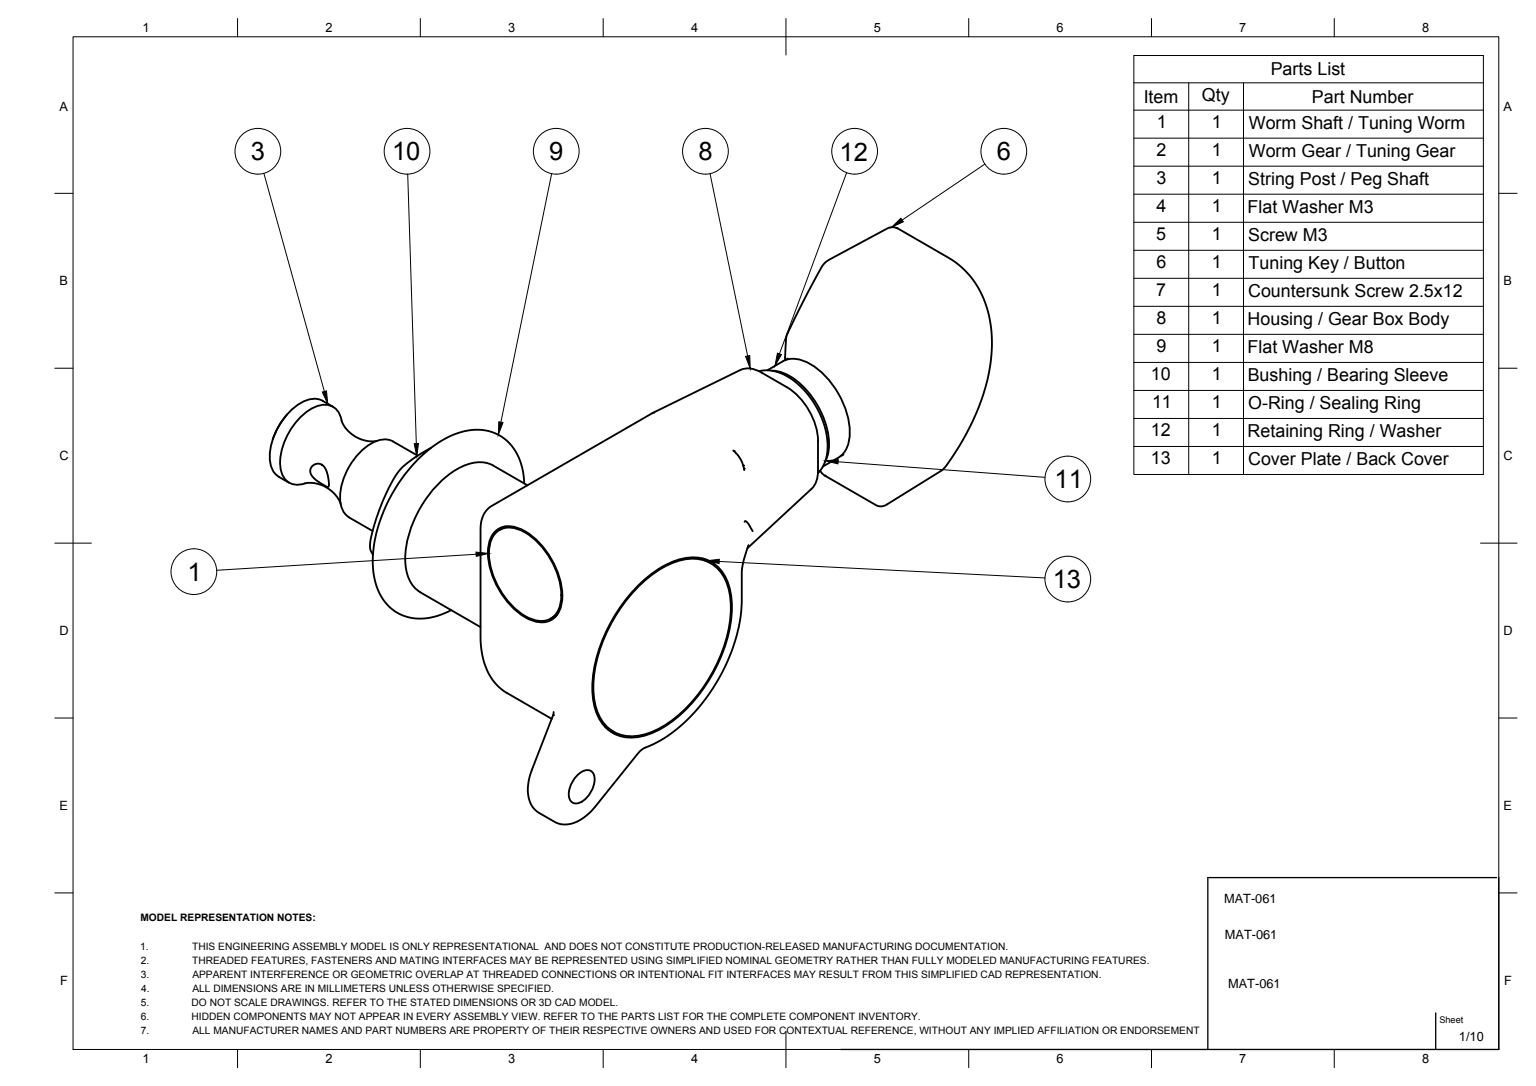
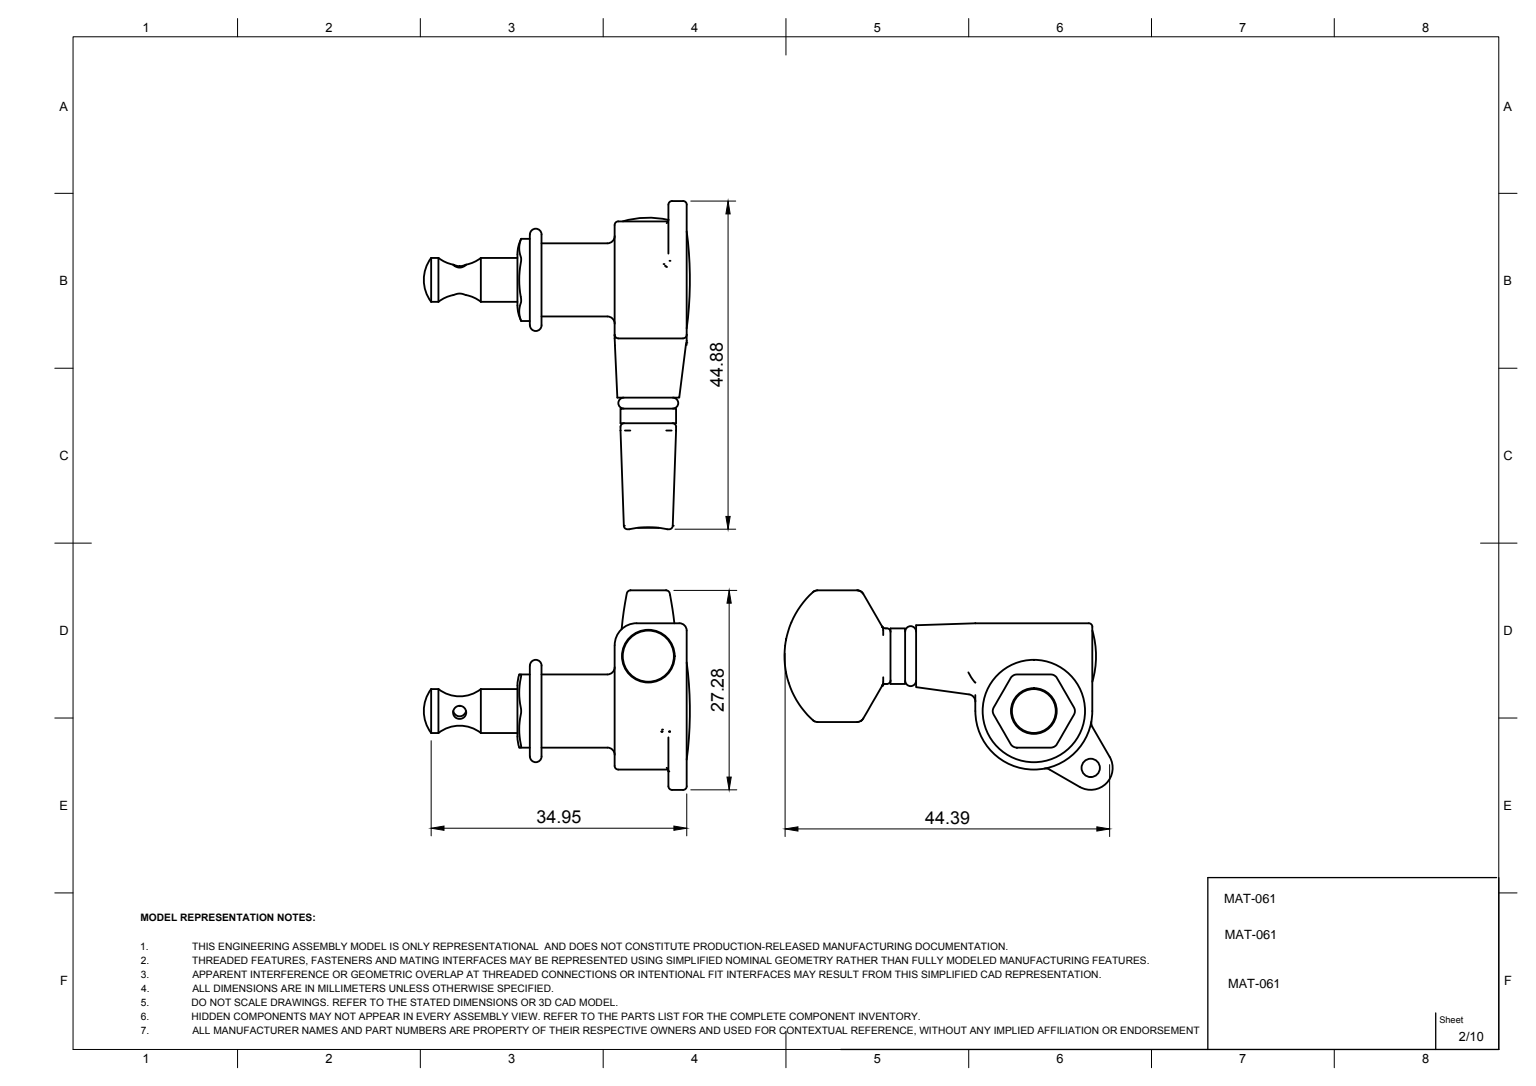
ISO-10303-21;
HEADER;
/* Generated by software containing ST-Developer
 * from STEP Tools, Inc. (www.steptools.com) 
 */

FILE_DESCRIPTION(
/* description */ ('', 'CAx-IF Rec.Pracs.---Representation and Presentation of Product Manufa
cturing Information (PMI)---4.0---2014-10-13'),
/* implementation_level */ '2;1');

FILE_NAME(
/* name */ 'MAT-061',
/* time_stamp */ '2026-10-28T14:45:12+01:00',
/* author */ (''),
/* organization */ (''),
/* preprocessor_version */ 'ST-DEVELOPER v20.2',
/* originating_system */ 'Autodesk Translation Framework v15.17.0.0',
/* authorisation */ '');

FILE_SCHEMA (('AP242_MANAGED_MODEL_BASED_3D_ENGINEERING_MIM_LF { 1 0 10303 442 2 1 4 }'));
ENDSEC;

DATA;
#10=MECHANICAL_DESIGN_GEOMETRIC_PRESENTATION_REPRESENTATION('',(#258,#259,
#260,#261,#262,#263,#264,#265,#266,#267,#268,#269,#270),#52164);
#11=ITEM_DEFINED_TRANSFORMATION($,$,#9276,#10197);
#12=ITEM_DEFINED_TRANSFORMATION($,$,#9302,#10198);
#13=ITEM_DEFINED_TRANSFORMATION($,$,#9667,#10199);
#14=ITEM_DEFINED_TRANSFORMATION($,$,#9694,#10200);
#15=ITEM_DEFINED_TRANSFORMATION($,$,#9704,#10201);
#16=ITEM_DEFINED_TRANSFORMATION($,$,#9776,#10202);
#17=ITEM_DEFINED_TRANSFORMATION($,$,#9921,#10203);
#18=ITEM_DEFINED_TRANSFORMATION($,$,#9987,#10204);
#19=ITEM_DEFINED_TRANSFORMATION($,$,#10132,#10205);
#20=ITEM_DEFINED_TRANSFORMATION($,$,#10142,#10206);
#21=ITEM_DEFINED_TRANSFORMATION($,$,#10171,#10207);
#22=ITEM_DEFINED_TRANSFORMATION($,$,#10175,#10208);
#23=ITEM_DEFINED_TRANSFORMATION($,$,#10184,#10209);
#24=(
REPRESENTATION_RELATIONSHIP($,$,#52211,#52210)
REPRESENTATION_RELATIONSHIP_WITH_TRANSFORMATION(#11)
SHAPE_REPRESENTATION_RELATIONSHIP()
);
#25=(
REPRESENTATION_RELATIONSHIP($,$,#52212,#52210)
REPRESENTATION_RELATIONSHIP_WITH_TRANSFORMATION(#12)
SHAPE_REPRESENTATION_RELATIONSHIP()
);
#26=(
REPRESENTATION_RELATIONSHIP($,$,#52213,#52210)
REPRESENTATION_RELATIONSHIP_WITH_TRANSFORMATION(#13)
SHAPE_REPRESENTATION_RELATIONSHIP()
);
#27=(
REPRESENTATION_RELATIONSHIP($,$,#52214,#52210)
REPRESENTATION_RELATIONSHIP_WITH_TRANSFORMATION(#14)
SHAPE_REPRESENTATION_RELATIONSHIP()
);
#28=(
REPRESENTATION_RELATIONSHIP($,$,#52215,#52210)
REPRESENTATION_RELATIONSHIP_WITH_TRANSFORMATION(#15)
SHAPE_REPRESENTATION_RELATIONSHIP()
);
#29=(
REPRESENTATION_RELATIONSHIP($,$,#52216,#52210)
REPRESENTATION_RELATIONSHIP_WITH_TRANSFORMATION(#16)
SHAPE_REPRESENTATION_RELATIONSHIP()
);
#30=(
REPRESENTATION_RELATIONSHIP($,$,#52217,#52210)
REPRESENTATION_RELATIONSHIP_WITH_TRANSFORMATION(#17)
SHAPE_REPRESENTATION_RELATIONSHIP()
);
#31=(
REPRESENTATION_RELATIONSHIP($,$,#52218,#52210)
REPRESENTATION_RELATIONSHIP_WITH_TRANSFORMATION(#18)
SHAPE_REPRESENTATION_RELATIONSHIP()
);
#32=(
REPRESENTATION_RELATIONSHIP($,$,#52219,#52210)
REPRESENTATION_RELATIONSHIP_WITH_TRANSFORMATION(#19)
SHAPE_REPRESENTATION_RELATIONSHIP()
);
#33=(
REPRESENTATION_RELATIONSHIP($,$,#52220,#52210)
REPRESENTATION_RELATIONSHIP_WITH_TRANSFORMATION(#20)
SHAPE_REPRESENTATION_RELATIONSHIP()
);
#34=(
REPRESENTATION_RELATIONSHIP($,$,#52221,#52210)
REPRESENTATION_RELATIONSHIP_WITH_TRANSFORMATION(#21)
SHAPE_REPRESENTATION_RELATIONSHIP()
);
#35=(
REPRESENTATION_RELATIONSHIP($,$,#52222,#52210)
REPRESENTATION_RELATIONSHIP_WITH_TRANSFORMATION(#22)
SHAPE_REPRESENTATION_RELATIONSHIP()
);
#36=(
REPRESENTATION_RELATIONSHIP($,$,#52223,#52210)
REPRESENTATION_RELATIONSHIP_WITH_TRANSFORMATION(#23)
SHAPE_REPRESENTATION_RELATIONSHIP()
);
#37=CONTEXT_DEPENDENT_SHAPE_REPRESENTATION(#24,#52197);
#38=CONTEXT_DEPENDENT_SHAPE_REPRESENTATION(#25,#52198);
#39=CONTEXT_DEPENDENT_SHAPE_REPRESENTATION(#26,#52199);
#40=CONTEXT_DEPENDENT_SHAPE_REPRESENTATION(#27,#52200);
#41=CONTEXT_DEPENDENT_SHAPE_REPRESENTATION(#28,#52201);
#42=CONTEXT_DEPENDENT_SHAPE_REPRESENTATION(#29,#52202);
#43=CONTEXT_DEPENDENT_SHAPE_REPRESENTATION(#30,#52203);
#44=CONTEXT_DEPENDENT_SHAPE_REPRESENTATION(#31,#52204);
#45=CONTEXT_DEPENDENT_SHAPE_REPRESENTATION(#32,#52205);
#46=CONTEXT_DEPENDENT_SHAPE_REPRESENTATION(#33,#52206);
#47=CONTEXT_DEPENDENT_SHAPE_REPRESENTATION(#34,#52207);
#48=CONTEXT_DEPENDENT_SHAPE_REPRESENTATION(#35,#52208);
#49=CONTEXT_DEPENDENT_SHAPE_REPRESENTATION(#36,#52209);
#50=NEXT_ASSEMBLY_USAGE_OCCURRENCE('Worm Shaft / Tuning Worm:1',
'Worm Shaft / Tuning Worm:1','Worm Shaft / Tuning Worm:1',#52225,#52226,
'Worm Shaft / Tuning Worm:1');
#51=NEXT_ASSEMBLY_USAGE_OCCURRENCE('Worm Gear / Tuning Gear:1',
'Worm Gear / Tuning Gear:1','Worm Gear / Tuning Gear:1',#52225,#52227,
'Worm Gear / Tuning Gear:1');
#52=NEXT_ASSEMBLY_USAGE_OCCURRENCE('String Post / Peg Shaft:1',
'String Post / Peg Shaft:1','String Post / Peg Shaft:1',#52225,#52228,
'String Post / Peg Shaft:1');
#53=NEXT_ASSEMBLY_USAGE_OCCURRENCE('Flat Washer M3:1',
'Flat Washer M3:1','Flat Washer M3:1',#52225,#52229,'Flat Washer M3:1');
#54=NEXT_ASSEMBLY_USAGE_OCCURRENCE('Screw M3:1','Screw M3:1',
'Screw M3:1',#52225,#52230,'Screw M3:1');
#55=NEXT_ASSEMBLY_USAGE_OCCURRENCE('Tuning Key / Button:1',
'Tuning Key / Button:1','Tuning Key / Button:1',#52225,#52231,
'Tuning Key / Button:1');
#56=NEXT_ASSEMBLY_USAGE_OCCURRENCE('Countersunk Screw 2.5x12:1',
'Countersunk Screw 2.5x12:1','Countersunk Screw 2.5x12:1',#52225,#52232,
'Countersunk Screw 2.5x12:1');
#57=NEXT_ASSEMBLY_USAGE_OCCURRENCE('Housing / Gear Box Body:1',
'Housing / Gear Box Body:1','Housing / Gear Box Body:1',#52225,#52233,
'Housing / Gear Box Body:1');
#58=NEXT_ASSEMBLY_USAGE_OCCURRENCE('Flat Washer M8:1',
'Flat Washer M8:1','Flat Washer M8:1',#52225,#52234,'Flat Washer M8:1');
#59=NEXT_ASSEMBLY_USAGE_OCCURRENCE('Bushing / Bearing Sleeve:1',
'Bushing / Bearing Sleeve:1','Bushing / Bearing Sleeve:1',#52225,#52235,
'Bushing / Bearing Sleeve:1');
#60=NEXT_ASSEMBLY_USAGE_OCCURRENCE('O-Ring / Sealing Ring:1',
'O-Ring / Sealing Ring:1','O-Ring / Sealing Ring:1',#52225,#52236,
'O-Ring / Sealing Ring:1');
#61=NEXT_ASSEMBLY_USAGE_OCCURRENCE('Retaining Ring / Washer:1',
'Retaining Ring / Washer:1','Retaining Ring / Washer:1',#52225,#52237,
'Retaining Ring / Washer:1');
#62=NEXT_ASSEMBLY_USAGE_OCCURRENCE('Cover Plate / Back Cover:1',
'Cover Plate / Back Cover:1','Cover Plate / Back Cover:1',#52225,#52238,
'Cover Plate / Back Cover:1');
#63=(
BOUNDED_CURVE()
B_SPLINE_CURVE(2,(#29010,#29011,#29012),.UNSPECIFIED.,.F.,.F.)
B_SPLINE_CURVE_WITH_KNOTS((3,3),(-1.41025055977478,-0.304692654014095),
 .UNSPECIFIED.)
CURVE()
GEOMETRIC_REPRESENTATION_ITEM()
RATIONAL_B_SPLINE_CURVE((0.957089080441345,0.830796931423118,1.))
REPRESENTATION_ITEM('')
);
#64=(
BOUNDED_CURVE()
B_SPLINE_CURVE(2,(#46348,#46349,#46350),.UNSPECIFIED.,.F.,.F.)
B_SPLINE_CURVE_WITH_KNOTS((3,3),(1.23956041519017,1.57079632679222),
 .UNSPECIFIED.)
CURVE()
GEOMETRIC_REPRESENTATION_ITEM()
RATIONAL_B_SPLINE_CURVE((0.987875274923375,0.980288238878012,1.))
REPRESENTATION_ITEM('')
);
#65=ELLIPSE('',#9725,0.771415586451778,0.0652711480392958);
#66=ELLIPSE('',#9726,0.771415586451778,0.0652711480392958);
#67=ELLIPSE('',#9729,0.771415586459596,0.0652711480406291);
#68=ELLIPSE('',#9733,0.251906298612587,0.25);
#69=ELLIPSE('',#9735,0.251906298612587,0.25);
#70=ELLIPSE('',#9736,0.251906298612587,0.25);
#71=ELLIPSE('',#9737,0.251906298612587,0.25);
#72=ELLIPSE('',#9738,0.251906298612587,0.25);
#73=ELLIPSE('',#9739,0.251906298612587,0.25);
#74=ELLIPSE('',#9740,0.251906298612587,0.25);
#75=ELLIPSE('',#9741,0.251906298612587,0.25);
#76=ELLIPSE('',#9742,0.251906298612587,0.25);
#77=ELLIPSE('',#9743,0.251906298612587,0.25);
#78=ELLIPSE('',#9744,0.251906298612587,0.25);
#79=ELLIPSE('',#9745,0.251906298612587,0.25);
#80=ELLIPSE('',#9748,0.251906298612587,0.25);
#81=ELLIPSE('',#9750,0.251906298612587,0.25);
#82=ELLIPSE('',#9752,0.251906298612587,0.25);
#83=ELLIPSE('',#9754,0.251906298612587,0.25);
#84=ELLIPSE('',#9778,3.41583409365519,0.299010553745989);
#85=ELLIPSE('',#9779,1.15925578938865,0.129764384341253);
#86=ELLIPSE('',#9810,58.0067380360385,50.6192841142981);
#87=ELLIPSE('',#9813,1.18656669130194,0.53832789407732);
#88=ELLIPSE('',#9814,2.36619692333918,0.2327676175482);
#89=ELLIPSE('',#9837,58.0426595105096,50.6800723424155);
#90=ELLIPSE('',#9844,57.8529892126302,50.3590102148563);
#91=ELLIPSE('',#9882,57.6813518726037,50.0696217347841);
#92=ELLIPSE('',#9924,0.251906298612587,0.25);
#93=ELLIPSE('',#9925,0.251906298612587,0.25);
#94=ELLIPSE('',#9926,0.251906298612587,0.25);
#95=ELLIPSE('',#9927,0.251906298612587,0.25);
#96=ELLIPSE('',#9928,0.251906298612587,0.25);
#97=ELLIPSE('',#9929,0.251906298612587,0.25);
#98=ELLIPSE('',#9930,0.251906298612587,0.25);
#99=ELLIPSE('',#9931,0.251906298612587,0.25);
#100=ELLIPSE('',#9932,0.251906298612587,0.25);
#101=ELLIPSE('',#9933,0.251906298612587,0.25);
#102=ELLIPSE('',#9934,0.251906298612587,0.25);
#103=ELLIPSE('',#9935,0.251906298612587,0.25);
#104=ELLIPSE('',#9951,0.251906298612587,0.25);
#105=ELLIPSE('',#9954,0.251906298612587,0.25);
#106=ELLIPSE('',#9955,0.251906298612587,0.25);
#107=ELLIPSE('',#9956,0.251906298612587,0.25);
#108=ELLIPSE('',#9957,0.251906298612587,0.25);
#109=ELLIPSE('',#9958,0.251906298612587,0.25);
#110=ELLIPSE('',#9959,0.251906298612587,0.25);
#111=ELLIPSE('',#9960,0.251906298612587,0.25);
#112=ELLIPSE('',#9961,0.251906298612587,0.25);
#113=ELLIPSE('',#9962,0.251906298612587,0.25);
#114=ELLIPSE('',#9963,0.251906298612587,0.25);
#115=ELLIPSE('',#9964,0.251906298612587,0.25);
#116=ELLIPSE('',#10069,3.09185060411887,2.99998911300292);
#117=ELLIPSE('',#10070,0.558356536433831,0.540529130211527);
#118=ELLIPSE('',#10075,3.02534560825415,3.);
#119=ELLIPSE('',#10096,3.05201365986006,3.);
#120=ELLIPSE('',#10097,3.03164154875039,3.);
#121=ELLIPSE('',#10098,3.00479269659654,3.);
#122=ELLIPSE('',#10104,3.05599112671771,2.99998273953943);
#123=ELLIPSE('',#10106,0.477842904086099,0.430473129723059);
#124=ELLIPSE('',#10110,0.470434252195438,0.436250539297532);
#125=ELLIPSE('',#10111,0.502233427925589,0.501933027798313);
#126=ELLIPSE('',#10115,0.0333294784166319,0.012380355937192);
#127=(
BOUNDED_SURFACE()
B_SPLINE_SURFACE(2,2,((#28929,#28930,#28931,#28932,#28933,#28934,#28935,
#28936,#28937),(#28938,#28939,#28940,#28941,#28942,#28943,#28944,#28945,
#28946),(#28947,#28948,#28949,#28950,#28951,#28952,#28953,#28954,#28955)),
 .UNSPECIFIED.,.F.,.T.,.F.)
B_SPLINE_SURFACE_WITH_KNOTS((3,3),(3,2,2,2,3),(0.304692654014095,1.57079632680149),
(-3.14159265358979,-1.5707963267949,0.,1.5707963267949,3.14159265358979),
 .UNSPECIFIED.)
GEOMETRIC_REPRESENTATION_ITEM()
RATIONAL_B_SPLINE_SURFACE(((1.,0.707106781186548,1.,0.707106781186548,1.,
0.707106781186548,1.,0.707106781186548,1.),(0.806225774827519,0.570087712547917,
0.806225774827519,0.570087712547917,0.806225774827519,0.570087712547917,
0.806225774827519,0.570087712547917,0.806225774827519),(1.,0.707106781186548,
1.,0.707106781186548,1.,0.707106781186548,1.,0.707106781186548,1.)))
REPRESENTATION_ITEM('')
SURFACE()
);
#128=(
BOUNDED_SURFACE()
B_SPLINE_SURFACE(3,3,((#29423,#29424,#29425,#29426,#29427,#29428,#29429,
#29430,#29431,#29432,#29433),(#29434,#29435,#29436,#29437,#29438,#29439,
#29440,#29441,#29442,#29443,#29444),(#29445,#29446,#29447,#29448,#29449,
#29450,#29451,#29452,#29453,#29454,#29455),(#29456,#29457,#29458,#29459,
#29460,#29461,#29462,#29463,#29464,#29465,#29466)),.UNSPECIFIED.,.F.,.F.,
 .F.)
B_SPLINE_SURFACE_WITH_KNOTS((4,4),(4,1,1,1,1,1,1,1,4),(0.,1.),(-0.02986974742742,
0.,0.1596527875626,0.3152888236561,0.4716393647845,0.6325142775716,0.8056128321368,
1.,1.030037265102),.UNSPECIFIED.)
GEOMETRIC_REPRESENTATION_ITEM()
RATIONAL_B_SPLINE_SURFACE(((1.021500558569,1.021500558569,1.021500558569,
1.021500558569,1.021500558569,1.021500558569,1.021500558569,1.021500558569,
1.021500558569,1.021500558569,1.021500558569),(0.9928331471435,0.9928331471435,
0.9928331471435,0.9928331471435,0.9928331471435,0.9928331471435,0.9928331471435,
0.9928331471435,0.9928331471435,0.9928331471435,0.9928331471435),(0.9928331471435,
0.9928331471435,0.9928331471435,0.9928331471435,0.9928331471435,0.9928331471435,
0.9928331471435,0.9928331471435,0.9928331471435,0.9928331471435,0.9928331471435),
(1.021500558569,1.021500558569,1.021500558569,1.021500558569,1.021500558569,
1.021500558569,1.021500558569,1.021500558569,1.021500558569,1.021500558569,
1.021500558569)))
REPRESENTATION_ITEM('')
SURFACE()
);
#129=(
BOUNDED_SURFACE()
B_SPLINE_SURFACE(3,3,((#29522,#29523,#29524,#29525,#29526,#29527,#29528,
#29529,#29530),(#29531,#29532,#29533,#29534,#29535,#29536,#29537,#29538,
#29539),(#29540,#29541,#29542,#29543,#29544,#29545,#29546,#29547,#29548),
(#29549,#29550,#29551,#29552,#29553,#29554,#29555,#29556,#29557)),
 .UNSPECIFIED.,.F.,.F.,.F.)
B_SPLINE_SURFACE_WITH_KNOTS((4,4),(4,1,1,1,1,1,4),(0.,1.),(-0.01572041923322,
0.,0.2489956052111,0.4846339404094,0.7277879443756,1.,1.015767529497),
 .UNSPECIFIED.)
GEOMETRIC_REPRESENTATION_ITEM()
RATIONAL_B_SPLINE_SURFACE(((1.20167030075,1.20167030075,1.20167030075,1.20167030075,
1.20167030075,1.20167030075,1.20167030075,1.20167030075,1.20167030075),
(0.9327765664168,0.9327765664168,0.9327765664168,0.9327765664168,0.9327765664168,
0.9327765664168,0.9327765664168,0.9327765664168,0.9327765664168),(0.9327765664168,
0.9327765664168,0.9327765664168,0.9327765664168,0.9327765664168,0.9327765664168,
0.9327765664168,0.9327765664168,0.9327765664168),(1.20167030075,1.20167030075,
1.20167030075,1.20167030075,1.20167030075,1.20167030075,1.20167030075,1.20167030075,
1.20167030075)))
REPRESENTATION_ITEM('')
SURFACE()
);
#130=(
BOUNDED_SURFACE()
B_SPLINE_SURFACE(3,3,((#29629,#29630,#29631,#29632,#29633,#29634,#29635,
#29636,#29637),(#29638,#29639,#29640,#29641,#29642,#29643,#29644,#29645,
#29646),(#29647,#29648,#29649,#29650,#29651,#29652,#29653,#29654,#29655),
(#29656,#29657,#29658,#29659,#29660,#29661,#29662,#29663,#29664)),
 .UNSPECIFIED.,.F.,.F.,.F.)
B_SPLINE_SURFACE_WITH_KNOTS((4,4),(4,1,1,1,1,1,4),(0.,1.),(-0.05556040640744,
0.,0.2510807745895,0.5005021153997,0.7496749190056,1.,1.055704479788),
 .UNSPECIFIED.)
GEOMETRIC_REPRESENTATION_ITEM()
RATIONAL_B_SPLINE_SURFACE(((1.211236736652,1.211236736652,1.211236736652,
1.211236736652,1.211236736652,1.211236736652,1.211236736652,1.211236736652,
1.211236736652),(0.9295877544494,0.9295877544494,0.9295877544494,0.9295877544494,
0.9295877544494,0.9295877544494,0.9295877544494,0.9295877544494,0.9295877544494),
(0.9295877544494,0.9295877544494,0.9295877544494,0.9295877544494,0.9295877544494,
0.9295877544494,0.9295877544494,0.9295877544494,0.9295877544494),(1.211236736652,
1.211236736652,1.211236736652,1.211236736652,1.211236736652,1.211236736652,
1.211236736652,1.211236736652,1.211236736652)))
REPRESENTATION_ITEM('')
SURFACE()
);
#131=(
BOUNDED_SURFACE()
B_SPLINE_SURFACE(3,3,((#29668,#29669,#29670,#29671,#29672,#29673,#29674,
#29675),(#29676,#29677,#29678,#29679,#29680,#29681,#29682,#29683),(#29684,
#29685,#29686,#29687,#29688,#29689,#29690,#29691),(#29692,#29693,#29694,
#29695,#29696,#29697,#29698,#29699)),.UNSPECIFIED.,.F.,.F.,.F.)
B_SPLINE_SURFACE_WITH_KNOTS((4,4),(4,1,1,1,1,4),(0.,1.),(0.8911674115136,
0.9072696780606,0.9355241084298,0.9657104248281,1.,1.001077582608),
 .UNSPECIFIED.)
GEOMETRIC_REPRESENTATION_ITEM()
RATIONAL_B_SPLINE_SURFACE(((1.199526961773,1.199526961773,1.199526961773,
1.199526961773,1.199526961773,1.199526961773,1.199526961773,1.199526961773),
(0.9334910127424,0.9334910127424,0.9334910127424,0.9334910127424,0.9334910127424,
0.9334910127424,0.9334910127424,0.9334910127424),(0.9334910127424,0.9334910127424,
0.9334910127424,0.9334910127424,0.9334910127424,0.9334910127424,0.9334910127424,
0.9334910127424),(1.199526961773,1.199526961773,1.199526961773,1.199526961773,
1.199526961773,1.199526961773,1.199526961773,1.199526961773)))
REPRESENTATION_ITEM('')
SURFACE()
);
#132=(
BOUNDED_SURFACE()
B_SPLINE_SURFACE(3,3,((#29815,#29816,#29817,#29818,#29819,#29820,#29821,
#29822,#29823,#29824,#29825),(#29826,#29827,#29828,#29829,#29830,#29831,
#29832,#29833,#29834,#29835,#29836),(#29837,#29838,#29839,#29840,#29841,
#29842,#29843,#29844,#29845,#29846,#29847),(#29848,#29849,#29850,#29851,
#29852,#29853,#29854,#29855,#29856,#29857,#29858)),.UNSPECIFIED.,.F.,.F.,
 .F.)
B_SPLINE_SURFACE_WITH_KNOTS((4,4),(4,1,1,1,1,1,1,1,4),(0.,1.),(-0.05042394646536,
0.,0.169599833297,0.3375196990485,0.507342039377,0.6686225111424,0.8285344877041,
1.,1.040577583792),.UNSPECIFIED.)
GEOMETRIC_REPRESENTATION_ITEM()
RATIONAL_B_SPLINE_SURFACE(((1.008087174025,1.008087174025,1.008087174025,
1.008087174025,1.008087174025,1.008087174025,1.008087174025,1.008087174025,
1.008087174025,1.008087174025,1.008087174025),(0.9973042753251,0.9973042753251,
0.9973042753251,0.9973042753251,0.9973042753251,0.9973042753251,0.9973042753251,
0.9973042753251,0.9973042753251,0.9973042753251,0.9973042753251),(0.9973042753251,
0.9973042753251,0.9973042753251,0.9973042753251,0.9973042753251,0.9973042753251,
0.9973042753251,0.9973042753251,0.9973042753251,0.9973042753251,0.9973042753251),
(1.008087174025,1.008087174025,1.008087174025,1.008087174025,1.008087174025,
1.008087174025,1.008087174025,1.008087174025,1.008087174025,1.008087174025,
1.008087174025)))
REPRESENTATION_ITEM('')
SURFACE()
);
#133=(
BOUNDED_SURFACE()
B_SPLINE_SURFACE(3,3,((#29905,#29906,#29907,#29908,#29909,#29910,#29911),
(#29912,#29913,#29914,#29915,#29916,#29917,#29918),(#29919,#29920,#29921,
#29922,#29923,#29924,#29925),(#29926,#29927,#29928,#29929,#29930,#29931,
#29932)),.UNSPECIFIED.,.F.,.F.,.F.)
B_SPLINE_SURFACE_WITH_KNOTS((4,4),(4,1,1,1,4),(0.,1.),(0.112613801722,0.3198611143952,
0.6533271535514,1.,1.02662543373),.UNSPECIFIED.)
GEOMETRIC_REPRESENTATION_ITEM()
RATIONAL_B_SPLINE_SURFACE(((1.133923634678,1.133923634678,1.133923634678,
1.133923634678,1.133923634678,1.133923634678,1.133923634678),(0.9553587884407,
0.9553587884407,0.9553587884407,0.9553587884407,0.9553587884407,0.9553587884407,
0.9553587884407),(0.9553587884407,0.9553587884407,0.9553587884407,0.9553587884407,
0.9553587884407,0.9553587884407,0.9553587884407),(1.133923634678,1.133923634678,
1.133923634678,1.133923634678,1.133923634678,1.133923634678,1.133923634678)))
REPRESENTATION_ITEM('')
SURFACE()
);
#134=(
BOUNDED_SURFACE()
B_SPLINE_SURFACE(3,3,((#30489,#30490,#30491,#30492,#30493,#30494,#30495,
#30496,#30497,#30498,#30499,#30500,#30501,#30502,#30503,#30504,#30505,#30506,
#30507),(#30508,#30509,#30510,#30511,#30512,#30513,#30514,#30515,#30516,
#30517,#30518,#30519,#30520,#30521,#30522,#30523,#30524,#30525,#30526),
(#30527,#30528,#30529,#30530,#30531,#30532,#30533,#30534,#30535,#30536,
#30537,#30538,#30539,#30540,#30541,#30542,#30543,#30544,#30545),(#30546,
#30547,#30548,#30549,#30550,#30551,#30552,#30553,#30554,#30555,#30556,#30557,
#30558,#30559,#30560,#30561,#30562,#30563,#30564)),.UNSPECIFIED.,.F.,.F.,
 .F.)
B_SPLINE_SURFACE_WITH_KNOTS((4,4),(4,1,1,1,1,1,1,1,1,1,1,1,1,1,1,1,4),(0.,
1.),(-0.01076426746052,0.,0.04152389901163,0.08394379225383,0.1302342687653,
0.1804523447143,0.2349355052965,0.2939338029968,0.3580057487009,0.4275129366519,
0.5025423241298,0.5839356639567,0.6731830882241,0.771794295847,0.880557504522,
1.,1.009808133051),.UNSPECIFIED.)
GEOMETRIC_REPRESENTATION_ITEM()
RATIONAL_B_SPLINE_SURFACE(((1.088372924818,1.088372924818,1.088372924818,
1.088372924818,1.088372924818,1.088372924818,1.088372924818,1.088372924818,
1.088372924818,1.088372924818,1.088372924818,1.088372924818,1.088372924818,
1.088372924818,1.088372924818,1.088372924818,1.088372924818,1.088372924818,
1.088372924818),(0.9705423583942,0.9705423583942,0.9705423583942,0.9705423583942,
0.9705423583942,0.9705423583942,0.9705423583942,0.9705423583942,0.9705423583942,
0.9705423583942,0.9705423583942,0.9705423583942,0.9705423583942,0.9705423583942,
0.9705423583942,0.9705423583942,0.9705423583942,0.9705423583942,0.9705423583942),
(0.9705423583942,0.9705423583942,0.9705423583942,0.9705423583942,0.9705423583942,
0.9705423583942,0.9705423583942,0.9705423583942,0.9705423583942,0.9705423583942,
0.9705423583942,0.9705423583942,0.9705423583942,0.9705423583942,0.9705423583942,
0.9705423583942,0.9705423583942,0.9705423583942,0.9705423583942),(1.088372924818,
1.088372924818,1.088372924818,1.088372924818,1.088372924818,1.088372924818,
1.088372924818,1.088372924818,1.088372924818,1.088372924818,1.088372924818,
1.088372924818,1.088372924818,1.088372924818,1.088372924818,1.088372924818,
1.088372924818,1.088372924818,1.088372924818)))
REPRESENTATION_ITEM('')
SURFACE()
);
#135=(
BOUNDED_SURFACE()
B_SPLINE_SURFACE(3,3,((#30667,#30668,#30669,#30670,#30671,#30672,#30673,
#30674,#30675,#30676),(#30677,#30678,#30679,#30680,#30681,#30682,#30683,
#30684,#30685,#30686),(#30687,#30688,#30689,#30690,#30691,#30692,#30693,
#30694,#30695,#30696),(#30697,#30698,#30699,#30700,#30701,#30702,#30703,
#30704,#30705,#30706)),.UNSPECIFIED.,.F.,.F.,.F.)
B_SPLINE_SURFACE_WITH_KNOTS((4,4),(4,1,1,1,1,1,1,4),(0.,1.),(0.03540281776569,
0.1234679415061,0.2632035734035,0.4203296727883,0.5957836491344,0.7892685013705,
1.,1.00911688994),.UNSPECIFIED.)
GEOMETRIC_REPRESENTATION_ITEM()
RATIONAL_B_SPLINE_SURFACE(((1.211236248281,1.211236248281,1.211236248281,
1.211236248281,1.211236248281,1.211236248281,1.211236248281,1.211236248281,
1.211236248281,1.211236248281),(0.9295879172397,0.9295879172397,0.9295879172397,
0.9295879172397,0.9295879172397,0.9295879172397,0.9295879172397,0.9295879172397,
0.9295879172397,0.9295879172397),(0.9295879172397,0.9295879172397,0.9295879172397,
0.9295879172397,0.9295879172397,0.9295879172397,0.9295879172397,0.9295879172397,
0.9295879172397,0.9295879172397),(1.211236248281,1.211236248281,1.211236248281,
1.211236248281,1.211236248281,1.211236248281,1.211236248281,1.211236248281,
1.211236248281,1.211236248281)))
REPRESENTATION_ITEM('')
SURFACE()
);
#136=(
BOUNDED_SURFACE()
B_SPLINE_SURFACE(3,3,((#30720,#30721,#30722,#30723,#30724,#30725,#30726,
#30727,#30728,#30729,#30730,#30731),(#30732,#30733,#30734,#30735,#30736,
#30737,#30738,#30739,#30740,#30741,#30742,#30743),(#30744,#30745,#30746,
#30747,#30748,#30749,#30750,#30751,#30752,#30753,#30754,#30755),(#30756,
#30757,#30758,#30759,#30760,#30761,#30762,#30763,#30764,#30765,#30766,#30767)),
 .UNSPECIFIED.,.F.,.F.,.F.)
B_SPLINE_SURFACE_WITH_KNOTS((4,4),(4,1,1,1,1,1,1,1,1,4),(0.,1.),(-0.1526180119247,
0.,0.1440925301464,0.2801219903111,0.411439159359,0.5434056701394,0.683264528579,
0.8346596058499,1.,1.152833582057),.UNSPECIFIED.)
GEOMETRIC_REPRESENTATION_ITEM()
RATIONAL_B_SPLINE_SURFACE(((1.000094023891,1.000094023891,1.000094023891,
1.000094023891,1.000094023891,1.000094023891,1.000094023891,1.000094023891,
1.000094023891,1.000094023891,1.000094023891,1.000094023891),(0.9999686587029,
0.9999686587029,0.9999686587029,0.9999686587029,0.9999686587029,0.9999686587029,
0.9999686587029,0.9999686587029,0.9999686587029,0.9999686587029,0.9999686587029,
0.9999686587029),(0.9999686587029,0.9999686587029,0.9999686587029,0.9999686587029,
0.9999686587029,0.9999686587029,0.9999686587029,0.9999686587029,0.9999686587029,
0.9999686587029,0.9999686587029,0.9999686587029),(1.000094023891,1.000094023891,
1.000094023891,1.000094023891,1.000094023891,1.000094023891,1.000094023891,
1.000094023891,1.000094023891,1.000094023891,1.000094023891,1.000094023891)))
REPRESENTATION_ITEM('')
SURFACE()
);
#137=(
BOUNDED_SURFACE()
B_SPLINE_SURFACE(3,3,((#30792,#30793,#30794,#30795,#30796,#30797,#30798,
#30799,#30800,#30801),(#30802,#30803,#30804,#30805,#30806,#30807,#30808,
#30809,#30810,#30811),(#30812,#30813,#30814,#30815,#30816,#30817,#30818,
#30819,#30820,#30821),(#30822,#30823,#30824,#30825,#30826,#30827,#30828,
#30829,#30830,#30831)),.UNSPECIFIED.,.F.,.F.,.F.)
B_SPLINE_SURFACE_WITH_KNOTS((4,4),(4,1,1,1,1,1,1,4),(0.,1.),(-0.009053405764055,
0.,0.2128253131464,0.406710340465,0.5817418357976,0.7383188923361,0.8773475428248,
0.9585687317144),.UNSPECIFIED.)
GEOMETRIC_REPRESENTATION_ITEM()
RATIONAL_B_SPLINE_SURFACE(((1.211237524847,1.211237524847,1.211237524847,
1.211237524847,1.211237524847,1.211237524847,1.211237524847,1.211237524847,
1.211237524847,1.211237524847),(0.9295874917176,0.9295874917176,0.9295874917176,
0.9295874917176,0.9295874917176,0.9295874917176,0.9295874917176,0.9295874917176,
0.9295874917176,0.9295874917176),(0.9295874917176,0.9295874917176,0.9295874917176,
0.9295874917176,0.9295874917176,0.9295874917176,0.9295874917176,0.9295874917176,
0.9295874917176,0.9295874917176),(1.211237524847,1.211237524847,1.211237524847,
1.211237524847,1.211237524847,1.211237524847,1.211237524847,1.211237524847,
1.211237524847,1.211237524847)))
REPRESENTATION_ITEM('')
SURFACE()
);
#138=(
BOUNDED_SURFACE()
B_SPLINE_SURFACE(3,3,((#30920,#30921,#30922,#30923,#30924,#30925,#30926,
#30927,#30928,#30929,#30930,#30931,#30932,#30933,#30934,#30935,#30936,#30937),
(#30938,#30939,#30940,#30941,#30942,#30943,#30944,#30945,#30946,#30947,
#30948,#30949,#30950,#30951,#30952,#30953,#30954,#30955),(#30956,#30957,
#30958,#30959,#30960,#30961,#30962,#30963,#30964,#30965,#30966,#30967,#30968,
#30969,#30970,#30971,#30972,#30973),(#30974,#30975,#30976,#30977,#30978,
#30979,#30980,#30981,#30982,#30983,#30984,#30985,#30986,#30987,#30988,#30989,
#30990,#30991)),.UNSPECIFIED.,.F.,.F.,.F.)
B_SPLINE_SURFACE_WITH_KNOTS((4,4),(4,1,1,1,1,1,1,1,1,1,1,1,1,1,1,4),(0.,
1.),(-0.009797090891185,0.,0.1252864769206,0.2381332273305,0.3395214867104,
0.4311702756132,0.514794596407,0.5913458810939,0.661337900673,0.7254151205028,
0.7843391271164,0.8380935847788,0.8886737238569,0.9411160876018,1.,1.010696795736),
 .UNSPECIFIED.)
GEOMETRIC_REPRESENTATION_ITEM()
RATIONAL_B_SPLINE_SURFACE(((1.088374512803,1.088374512803,1.088374512803,
1.088374512803,1.088374512803,1.088374512803,1.088374512803,1.088374512803,
1.088374512803,1.088374512803,1.088374512803,1.088374512803,1.088374512803,
1.088374512803,1.088374512803,1.088374512803,1.088374512803,1.088374512803),
(0.9705418290656,0.9705418290656,0.9705418290656,0.9705418290656,0.9705418290656,
0.9705418290656,0.9705418290656,0.9705418290655,0.9705418290656,0.9705418290656,
0.9705418290656,0.9705418290656,0.9705418290655,0.9705418290656,0.9705418290656,
0.9705418290655,0.9705418290656,0.9705418290656),(0.9705418290656,0.9705418290656,
0.9705418290656,0.9705418290656,0.9705418290656,0.9705418290656,0.9705418290656,
0.9705418290655,0.9705418290656,0.9705418290656,0.9705418290656,0.9705418290656,
0.9705418290655,0.9705418290656,0.9705418290656,0.9705418290655,0.9705418290656,
0.9705418290656),(1.088374512803,1.088374512803,1.088374512803,1.088374512803,
1.088374512803,1.088374512803,1.088374512803,1.088374512803,1.088374512803,
1.088374512803,1.088374512803,1.088374512803,1.088374512803,1.088374512803,
1.088374512803,1.088374512803,1.088374512803,1.088374512803)))
REPRESENTATION_ITEM('')
SURFACE()
);
#139=(
BOUNDED_SURFACE()
B_SPLINE_SURFACE(3,3,((#30993,#30994,#30995,#30996,#30997,#30998,#30999,
#31000,#31001),(#31002,#31003,#31004,#31005,#31006,#31007,#31008,#31009,
#31010),(#31011,#31012,#31013,#31014,#31015,#31016,#31017,#31018,#31019),
(#31020,#31021,#31022,#31023,#31024,#31025,#31026,#31027,#31028)),
 .UNSPECIFIED.,.F.,.F.,.F.)
B_SPLINE_SURFACE_WITH_KNOTS((4,4),(4,1,1,1,1,1,4),(0.,1.),(-0.01572041923323,
0.,0.2489956052094,0.4846339404077,0.7277879443747,1.,1.015767529497),
 .UNSPECIFIED.)
GEOMETRIC_REPRESENTATION_ITEM()
RATIONAL_B_SPLINE_SURFACE(((1.20167030075,1.20167030075,1.20167030075,1.20167030075,
1.20167030075,1.20167030075,1.20167030075,1.20167030075,1.20167030075),
(0.9327765664168,0.9327765664168,0.9327765664168,0.9327765664168,0.9327765664168,
0.9327765664168,0.9327765664168,0.9327765664168,0.9327765664168),(0.9327765664168,
0.9327765664168,0.9327765664168,0.9327765664168,0.9327765664168,0.9327765664168,
0.9327765664168,0.9327765664168,0.9327765664168),(1.20167030075,1.20167030075,
1.20167030075,1.20167030075,1.20167030075,1.20167030075,1.20167030075,1.20167030075,
1.20167030075)))
REPRESENTATION_ITEM('')
SURFACE()
);
#140=(
BOUNDED_SURFACE()
B_SPLINE_SURFACE(3,3,((#31065,#31066,#31067,#31068,#31069,#31070,#31071,
#31072,#31073),(#31074,#31075,#31076,#31077,#31078,#31079,#31080,#31081,
#31082),(#31083,#31084,#31085,#31086,#31087,#31088,#31089,#31090,#31091),
(#31092,#31093,#31094,#31095,#31096,#31097,#31098,#31099,#31100)),
 .UNSPECIFIED.,.F.,.F.,.F.)
B_SPLINE_SURFACE_WITH_KNOTS((4,4),(4,1,1,1,1,1,4),(0.,1.),(-0.05556027674448,
0.,0.2486256441043,0.4972385660022,0.747219976182,1.,1.055704281495),
 .UNSPECIFIED.)
GEOMETRIC_REPRESENTATION_ITEM()
RATIONAL_B_SPLINE_SURFACE(((1.211236736616,1.211236736616,1.211236736616,
1.211236736616,1.211236736616,1.211236736616,1.211236736616,1.211236736616,
1.211236736616),(0.9295877544614,0.9295877544614,0.9295877544614,0.9295877544614,
0.9295877544614,0.9295877544614,0.9295877544614,0.9295877544614,0.9295877544614),
(0.9295877544614,0.9295877544614,0.9295877544614,0.9295877544614,0.9295877544614,
0.9295877544614,0.9295877544614,0.9295877544614,0.9295877544614),(1.211236736616,
1.211236736616,1.211236736616,1.211236736616,1.211236736616,1.211236736616,
1.211236736616,1.211236736616,1.211236736616)))
REPRESENTATION_ITEM('')
SURFACE()
);
#141=(
BOUNDED_SURFACE()
B_SPLINE_SURFACE(3,3,((#31104,#31105,#31106,#31107,#31108,#31109,#31110,
#31111),(#31112,#31113,#31114,#31115,#31116,#31117,#31118,#31119),(#31120,
#31121,#31122,#31123,#31124,#31125,#31126,#31127),(#31128,#31129,#31130,
#31131,#31132,#31133,#31134,#31135)),.UNSPECIFIED.,.F.,.F.,.F.)
B_SPLINE_SURFACE_WITH_KNOTS((4,4),(4,1,1,1,1,4),(0.,1.),(0.8864361758264,
0.9023348460698,0.9320880776135,0.9638776326039,1.,1.001124438805),
 .UNSPECIFIED.)
GEOMETRIC_REPRESENTATION_ITEM()
RATIONAL_B_SPLINE_SURFACE(((1.199526961777,1.199526961777,1.199526961777,
1.199526961777,1.199526961777,1.199526961777,1.199526961777,1.199526961777),
(0.933491012741,0.933491012741,0.933491012741,0.933491012741,0.933491012741,
0.933491012741,0.933491012741,0.933491012741),(0.933491012741,0.933491012741,
0.933491012741,0.933491012741,0.933491012741,0.933491012741,0.933491012741,
0.933491012741),(1.199526961777,1.199526961777,1.199526961777,1.199526961777,
1.199526961777,1.199526961777,1.199526961777,1.199526961777)))
REPRESENTATION_ITEM('')
SURFACE()
);
#142=(
BOUNDED_SURFACE()
B_SPLINE_SURFACE(3,3,((#31139,#31140,#31141,#31142,#31143,#31144,#31145,
#31146,#31147,#31148),(#31149,#31150,#31151,#31152,#31153,#31154,#31155,
#31156,#31157,#31158),(#31159,#31160,#31161,#31162,#31163,#31164,#31165,
#31166,#31167,#31168),(#31169,#31170,#31171,#31172,#31173,#31174,#31175,
#31176,#31177,#31178)),.UNSPECIFIED.,.F.,.F.,.F.)
B_SPLINE_SURFACE_WITH_KNOTS((4,4),(4,1,1,1,1,1,1,4),(0.,1.),(-0.02782802324678,
0.,0.206830483526,0.4072723973775,0.5982739087583,0.7917037265225,1.,1.028080129965),
 .UNSPECIFIED.)
GEOMETRIC_REPRESENTATION_ITEM()
RATIONAL_B_SPLINE_SURFACE(((1.187634479555,1.187634479555,1.187634479555,
1.187634479555,1.187634479555,1.187634479555,1.187634479555,1.187634479555,
1.187634479555,1.187634479555),(0.9374551734818,0.9374551734818,0.9374551734818,
0.9374551734818,0.9374551734818,0.9374551734818,0.9374551734818,0.9374551734818,
0.9374551734818,0.9374551734818),(0.9374551734818,0.9374551734818,0.9374551734818,
0.9374551734818,0.9374551734818,0.9374551734818,0.9374551734818,0.9374551734818,
0.9374551734818,0.9374551734818),(1.187634479555,1.187634479555,1.187634479555,
1.187634479555,1.187634479555,1.187634479555,1.187634479555,1.187634479555,
1.187634479555,1.187634479555)))
REPRESENTATION_ITEM('')
SURFACE()
);
#143=(
BOUNDED_SURFACE()
B_SPLINE_SURFACE(3,3,((#31284,#31285,#31286,#31287,#31288,#31289,#31290,
#31291,#31292,#31293),(#31294,#31295,#31296,#31297,#31298,#31299,#31300,
#31301,#31302,#31303),(#31304,#31305,#31306,#31307,#31308,#31309,#31310,
#31311,#31312,#31313),(#31314,#31315,#31316,#31317,#31318,#31319,#31320,
#31321,#31322,#31323)),.UNSPECIFIED.,.F.,.F.,.F.)
B_SPLINE_SURFACE_WITH_KNOTS((4,4),(4,1,1,1,1,1,1,4),(0.,1.),(-0.02810100933582,
0.,0.2037887769512,0.4025777380169,0.5941765368876,0.7898232262628,1.,1.027817051165),
 .UNSPECIFIED.)
GEOMETRIC_REPRESENTATION_ITEM()
RATIONAL_B_SPLINE_SURFACE(((1.18763448144,1.18763448144,1.18763448144,1.18763448144,
1.18763448144,1.18763448144,1.18763448144,1.18763448144,1.18763448144,1.18763448144),
(0.9374551728533,0.9374551728533,0.9374551728533,0.9374551728533,0.9374551728533,
0.9374551728533,0.9374551728533,0.9374551728533,0.9374551728533,0.9374551728533),
(0.9374551728533,0.9374551728533,0.9374551728533,0.9374551728533,0.9374551728533,
0.9374551728533,0.9374551728533,0.9374551728533,0.9374551728533,0.9374551728533),
(1.18763448144,1.18763448144,1.18763448144,1.18763448144,1.18763448144,
1.18763448144,1.18763448144,1.18763448144,1.18763448144,1.18763448144)))
REPRESENTATION_ITEM('')
SURFACE()
);
#144=(
BOUNDED_SURFACE()
B_SPLINE_SURFACE(3,3,((#31368,#31369,#31370,#31371,#31372,#31373,#31374,
#31375),(#31376,#31377,#31378,#31379,#31380,#31381,#31382,#31383),(#31384,
#31385,#31386,#31387,#31388,#31389,#31390,#31391),(#31392,#31393,#31394,
#31395,#31396,#31397,#31398,#31399)),.UNSPECIFIED.,.F.,.F.,.F.)
B_SPLINE_SURFACE_WITH_KNOTS((4,4),(4,1,1,1,1,4),(0.,1.),(-0.001124474187882,
0.,0.0292220127923,0.0587438887651,0.09152259808643,0.1135644482631),
 .UNSPECIFIED.)
GEOMETRIC_REPRESENTATION_ITEM()
RATIONAL_B_SPLINE_SURFACE(((1.199526978638,1.199526978638,1.199526978638,
1.199526978638,1.199526978638,1.199526978638,1.199526978638,1.199526978638),
(0.9334910071206,0.9334910071206,0.9334910071206,0.9334910071206,0.9334910071206,
0.9334910071206,0.9334910071206,0.9334910071206),(0.9334910071206,0.9334910071206,
0.9334910071206,0.9334910071206,0.9334910071206,0.9334910071206,0.9334910071206,
0.9334910071206),(1.199526978638,1.199526978638,1.199526978638,1.199526978638,
1.199526978638,1.199526978638,1.199526978638,1.199526978638)))
REPRESENTATION_ITEM('')
SURFACE()
);
#145=(
BOUNDED_SURFACE()
B_SPLINE_SURFACE(3,3,((#31403,#31404,#31405,#31406,#31407,#31408,#31409,
#31410,#31411,#31412,#31413,#31414),(#31415,#31416,#31417,#31418,#31419,
#31420,#31421,#31422,#31423,#31424,#31425,#31426),(#31427,#31428,#31429,
#31430,#31431,#31432,#31433,#31434,#31435,#31436,#31437,#31438),(#31439,
#31440,#31441,#31442,#31443,#31444,#31445,#31446,#31447,#31448,#31449,#31450)),
 .UNSPECIFIED.,.F.,.F.,.F.)
B_SPLINE_SURFACE_WITH_KNOTS((4,4),(4,1,1,1,1,1,1,1,1,4),(0.,1.),(0.01735834385764,
0.1111047299147,0.222221140213,0.3333544708185,0.4444847206802,0.5555988587856,
0.6667216990803,0.777841116212,0.8889364520316,0.9880643576882),
 .UNSPECIFIED.)
GEOMETRIC_REPRESENTATION_ITEM()
RATIONAL_B_SPLINE_SURFACE(((1.211236726429,1.211236726429,1.211236726429,
1.211236726429,1.211236726429,1.211236726429,1.211236726429,1.211236726429,
1.211236726429,1.211236726429,1.211236726429,1.211236726429),(0.929587757857,
0.929587757857,0.929587757857,0.929587757857,0.929587757857,0.929587757857,
0.929587757857,0.929587757857,0.929587757857,0.929587757857,0.929587757857,
0.929587757857),(0.929587757857,0.929587757857,0.929587757857,0.929587757857,
0.929587757857,0.929587757857,0.929587757857,0.929587757857,0.929587757857,
0.929587757857,0.929587757857,0.929587757857),(1.211236726429,1.211236726429,
1.211236726429,1.211236726429,1.211236726429,1.211236726429,1.211236726429,
1.211236726429,1.211236726429,1.211236726429,1.211236726429,1.211236726429)))
REPRESENTATION_ITEM('')
SURFACE()
);
#146=(
BOUNDED_SURFACE()
B_SPLINE_SURFACE(3,3,((#31488,#31489,#31490,#31491,#31492,#31493,#31494,
#31495,#31496),(#31497,#31498,#31499,#31500,#31501,#31502,#31503,#31504,
#31505),(#31506,#31507,#31508,#31509,#31510,#31511,#31512,#31513,#31514),
(#31515,#31516,#31517,#31518,#31519,#31520,#31521,#31522,#31523)),
 .UNSPECIFIED.,.F.,.F.,.F.)
B_SPLINE_SURFACE_WITH_KNOTS((4,4),(4,1,1,1,1,1,4),(0.,1.),(-0.01575975614392,
0.,0.2456294260624,0.4801888085378,0.72700648837,1.,1.015733967826),
 .UNSPECIFIED.)
GEOMETRIC_REPRESENTATION_ITEM()
RATIONAL_B_SPLINE_SURFACE(((1.201670188537,1.201670188537,1.201670188537,
1.201670188537,1.201670188537,1.201670188537,1.201670188537,1.201670188537,
1.201670188537),(0.9327766038211,0.9327766038211,0.9327766038211,0.9327766038211,
0.9327766038211,0.9327766038211,0.9327766038211,0.9327766038211,0.9327766038211),
(0.9327766038211,0.9327766038211,0.9327766038211,0.9327766038211,0.9327766038211,
0.9327766038211,0.9327766038211,0.9327766038211,0.9327766038211),(1.201670188537,
1.201670188537,1.201670188537,1.201670188537,1.201670188537,1.201670188537,
1.201670188537,1.201670188537,1.201670188537)))
REPRESENTATION_ITEM('')
SURFACE()
);
#147=(
BOUNDED_SURFACE()
B_SPLINE_SURFACE(3,3,((#31570,#31571,#31572,#31573,#31574,#31575,#31576,
#31577,#31578,#31579),(#31580,#31581,#31582,#31583,#31584,#31585,#31586,
#31587,#31588,#31589),(#31590,#31591,#31592,#31593,#31594,#31595,#31596,
#31597,#31598,#31599),(#31600,#31601,#31602,#31603,#31604,#31605,#31606,
#31607,#31608,#31609)),.UNSPECIFIED.,.F.,.F.,.F.)
B_SPLINE_SURFACE_WITH_KNOTS((4,4),(4,1,1,1,1,1,1,4),(0.,1.),(-0.02987479217279,
0.,0.1922564273876,0.376033241946,0.5650637118402,0.769737337347,1.,1.030040321285),
 .UNSPECIFIED.)
GEOMETRIC_REPRESENTATION_ITEM()
RATIONAL_B_SPLINE_SURFACE(((1.02150055857,1.02150055857,1.02150055857,1.02150055857,
1.02150055857,1.02150055857,1.02150055857,1.02150055857,1.02150055857,1.02150055857),
(0.9928331471434,0.9928331471434,0.9928331471434,0.9928331471434,0.9928331471434,
0.9928331471434,0.9928331471434,0.9928331471434,0.9928331471434,0.9928331471434),
(0.9928331471434,0.9928331471434,0.9928331471434,0.9928331471434,0.9928331471434,
0.9928331471434,0.9928331471434,0.9928331471434,0.9928331471434,0.9928331471434),
(1.02150055857,1.02150055857,1.02150055857,1.02150055857,1.02150055857,
1.02150055857,1.02150055857,1.02150055857,1.02150055857,1.02150055857)))
REPRESENTATION_ITEM('')
SURFACE()
);
#148=(
BOUNDED_SURFACE()
B_SPLINE_SURFACE(3,3,((#31612,#31613,#31614,#31615,#31616,#31617,#31618,
#31619,#31620),(#31621,#31622,#31623,#31624,#31625,#31626,#31627,#31628,
#31629),(#31630,#31631,#31632,#31633,#31634,#31635,#31636,#31637,#31638),
(#31639,#31640,#31641,#31642,#31643,#31644,#31645,#31646,#31647)),
 .UNSPECIFIED.,.F.,.F.,.F.)
B_SPLINE_SURFACE_WITH_KNOTS((4,4),(4,1,1,1,1,1,4),(0.,1.),(-0.05038062996365,
0.,0.2351349496917,0.4696037900664,0.7241664476852,1.,1.040579001464),
 .UNSPECIFIED.)
GEOMETRIC_REPRESENTATION_ITEM()
RATIONAL_B_SPLINE_SURFACE(((1.008087784169,1.008087784169,1.008087784169,
1.008087784169,1.008087784169,1.008087784169,1.008087784169,1.008087784169,
1.008087784169),(0.9973040719437,0.9973040719437,0.9973040719437,0.9973040719437,
0.9973040719437,0.9973040719437,0.9973040719437,0.9973040719437,0.9973040719437),
(0.9973040719437,0.9973040719437,0.9973040719437,0.9973040719437,0.9973040719437,
0.9973040719437,0.9973040719437,0.9973040719437,0.9973040719437),(1.008087784169,
1.008087784169,1.008087784169,1.008087784169,1.008087784169,1.008087784169,
1.008087784169,1.008087784169,1.008087784169)))
REPRESENTATION_ITEM('')
SURFACE()
);
#149=(
BOUNDED_SURFACE()
B_SPLINE_SURFACE(3,3,((#31685,#31686,#31687,#31688,#31689,#31690,#31691),
(#31692,#31693,#31694,#31695,#31696,#31697,#31698),(#31699,#31700,#31701,
#31702,#31703,#31704,#31705),(#31706,#31707,#31708,#31709,#31710,#31711,
#31712)),.UNSPECIFIED.,.F.,.F.,.F.)
B_SPLINE_SURFACE_WITH_KNOTS((4,4),(4,1,1,1,4),(0.,1.),(-0.02191865670978,
0.,0.3711108307934,0.7030029884295,0.8666418147817),.UNSPECIFIED.)
GEOMETRIC_REPRESENTATION_ITEM()
RATIONAL_B_SPLINE_SURFACE(((1.201671391236,1.201671391236,1.201671391236,
1.201671391236,1.201671391236,1.201671391236,1.201671391236),(0.9327762029212,
0.9327762029212,0.9327762029212,0.9327762029212,0.9327762029212,0.9327762029212,
0.9327762029212),(0.9327762029212,0.9327762029212,0.9327762029212,0.9327762029212,
0.9327762029212,0.9327762029212,0.9327762029212),(1.201671391236,1.201671391236,
1.201671391236,1.201671391236,1.201671391236,1.201671391236,1.201671391236)))
REPRESENTATION_ITEM('')
SURFACE()
);
#150=(
BOUNDED_SURFACE()
B_SPLINE_SURFACE(3,3,((#31714,#31715,#31716,#31717,#31718,#31719,#31720,
#31721),(#31722,#31723,#31724,#31725,#31726,#31727,#31728,#31729),(#31730,
#31731,#31732,#31733,#31734,#31735,#31736,#31737),(#31738,#31739,#31740,
#31741,#31742,#31743,#31744,#31745)),.UNSPECIFIED.,.F.,.F.,.F.)
B_SPLINE_SURFACE_WITH_KNOTS((4,4),(4,1,1,1,1,4),(0.,1.),(-0.01121526784147,
0.,0.3190655160223,0.6396471045238,1.,1.011194064343),.UNSPECIFIED.)
GEOMETRIC_REPRESENTATION_ITEM()
RATIONAL_B_SPLINE_SURFACE(((1.095350229527,1.095350229527,1.095350229527,
1.095350229527,1.095350229527,1.095350229527,1.095350229527,1.095350229527),
(0.9682165901577,0.9682165901577,0.9682165901577,0.9682165901577,0.9682165901577,
0.9682165901577,0.9682165901577,0.9682165901577),(0.9682165901577,0.9682165901577,
0.9682165901577,0.9682165901577,0.9682165901577,0.9682165901577,0.9682165901577,
0.9682165901577),(1.095350229527,1.095350229527,1.095350229527,1.095350229527,
1.095350229527,1.095350229527,1.095350229527,1.095350229527)))
REPRESENTATION_ITEM('')
SURFACE()
);
#151=(
BOUNDED_SURFACE()
B_SPLINE_SURFACE(3,3,((#31747,#31748,#31749,#31750,#31751,#31752,#31753,
#31754),(#31755,#31756,#31757,#31758,#31759,#31760,#31761,#31762),(#31763,
#31764,#31765,#31766,#31767,#31768,#31769,#31770),(#31771,#31772,#31773,
#31774,#31775,#31776,#31777,#31778)),.UNSPECIFIED.,.F.,.F.,.F.)
B_SPLINE_SURFACE_WITH_KNOTS((4,4),(4,1,1,1,1,4),(0.,1.),(-0.01123151966199,
0.,0.3226423274774,0.6411748598112,1.,1.011214131254),.UNSPECIFIED.)
GEOMETRIC_REPRESENTATION_ITEM()
RATIONAL_B_SPLINE_SURFACE(((1.095350237894,1.095350237894,1.095350237894,
1.095350237894,1.095350237894,1.095350237894,1.095350237894,1.095350237894),
(0.9682165873688,0.9682165873688,0.9682165873688,0.9682165873688,0.9682165873688,
0.9682165873688,0.9682165873688,0.9682165873688),(0.9682165873688,0.9682165873688,
0.9682165873688,0.9682165873688,0.9682165873688,0.9682165873688,0.9682165873688,
0.9682165873688),(1.095350237894,1.095350237894,1.095350237894,1.095350237894,
1.095350237894,1.095350237894,1.095350237894,1.095350237894)))
REPRESENTATION_ITEM('')
SURFACE()
);
#152=(
BOUNDED_SURFACE()
B_SPLINE_SURFACE(3,3,((#31780,#31781,#31782,#31783,#31784,#31785,#31786),
(#31787,#31788,#31789,#31790,#31791,#31792,#31793),(#31794,#31795,#31796,
#31797,#31798,#31799,#31800),(#31801,#31802,#31803,#31804,#31805,#31806,
#31807)),.UNSPECIFIED.,.F.,.F.,.F.)
B_SPLINE_SURFACE_WITH_KNOTS((4,4),(4,1,1,1,4),(0.,1.),(0.1126138017486,
0.319861120519,0.6533271596459,1.,1.026625433703),.UNSPECIFIED.)
GEOMETRIC_REPRESENTATION_ITEM()
RATIONAL_B_SPLINE_SURFACE(((1.133923637937,1.133923637937,1.133923637937,
1.133923637937,1.133923637937,1.133923637937,1.133923637937),(0.9553587873545,
0.9553587873545,0.9553587873545,0.9553587873545,0.9553587873545,0.9553587873545,
0.9553587873545),(0.9553587873545,0.9553587873545,0.9553587873545,0.9553587873545,
0.9553587873545,0.9553587873545,0.9553587873545),(1.133923637937,1.133923637937,
1.133923637937,1.133923637937,1.133923637937,1.133923637937,1.133923637937)))
REPRESENTATION_ITEM('')
SURFACE()
);
#153=(
BOUNDED_SURFACE()
B_SPLINE_SURFACE(3,3,((#31844,#31845,#31846,#31847,#31848,#31849,#31850,
#31851,#31852,#31853,#31854),(#31855,#31856,#31857,#31858,#31859,#31860,
#31861,#31862,#31863,#31864,#31865),(#31866,#31867,#31868,#31869,#31870,
#31871,#31872,#31873,#31874,#31875,#31876),(#31877,#31878,#31879,#31880,
#31881,#31882,#31883,#31884,#31885,#31886,#31887)),.UNSPECIFIED.,.F.,.F.,
 .F.)
B_SPLINE_SURFACE_WITH_KNOTS((4,4),(4,1,1,1,1,1,1,1,4),(0.,1.),(-0.04051174551792,
0.,0.1601684695697,0.3176853418238,0.4756542837724,0.6362846105788,0.8070461231236,
1.,1.048408689707),.UNSPECIFIED.)
GEOMETRIC_REPRESENTATION_ITEM()
RATIONAL_B_SPLINE_SURFACE(((1.008087174024,1.008087174024,1.008087174024,
1.008087174024,1.008087174024,1.008087174024,1.008087174024,1.008087174024,
1.008087174024,1.008087174024,1.008087174024),(0.9973042753252,0.9973042753252,
0.9973042753252,0.9973042753252,0.9973042753252,0.9973042753252,0.9973042753252,
0.9973042753252,0.9973042753252,0.9973042753252,0.9973042753252),(0.9973042753252,
0.9973042753252,0.9973042753252,0.9973042753252,0.9973042753252,0.9973042753252,
0.9973042753252,0.9973042753252,0.9973042753252,0.9973042753252,0.9973042753252),
(1.008087174024,1.008087174024,1.008087174024,1.008087174024,1.008087174024,
1.008087174024,1.008087174024,1.008087174024,1.008087174024,1.008087174024,
1.008087174024)))
REPRESENTATION_ITEM('')
SURFACE()
);
#154=(
BOUNDED_SURFACE()
B_SPLINE_SURFACE(3,3,((#31889,#31890,#31891,#31892,#31893,#31894,#31895,
#31896,#31897),(#31898,#31899,#31900,#31901,#31902,#31903,#31904,#31905,
#31906),(#31907,#31908,#31909,#31910,#31911,#31912,#31913,#31914,#31915),
(#31916,#31917,#31918,#31919,#31920,#31921,#31922,#31923,#31924)),
 .UNSPECIFIED.,.F.,.F.,.F.)
B_SPLINE_SURFACE_WITH_KNOTS((4,4),(4,1,1,1,1,1,4),(0.,1.),(-0.02991897955271,
0.,0.2239749897618,0.4574668129281,0.7131740843088,1.,1.029884092175),
 .UNSPECIFIED.)
GEOMETRIC_REPRESENTATION_ITEM()
RATIONAL_B_SPLINE_SURFACE(((1.021500558577,1.021500558577,1.021500558577,
1.021500558577,1.021500558577,1.021500558577,1.021500558577,1.021500558577,
1.021500558577),(0.992833147141,0.992833147141,0.992833147141,0.992833147141,
0.992833147141,0.992833147141,0.992833147141,0.992833147141,0.992833147141),
(0.992833147141,0.992833147141,0.992833147141,0.992833147141,0.992833147141,
0.992833147141,0.992833147141,0.992833147141,0.992833147141),(1.021500558577,
1.021500558577,1.021500558577,1.021500558577,1.021500558577,1.021500558577,
1.021500558577,1.021500558577,1.021500558577)))
REPRESENTATION_ITEM('')
SURFACE()
);
#155=(
BOUNDED_SURFACE()
B_SPLINE_SURFACE(3,3,((#31992,#31993,#31994,#31995,#31996,#31997,#31998,
#31999,#32000,#32001,#32002),(#32003,#32004,#32005,#32006,#32007,#32008,
#32009,#32010,#32011,#32012,#32013),(#32014,#32015,#32016,#32017,#32018,
#32019,#32020,#32021,#32022,#32023,#32024),(#32025,#32026,#32027,#32028,
#32029,#32030,#32031,#32032,#32033,#32034,#32035)),.UNSPECIFIED.,.F.,.F.,
 .F.)
B_SPLINE_SURFACE_WITH_KNOTS((4,4),(4,1,1,1,1,1,1,1,4),(0.,1.),(-0.02991442636641,
0.,0.1652192384749,0.3271780455741,0.486578186817,0.6458635561448,0.8144083932013,
1.,1.029876740826),.UNSPECIFIED.)
GEOMETRIC_REPRESENTATION_ITEM()
RATIONAL_B_SPLINE_SURFACE(((1.021500558569,1.021500558569,1.021500558569,
1.021500558569,1.021500558569,1.021500558569,1.021500558569,1.021500558569,
1.021500558569,1.021500558569,1.021500558569),(0.9928331471435,0.9928331471435,
0.9928331471435,0.9928331471435,0.9928331471435,0.9928331471435,0.9928331471435,
0.9928331471435,0.9928331471435,0.9928331471435,0.9928331471435),(0.9928331471435,
0.9928331471435,0.9928331471435,0.9928331471435,0.9928331471435,0.9928331471435,
0.9928331471435,0.9928331471435,0.9928331471435,0.9928331471435,0.9928331471435),
(1.021500558569,1.021500558569,1.021500558569,1.021500558569,1.021500558569,
1.021500558569,1.021500558569,1.021500558569,1.021500558569,1.021500558569,
1.021500558569)))
REPRESENTATION_ITEM('')
SURFACE()
);
#156=(
BOUNDED_SURFACE()
B_SPLINE_SURFACE(3,3,((#32040,#32041,#32042,#32043,#32044,#32045,#32046,
#32047,#32048,#32049,#32050,#32051),(#32052,#32053,#32054,#32055,#32056,
#32057,#32058,#32059,#32060,#32061,#32062,#32063),(#32064,#32065,#32066,
#32067,#32068,#32069,#32070,#32071,#32072,#32073,#32074,#32075),(#32076,
#32077,#32078,#32079,#32080,#32081,#32082,#32083,#32084,#32085,#32086,#32087)),
 .UNSPECIFIED.,.F.,.F.,.F.)
B_SPLINE_SURFACE_WITH_KNOTS((4,4),(4,1,1,1,1,1,1,1,1,4),(0.,1.),(0.0119111100004,
0.111104700859,0.2222213328836,0.3333553389617,0.4444873410571,0.5556025705647,
0.6667268893849,0.7778458691404,0.888938349439,0.9826188152285),
 .UNSPECIFIED.)
GEOMETRIC_REPRESENTATION_ITEM()
RATIONAL_B_SPLINE_SURFACE(((1.211236726733,1.211236726733,1.211236726733,
1.211236726733,1.211236726733,1.211236726733,1.211236726733,1.211236726733,
1.211236726733,1.211236726733,1.211236726733,1.211236726733),(0.9295877577556,
0.9295877577556,0.9295877577556,0.9295877577556,0.9295877577556,0.9295877577556,
0.9295877577556,0.9295877577556,0.9295877577556,0.9295877577556,0.9295877577556,
0.9295877577556),(0.9295877577556,0.9295877577556,0.9295877577556,0.9295877577556,
0.9295877577556,0.9295877577556,0.9295877577556,0.9295877577556,0.9295877577556,
0.9295877577556,0.9295877577556,0.9295877577556),(1.211236726733,1.211236726733,
1.211236726733,1.211236726733,1.211236726733,1.211236726733,1.211236726733,
1.211236726733,1.211236726733,1.211236726733,1.211236726733,1.211236726733)))
REPRESENTATION_ITEM('')
SURFACE()
);
#157=(
BOUNDED_SURFACE()
B_SPLINE_SURFACE(3,3,((#32123,#32124,#32125,#32126,#32127,#32128,#32129,
#32130,#32131),(#32132,#32133,#32134,#32135,#32136,#32137,#32138,#32139,
#32140),(#32141,#32142,#32143,#32144,#32145,#32146,#32147,#32148,#32149),
(#32150,#32151,#32152,#32153,#32154,#32155,#32156,#32157,#32158)),
 .UNSPECIFIED.,.F.,.F.,.F.)
B_SPLINE_SURFACE_WITH_KNOTS((4,4),(4,1,1,1,1,1,4),(0.,1.),(-0.01575975614391,
0.,0.2456294260624,0.4801888085378,0.7270064883701,1.,1.015733967826),
 .UNSPECIFIED.)
GEOMETRIC_REPRESENTATION_ITEM()
RATIONAL_B_SPLINE_SURFACE(((1.201670188537,1.201670188537,1.201670188537,
1.201670188537,1.201670188537,1.201670188537,1.201670188537,1.201670188537,
1.201670188537),(0.9327766038211,0.9327766038211,0.9327766038211,0.9327766038211,
0.9327766038211,0.9327766038211,0.9327766038211,0.9327766038211,0.9327766038211),
(0.9327766038211,0.9327766038211,0.9327766038211,0.9327766038211,0.9327766038211,
0.9327766038211,0.9327766038211,0.9327766038211,0.9327766038211),(1.201670188537,
1.201670188537,1.201670188537,1.201670188537,1.201670188537,1.201670188537,
1.201670188537,1.201670188537,1.201670188537)))
REPRESENTATION_ITEM('')
SURFACE()
);
#158=(
BOUNDED_SURFACE()
B_SPLINE_SURFACE(3,3,((#32368,#32369,#32370,#32371,#32372,#32373,#32374,
#32375),(#32376,#32377,#32378,#32379,#32380,#32381,#32382,#32383),(#32384,
#32385,#32386,#32387,#32388,#32389,#32390,#32391),(#32392,#32393,#32394,
#32395,#32396,#32397,#32398,#32399)),.UNSPECIFIED.,.F.,.F.,.F.)
B_SPLINE_SURFACE_WITH_KNOTS((4,4),(4,1,1,1,1,4),(0.,1.),(-0.02000000006299,
0.,0.3331237554216,0.6664570887615,1.,1.020000003967),.UNSPECIFIED.)
GEOMETRIC_REPRESENTATION_ITEM()
RATIONAL_B_SPLINE_SURFACE(((1.158475807259,1.158475807259,1.158475807259,
1.158475807259,1.158475807259,1.158475807259,1.158475807259,1.158475807259),
(0.9471747309136,0.9471747309136,0.9471747309136,0.9471747309136,0.9471747309136,
0.9471747309136,0.9471747309136,0.9471747309136),(0.9471747309136,0.9471747309136,
0.9471747309136,0.9471747309136,0.9471747309136,0.9471747309136,0.9471747309136,
0.9471747309136),(1.158475807259,1.158475807259,1.158475807259,1.158475807259,
1.158475807259,1.158475807259,1.158475807259,1.158475807259)))
REPRESENTATION_ITEM('')
SURFACE()
);
#159=(
BOUNDED_SURFACE()
B_SPLINE_SURFACE(3,3,((#32407,#32408,#32409,#32410,#32411,#32412,#32413,
#32414),(#32415,#32416,#32417,#32418,#32419,#32420,#32421,#32422),(#32423,
#32424,#32425,#32426,#32427,#32428,#32429,#32430),(#32431,#32432,#32433,
#32434,#32435,#32436,#32437,#32438)),.UNSPECIFIED.,.F.,.F.,.F.)
B_SPLINE_SURFACE_WITH_KNOTS((4,4),(4,1,1,1,1,4),(0.,1.),(-0.02,0.,0.3335430444131,
0.666876377753,1.,1.019999999985),.UNSPECIFIED.)
GEOMETRIC_REPRESENTATION_ITEM()
RATIONAL_B_SPLINE_SURFACE(((1.158475807259,1.158475807259,1.158475807259,
1.158475807259,1.158475807259,1.158475807259,1.158475807259,1.158475807259),
(0.9471747309136,0.9471747309136,0.9471747309136,0.9471747309136,0.9471747309136,
0.9471747309136,0.9471747309136,0.9471747309136),(0.9471747309136,0.9471747309136,
0.9471747309136,0.9471747309136,0.9471747309136,0.9471747309136,0.9471747309136,
0.9471747309136),(1.158475807259,1.158475807259,1.158475807259,1.158475807259,
1.158475807259,1.158475807259,1.158475807259,1.158475807259)))
REPRESENTATION_ITEM('')
SURFACE()
);
#160=(
BOUNDED_SURFACE()
B_SPLINE_SURFACE(3,3,((#32665,#32666,#32667,#32668,#32669,#32670,#32671,
#32672,#32673,#32674),(#32675,#32676,#32677,#32678,#32679,#32680,#32681,
#32682,#32683,#32684),(#32685,#32686,#32687,#32688,#32689,#32690,#32691,
#32692,#32693,#32694),(#32695,#32696,#32697,#32698,#32699,#32700,#32701,
#32702,#32703,#32704)),.UNSPECIFIED.,.F.,.F.,.F.)
B_SPLINE_SURFACE_WITH_KNOTS((4,4),(4,1,1,1,1,1,1,4),(0.,1.),(-0.02782793672778,
0.,0.2061198945833,0.405852717027,0.5969792694224,0.7914070803093,1.,1.028079856947),
 .UNSPECIFIED.)
GEOMETRIC_REPRESENTATION_ITEM()
RATIONAL_B_SPLINE_SURFACE(((1.187634479517,1.187634479517,1.187634479517,
1.187634479517,1.187634479517,1.187634479517,1.187634479517,1.187634479517,
1.187634479517,1.187634479517),(0.9374551734942,0.9374551734942,0.9374551734942,
0.9374551734942,0.9374551734942,0.9374551734942,0.9374551734942,0.9374551734942,
0.9374551734942,0.9374551734942),(0.9374551734942,0.9374551734942,0.9374551734942,
0.9374551734942,0.9374551734942,0.9374551734942,0.9374551734942,0.9374551734942,
0.9374551734942,0.9374551734942),(1.187634479517,1.187634479517,1.187634479517,
1.187634479517,1.187634479517,1.187634479517,1.187634479517,1.187634479517,
1.187634479517,1.187634479517)))
REPRESENTATION_ITEM('')
SURFACE()
);
#161=(
BOUNDED_SURFACE()
B_SPLINE_SURFACE(3,3,((#32793,#32794,#32795,#32796,#32797,#32798,#32799,
#32800,#32801,#32802),(#32803,#32804,#32805,#32806,#32807,#32808,#32809,
#32810,#32811,#32812),(#32813,#32814,#32815,#32816,#32817,#32818,#32819,
#32820,#32821,#32822),(#32823,#32824,#32825,#32826,#32827,#32828,#32829,
#32830,#32831,#32832)),.UNSPECIFIED.,.F.,.F.,.F.)
B_SPLINE_SURFACE_WITH_KNOTS((4,4),(4,1,1,1,1,1,1,4),(0.,1.),(-0.02810083996936,
0.,0.2044929737017,0.4039878177866,0.5954658095825,0.7901158902839,1.,1.027817073056),
 .UNSPECIFIED.)
GEOMETRIC_REPRESENTATION_ITEM()
RATIONAL_B_SPLINE_SURFACE(((1.187634481559,1.187634481559,1.187634481559,
1.187634481559,1.187634481559,1.187634481559,1.187634481559,1.187634481559,
1.187634481559,1.187634481559),(0.9374551728136,0.9374551728136,0.9374551728136,
0.9374551728136,0.9374551728136,0.9374551728136,0.9374551728136,0.9374551728136,
0.9374551728136,0.9374551728136),(0.9374551728136,0.9374551728136,0.9374551728136,
0.9374551728136,0.9374551728136,0.9374551728136,0.9374551728136,0.9374551728136,
0.9374551728136,0.9374551728136),(1.187634481559,1.187634481559,1.187634481559,
1.187634481559,1.187634481559,1.187634481559,1.187634481559,1.187634481559,
1.187634481559,1.187634481559)))
REPRESENTATION_ITEM('')
SURFACE()
);
#162=(
BOUNDED_SURFACE()
B_SPLINE_SURFACE(3,3,((#32835,#32836,#32837,#32838,#32839,#32840,#32841,
#32842),(#32843,#32844,#32845,#32846,#32847,#32848,#32849,#32850),(#32851,
#32852,#32853,#32854,#32855,#32856,#32857,#32858),(#32859,#32860,#32861,
#32862,#32863,#32864,#32865,#32866)),.UNSPECIFIED.,.F.,.F.,.F.)
B_SPLINE_SURFACE_WITH_KNOTS((4,4),(4,1,1,1,1,4),(0.,1.),(-0.001077616544647,
0.,0.0278179355033,0.0559228241955,0.08712239292215,0.1088331409388),
 .UNSPECIFIED.)
GEOMETRIC_REPRESENTATION_ITEM()
RATIONAL_B_SPLINE_SURFACE(((1.199526979016,1.199526979016,1.199526979016,
1.199526979016,1.199526979016,1.199526979016,1.199526979016,1.199526979016),
(0.9334910069946,0.9334910069946,0.9334910069946,0.9334910069946,0.9334910069946,
0.9334910069946,0.9334910069946,0.9334910069946),(0.9334910069946,0.9334910069946,
0.9334910069946,0.9334910069946,0.9334910069946,0.9334910069946,0.9334910069946,
0.9334910069946),(1.199526979016,1.199526979016,1.199526979016,1.199526979016,
1.199526979016,1.199526979016,1.199526979016,1.199526979016)))
REPRESENTATION_ITEM('')
SURFACE()
);
#163=(
BOUNDED_SURFACE()
B_SPLINE_SURFACE(3,3,((#32867,#32868,#32869,#32870,#32871,#32872,#32873,
#32874),(#32875,#32876,#32877,#32878,#32879,#32880,#32881,#32882),(#32883,
#32884,#32885,#32886,#32887,#32888,#32889,#32890),(#32891,#32892,#32893,
#32894,#32895,#32896,#32897,#32898)),.UNSPECIFIED.,.F.,.F.,.F.)
B_SPLINE_SURFACE_WITH_KNOTS((4,4),(4,1,1,1,1,4),(0.,1.),(-0.02,0.,0.3335430447055,
0.6668763780453,1.,1.019999999985),.UNSPECIFIED.)
GEOMETRIC_REPRESENTATION_ITEM()
RATIONAL_B_SPLINE_SURFACE(((1.158475807259,1.158475807259,1.158475807259,
1.158475807259,1.158475807259,1.158475807259,1.158475807259,1.158475807259),
(0.9471747309136,0.9471747309136,0.9471747309136,0.9471747309136,0.9471747309136,
0.9471747309136,0.9471747309136,0.9471747309136),(0.9471747309136,0.9471747309136,
0.9471747309136,0.9471747309136,0.9471747309136,0.9471747309136,0.9471747309136,
0.9471747309136),(1.158475807259,1.158475807259,1.158475807259,1.158475807259,
1.158475807259,1.158475807259,1.158475807259,1.158475807259)))
REPRESENTATION_ITEM('')
SURFACE()
);
#164=(
BOUNDED_SURFACE()
B_SPLINE_SURFACE(3,3,((#32906,#32907,#32908,#32909,#32910,#32911,#32912,
#32913),(#32914,#32915,#32916,#32917,#32918,#32919,#32920,#32921),(#32922,
#32923,#32924,#32925,#32926,#32927,#32928,#32929),(#32930,#32931,#32932,
#32933,#32934,#32935,#32936,#32937)),.UNSPECIFIED.,.F.,.F.,.F.)
B_SPLINE_SURFACE_WITH_KNOTS((4,4),(4,1,1,1,1,4),(0.,1.),(-0.02000000007603,
0.,0.3331237556924,0.6664570890323,1.,1.020000004632),.UNSPECIFIED.)
GEOMETRIC_REPRESENTATION_ITEM()
RATIONAL_B_SPLINE_SURFACE(((1.158475807259,1.158475807259,1.158475807259,
1.158475807259,1.158475807259,1.158475807259,1.158475807259,1.158475807259),
(0.9471747309136,0.9471747309136,0.9471747309136,0.9471747309136,0.9471747309136,
0.9471747309136,0.9471747309136,0.9471747309136),(0.9471747309136,0.9471747309136,
0.9471747309136,0.9471747309136,0.9471747309136,0.9471747309136,0.9471747309136,
0.9471747309136),(1.158475807259,1.158475807259,1.158475807259,1.158475807259,
1.158475807259,1.158475807259,1.158475807259,1.158475807259)))
REPRESENTATION_ITEM('')
SURFACE()
);
#165=(
BOUNDED_SURFACE()
B_SPLINE_SURFACE(3,3,((#32939,#32940,#32941,#32942,#32943,#32944,#32945,
#32946,#32947),(#32948,#32949,#32950,#32951,#32952,#32953,#32954,#32955,
#32956),(#32957,#32958,#32959,#32960,#32961,#32962,#32963,#32964,#32965),
(#32966,#32967,#32968,#32969,#32970,#32971,#32972,#32973,#32974)),
 .UNSPECIFIED.,.F.,.F.,.F.)
B_SPLINE_SURFACE_WITH_KNOTS((4,4),(4,1,1,1,1,1,4),(0.,1.),(-0.03990139320459,
0.,0.2383747185699,0.4794833111693,0.7307955330181,1.,1.039731692604),
 .UNSPECIFIED.)
GEOMETRIC_REPRESENTATION_ITEM()
RATIONAL_B_SPLINE_SURFACE(((1.163827495202,1.163827495202,1.163827495202,
1.163827495202,1.163827495202,1.163827495202,1.163827495202,1.163827495202,
1.163827495202),(0.9453908349325,0.9453908349325,0.9453908349325,0.9453908349325,
0.9453908349325,0.9453908349325,0.9453908349325,0.9453908349325,0.9453908349325),
(0.9453908349325,0.9453908349325,0.9453908349325,0.9453908349325,0.9453908349325,
0.9453908349325,0.9453908349325,0.9453908349325,0.9453908349325),(1.163827495202,
1.163827495202,1.163827495202,1.163827495202,1.163827495202,1.163827495202,
1.163827495202,1.163827495202,1.163827495202)))
REPRESENTATION_ITEM('')
SURFACE()
);
#166=(
BOUNDED_SURFACE()
B_SPLINE_SURFACE(3,3,((#33033,#33034,#33035,#33036,#33037,#33038,#33039,
#33040,#33041),(#33042,#33043,#33044,#33045,#33046,#33047,#33048,#33049,
#33050),(#33051,#33052,#33053,#33054,#33055,#33056,#33057,#33058,#33059),
(#33060,#33061,#33062,#33063,#33064,#33065,#33066,#33067,#33068)),
 .UNSPECIFIED.,.F.,.F.,.F.)
B_SPLINE_SURFACE_WITH_KNOTS((4,4),(4,1,1,1,1,1,4),(0.,1.),(-0.03973821722907,
0.,0.2388826440098,0.4802432095543,0.7314080978693,1.,1.039877733719),
 .UNSPECIFIED.)
GEOMETRIC_REPRESENTATION_ITEM()
RATIONAL_B_SPLINE_SURFACE(((1.163827493612,1.163827493612,1.163827493612,
1.163827493612,1.163827493612,1.163827493612,1.163827493612,1.163827493612,
1.163827493612),(0.9453908354627,0.9453908354627,0.9453908354627,0.9453908354627,
0.9453908354627,0.9453908354627,0.9453908354627,0.9453908354627,0.9453908354627),
(0.9453908354627,0.9453908354627,0.9453908354627,0.9453908354627,0.9453908354627,
0.9453908354627,0.9453908354627,0.9453908354627,0.9453908354627),(1.163827493612,
1.163827493612,1.163827493612,1.163827493612,1.163827493612,1.163827493612,
1.163827493612,1.163827493612,1.163827493612)))
REPRESENTATION_ITEM('')
SURFACE()
);
#167=(
BOUNDED_SURFACE()
B_SPLINE_SURFACE(3,3,((#33070,#33071,#33072,#33073,#33074,#33075,#33076,
#33077,#33078,#33079,#33080,#33081,#33082,#33083,#33084,#33085,#33086,#33087,
#33088,#33089,#33090,#33091,#33092,#33093,#33094,#33095,#33096,#33097,#33098,
#33099,#33100,#33101),(#33102,#33103,#33104,#33105,#33106,#33107,#33108,
#33109,#33110,#33111,#33112,#33113,#33114,#33115,#33116,#33117,#33118,#33119,
#33120,#33121,#33122,#33123,#33124,#33125,#33126,#33127,#33128,#33129,#33130,
#33131,#33132,#33133),(#33134,#33135,#33136,#33137,#33138,#33139,#33140,
#33141,#33142,#33143,#33144,#33145,#33146,#33147,#33148,#33149,#33150,#33151,
#33152,#33153,#33154,#33155,#33156,#33157,#33158,#33159,#33160,#33161,#33162,
#33163,#33164,#33165),(#33166,#33167,#33168,#33169,#33170,#33171,#33172,
#33173,#33174,#33175,#33176,#33177,#33178,#33179,#33180,#33181,#33182,#33183,
#33184,#33185,#33186,#33187,#33188,#33189,#33190,#33191,#33192,#33193,#33194,
#33195,#33196,#33197)),.UNSPECIFIED.,.F.,.F.,.F.)
B_SPLINE_SURFACE_WITH_KNOTS((4,4),(4,1,1,1,1,1,1,1,1,1,1,1,1,1,1,1,1,1,
1,1,1,1,1,1,1,1,1,1,1,4),(0.,1.),(-0.009989617270159,0.,0.0587369296208,
0.111068550249,0.1581000808001,0.2003396839717,0.2384448290796,0.2747221985793,
0.3117544904028,0.3494937277553,0.3869465899255,0.4242215507061,0.4615931261968,
0.499066395259,0.5364199609172,0.5733902772176,0.6100694635878,0.6464467903499,
0.6809974474155,0.7120024196009,0.7411742705344,0.7707771184994,0.8006196344549,
0.8302940356761,0.8602243035839,0.8909644083677,0.9237463930732,0.9597502743101,
1.,1.009989117017),.UNSPECIFIED.)
GEOMETRIC_REPRESENTATION_ITEM()
RATIONAL_B_SPLINE_SURFACE(((1.192397230944,1.192397230944,1.192397230944,
1.192397230944,1.192397230944,1.192397230944,1.192397230944,1.192397230944,
1.192397230944,1.192397230944,1.192397230944,1.192397230944,1.192397230944,
1.192397230944,1.192397230944,1.192397230944,1.192397230944,1.192397230944,
1.192397230944,1.192397230944,1.192397230944,1.192397230944,1.192397230944,
1.192397230944,1.192397230944,1.192397230944,1.192397230944,1.192397230944,
1.192397230944,1.192397230944,1.192397230944,1.192397230944),(0.9358675896855,
0.9358675896855,0.9358675896855,0.9358675896855,0.9358675896855,0.9358675896855,
0.9358675896855,0.9358675896855,0.9358675896855,0.9358675896855,0.9358675896855,
0.9358675896855,0.9358675896855,0.9358675896855,0.9358675896855,0.9358675896855,
0.9358675896855,0.9358675896855,0.9358675896855,0.9358675896855,0.9358675896855,
0.9358675896855,0.9358675896855,0.9358675896855,0.9358675896855,0.9358675896855,
0.9358675896855,0.9358675896855,0.9358675896855,0.9358675896855,0.9358675896855,
0.9358675896855),(0.9358675896855,0.9358675896855,0.9358675896855,0.9358675896855,
0.9358675896855,0.9358675896855,0.9358675896855,0.9358675896855,0.9358675896855,
0.9358675896855,0.9358675896855,0.9358675896855,0.9358675896855,0.9358675896855,
0.9358675896855,0.9358675896855,0.9358675896855,0.9358675896855,0.9358675896855,
0.9358675896855,0.9358675896855,0.9358675896855,0.9358675896855,0.9358675896855,
0.9358675896855,0.9358675896855,0.9358675896855,0.9358675896855,0.9358675896855,
0.9358675896855,0.9358675896855,0.9358675896855),(1.192397230944,1.192397230944,
1.192397230944,1.192397230944,1.192397230944,1.192397230944,1.192397230944,
1.192397230944,1.192397230944,1.192397230944,1.192397230944,1.192397230944,
1.192397230944,1.192397230944,1.192397230944,1.192397230944,1.192397230944,
1.192397230944,1.192397230944,1.192397230944,1.192397230944,1.192397230944,
1.192397230944,1.192397230944,1.192397230944,1.192397230944,1.192397230944,
1.192397230944,1.192397230944,1.192397230944,1.192397230944,1.192397230944)))
REPRESENTATION_ITEM('')
SURFACE()
);
#168=(
BOUNDED_SURFACE()
B_SPLINE_SURFACE(3,3,((#33666,#33667,#33668,#33669,#33670,#33671,#33672,
#33673,#33674,#33675,#33676,#33677,#33678,#33679,#33680,#33681,#33682,#33683,
#33684,#33685,#33686,#33687,#33688,#33689,#33690,#33691,#33692,#33693,#33694,
#33695,#33696,#33697),(#33698,#33699,#33700,#33701,#33702,#33703,#33704,
#33705,#33706,#33707,#33708,#33709,#33710,#33711,#33712,#33713,#33714,#33715,
#33716,#33717,#33718,#33719,#33720,#33721,#33722,#33723,#33724,#33725,#33726,
#33727,#33728,#33729),(#33730,#33731,#33732,#33733,#33734,#33735,#33736,
#33737,#33738,#33739,#33740,#33741,#33742,#33743,#33744,#33745,#33746,#33747,
#33748,#33749,#33750,#33751,#33752,#33753,#33754,#33755,#33756,#33757,#33758,
#33759,#33760,#33761),(#33762,#33763,#33764,#33765,#33766,#33767,#33768,
#33769,#33770,#33771,#33772,#33773,#33774,#33775,#33776,#33777,#33778,#33779,
#33780,#33781,#33782,#33783,#33784,#33785,#33786,#33787,#33788,#33789,#33790,
#33791,#33792,#33793)),.UNSPECIFIED.,.F.,.F.,.F.)
B_SPLINE_SURFACE_WITH_KNOTS((4,4),(4,1,1,1,1,1,1,1,1,1,1,1,1,1,1,1,1,1,
1,1,1,1,1,1,1,1,1,1,1,4),(0.,1.),(-0.009989616921005,0.,0.05872646932563,
0.1110508073303,0.1580780876269,0.2003155443802,0.2384155963746,0.2746745689611,
0.3116781024864,0.3493943002845,0.3868271443784,0.4240772685742,0.4614186760705,
0.4988604389596,0.5361879081759,0.5731414127621,0.6098108086259,0.6461939396313,
0.6807803323384,0.7118281019108,0.7410274548133,0.7706525155955,0.8005231162647,
0.8302238307092,0.8601755167066,0.89093194483,0.9237248042115,0.9597384770757,
1.,1.009989116574),.UNSPECIFIED.)
GEOMETRIC_REPRESENTATION_ITEM()
RATIONAL_B_SPLINE_SURFACE(((1.192397251387,1.192397251387,1.192397251387,
1.192397251387,1.192397251387,1.192397251387,1.192397251387,1.192397251387,
1.192397251387,1.192397251387,1.192397251387,1.192397251387,1.192397251387,
1.192397251387,1.192397251387,1.192397251387,1.192397251387,1.192397251387,
1.192397251387,1.192397251387,1.192397251387,1.192397251387,1.192397251387,
1.192397251387,1.192397251387,1.192397251387,1.192397251387,1.192397251387,
1.192397251387,1.192397251387,1.192397251387,1.192397251387),(0.935867582871,
0.935867582871,0.935867582871,0.935867582871,0.935867582871,0.935867582871,
0.935867582871,0.935867582871,0.935867582871,0.935867582871,0.935867582871,
0.935867582871,0.935867582871,0.935867582871,0.935867582871,0.935867582871,
0.935867582871,0.935867582871,0.935867582871,0.935867582871,0.935867582871,
0.935867582871,0.935867582871,0.935867582871,0.935867582871,0.935867582871,
0.935867582871,0.935867582871,0.935867582871,0.935867582871,0.935867582871,
0.935867582871),(0.935867582871,0.935867582871,0.935867582871,0.935867582871,
0.935867582871,0.935867582871,0.935867582871,0.935867582871,0.935867582871,
0.935867582871,0.935867582871,0.935867582871,0.935867582871,0.935867582871,
0.935867582871,0.935867582871,0.935867582871,0.935867582871,0.935867582871,
0.935867582871,0.935867582871,0.935867582871,0.935867582871,0.935867582871,
0.935867582871,0.935867582871,0.935867582871,0.935867582871,0.935867582871,
0.935867582871,0.935867582871,0.935867582871),(1.192397251387,1.192397251387,
1.192397251387,1.192397251387,1.192397251387,1.192397251387,1.192397251387,
1.192397251387,1.192397251387,1.192397251387,1.192397251387,1.192397251387,
1.192397251387,1.192397251387,1.192397251387,1.192397251387,1.192397251387,
1.192397251387,1.192397251387,1.192397251387,1.192397251387,1.192397251387,
1.192397251387,1.192397251387,1.192397251387,1.192397251387,1.192397251387,
1.192397251387,1.192397251387,1.192397251387,1.192397251387,1.192397251387)))
REPRESENTATION_ITEM('')
SURFACE()
);
#169=(
BOUNDED_SURFACE()
B_SPLINE_SURFACE(3,3,((#33795,#33796,#33797,#33798,#33799,#33800,#33801,
#33802,#33803),(#33804,#33805,#33806,#33807,#33808,#33809,#33810,#33811,
#33812),(#33813,#33814,#33815,#33816,#33817,#33818,#33819,#33820,#33821),
(#33822,#33823,#33824,#33825,#33826,#33827,#33828,#33829,#33830)),
 .UNSPECIFIED.,.F.,.F.,.F.)
B_SPLINE_SURFACE_WITH_KNOTS((4,4),(4,1,1,1,1,1,4),(0.,1.),(-0.03973820027638,
0.,0.238622357915,0.4800568473432,0.731387517944,1.,1.03987771478),
 .UNSPECIFIED.)
GEOMETRIC_REPRESENTATION_ITEM()
RATIONAL_B_SPLINE_SURFACE(((1.163827493602,1.163827493602,1.163827493602,
1.163827493602,1.163827493602,1.163827493602,1.163827493602,1.163827493602,
1.163827493602),(0.9453908354662,0.9453908354662,0.9453908354662,0.9453908354662,
0.9453908354662,0.9453908354662,0.9453908354662,0.9453908354662,0.9453908354662),
(0.9453908354662,0.9453908354662,0.9453908354662,0.9453908354662,0.9453908354662,
0.9453908354662,0.9453908354662,0.9453908354662,0.9453908354662),(1.163827493602,
1.163827493602,1.163827493602,1.163827493602,1.163827493602,1.163827493602,
1.163827493602,1.163827493602,1.163827493602)))
REPRESENTATION_ITEM('')
SURFACE()
);
#170=(
BOUNDED_SURFACE()
B_SPLINE_SURFACE(3,3,((#33888,#33889,#33890,#33891,#33892,#33893,#33894,
#33895,#33896),(#33897,#33898,#33899,#33900,#33901,#33902,#33903,#33904,
#33905),(#33906,#33907,#33908,#33909,#33910,#33911,#33912,#33913,#33914),
(#33915,#33916,#33917,#33918,#33919,#33920,#33921,#33922,#33923)),
 .UNSPECIFIED.,.F.,.F.,.F.)
B_SPLINE_SURFACE_WITH_KNOTS((4,4),(4,1,1,1,1,1,4),(0.,1.),(-0.03990137353967,
0.,0.2386413019669,0.4796774710128,0.7308215928377,1.,1.039731675547),
 .UNSPECIFIED.)
GEOMETRIC_REPRESENTATION_ITEM()
RATIONAL_B_SPLINE_SURFACE(((1.163827495208,1.163827495208,1.163827495208,
1.163827495208,1.163827495208,1.163827495208,1.163827495208,1.163827495208,
1.163827495208),(0.9453908349308,0.9453908349308,0.9453908349308,0.9453908349308,
0.9453908349308,0.9453908349308,0.9453908349308,0.9453908349308,0.9453908349308),
(0.9453908349308,0.9453908349308,0.9453908349308,0.9453908349308,0.9453908349308,
0.9453908349308,0.9453908349308,0.9453908349308,0.9453908349308),(1.163827495208,
1.163827495208,1.163827495208,1.163827495208,1.163827495208,1.163827495208,
1.163827495208,1.163827495208,1.163827495208)))
REPRESENTATION_ITEM('')
SURFACE()
);
#171=(
BOUNDED_SURFACE()
B_SPLINE_SURFACE(3,3,((#33924,#33925,#33926,#33927,#33928,#33929,#33930,
#33931,#33932,#33933),(#33934,#33935,#33936,#33937,#33938,#33939,#33940,
#33941,#33942,#33943),(#33944,#33945,#33946,#33947,#33948,#33949,#33950,
#33951,#33952,#33953),(#33954,#33955,#33956,#33957,#33958,#33959,#33960,
#33961,#33962,#33963)),.UNSPECIFIED.,.F.,.F.,.F.)
B_SPLINE_SURFACE_WITH_KNOTS((4,4),(4,1,1,1,1,1,1,4),(0.,1.),(0.03540281776569,
0.1234679415063,0.2632035734038,0.4203296727887,0.5957836491349,0.789268501371,
1.,1.00911688994),.UNSPECIFIED.)
GEOMETRIC_REPRESENTATION_ITEM()
RATIONAL_B_SPLINE_SURFACE(((1.211236248281,1.211236248281,1.211236248281,
1.211236248281,1.211236248281,1.211236248281,1.211236248281,1.211236248281,
1.211236248281,1.211236248281),(0.9295879172397,0.9295879172397,0.9295879172397,
0.9295879172397,0.9295879172397,0.9295879172397,0.9295879172397,0.9295879172397,
0.9295879172397,0.9295879172397),(0.9295879172397,0.9295879172397,0.9295879172397,
0.9295879172397,0.9295879172397,0.9295879172397,0.9295879172397,0.9295879172397,
0.9295879172397,0.9295879172397),(1.211236248281,1.211236248281,1.211236248281,
1.211236248281,1.211236248281,1.211236248281,1.211236248281,1.211236248281,
1.211236248281,1.211236248281)))
REPRESENTATION_ITEM('')
SURFACE()
);
#172=(
BOUNDED_SURFACE()
B_SPLINE_SURFACE(3,3,((#34041,#34042,#34043,#34044,#34045,#34046,#34047,
#34048,#34049,#34050,#34051,#34052,#34053,#34054,#34055,#34056,#34057,#34058,
#34059),(#34060,#34061,#34062,#34063,#34064,#34065,#34066,#34067,#34068,
#34069,#34070,#34071,#34072,#34073,#34074,#34075,#34076,#34077,#34078),
(#34079,#34080,#34081,#34082,#34083,#34084,#34085,#34086,#34087,#34088,
#34089,#34090,#34091,#34092,#34093,#34094,#34095,#34096,#34097),(#34098,
#34099,#34100,#34101,#34102,#34103,#34104,#34105,#34106,#34107,#34108,#34109,
#34110,#34111,#34112,#34113,#34114,#34115,#34116)),.UNSPECIFIED.,.F.,.F.,
 .F.)
B_SPLINE_SURFACE_WITH_KNOTS((4,4),(4,1,1,1,1,1,1,1,1,1,1,1,1,1,1,1,4),(0.,
1.),(-0.01076426746053,0.,0.04152389901166,0.08394379225387,0.1302342687654,
0.1804523447143,0.2349355052966,0.2939338029969,0.3580057487009,0.4275129366519,
0.5025423241297,0.5839356639565,0.6731830882238,0.7717942958468,0.8805575045219,
1.,1.009808133051),.UNSPECIFIED.)
GEOMETRIC_REPRESENTATION_ITEM()
RATIONAL_B_SPLINE_SURFACE(((1.088372924818,1.088372924818,1.088372924818,
1.088372924818,1.088372924818,1.088372924818,1.088372924818,1.088372924818,
1.088372924818,1.088372924818,1.088372924818,1.088372924818,1.088372924818,
1.088372924818,1.088372924818,1.088372924818,1.088372924818,1.088372924818,
1.088372924818),(0.9705423583942,0.9705423583942,0.9705423583942,0.9705423583942,
0.9705423583942,0.9705423583942,0.9705423583942,0.9705423583942,0.9705423583942,
0.9705423583942,0.9705423583942,0.9705423583942,0.9705423583942,0.9705423583942,
0.9705423583942,0.9705423583942,0.9705423583942,0.9705423583942,0.9705423583942),
(0.9705423583942,0.9705423583942,0.9705423583942,0.9705423583942,0.9705423583942,
0.9705423583942,0.9705423583942,0.9705423583942,0.9705423583942,0.9705423583942,
0.9705423583942,0.9705423583942,0.9705423583942,0.9705423583942,0.9705423583942,
0.9705423583942,0.9705423583942,0.9705423583942,0.9705423583942),(1.088372924818,
1.088372924818,1.088372924818,1.088372924818,1.088372924818,1.088372924818,
1.088372924818,1.088372924818,1.088372924818,1.088372924818,1.088372924818,
1.088372924818,1.088372924818,1.088372924818,1.088372924818,1.088372924818,
1.088372924818,1.088372924818,1.088372924818)))
REPRESENTATION_ITEM('')
SURFACE()
);
#173=(
BOUNDED_SURFACE()
B_SPLINE_SURFACE(3,3,((#34117,#34118,#34119,#34120,#34121,#34122,#34123,
#34124,#34125,#34126,#34127,#34128),(#34129,#34130,#34131,#34132,#34133,
#34134,#34135,#34136,#34137,#34138,#34139,#34140),(#34141,#34142,#34143,
#34144,#34145,#34146,#34147,#34148,#34149,#34150,#34151,#34152),(#34153,
#34154,#34155,#34156,#34157,#34158,#34159,#34160,#34161,#34162,#34163,#34164)),
 .UNSPECIFIED.,.F.,.F.,.F.)
B_SPLINE_SURFACE_WITH_KNOTS((4,4),(4,1,1,1,1,1,1,1,1,4),(0.,1.),(-0.152618011925,
0.,0.1440925301842,0.2801219903658,0.4114391594101,0.5434056701778,0.6832645286048,
0.8346596058642,1.,1.152833582056),.UNSPECIFIED.)
GEOMETRIC_REPRESENTATION_ITEM()
RATIONAL_B_SPLINE_SURFACE(((1.000094023891,1.000094023891,1.000094023891,
1.000094023891,1.000094023891,1.000094023891,1.000094023891,1.000094023891,
1.000094023891,1.000094023891,1.000094023891,1.000094023891),(0.9999686587029,
0.9999686587029,0.9999686587029,0.9999686587029,0.9999686587029,0.9999686587029,
0.9999686587029,0.9999686587029,0.9999686587029,0.9999686587029,0.9999686587029,
0.9999686587029),(0.9999686587029,0.9999686587029,0.9999686587029,0.9999686587029,
0.9999686587029,0.9999686587029,0.9999686587029,0.9999686587029,0.9999686587029,
0.9999686587029,0.9999686587029,0.9999686587029),(1.000094023891,1.000094023891,
1.000094023891,1.000094023891,1.000094023891,1.000094023891,1.000094023891,
1.000094023891,1.000094023891,1.000094023891,1.000094023891,1.000094023891)))
REPRESENTATION_ITEM('')
SURFACE()
);
#174=(
BOUNDED_SURFACE()
B_SPLINE_SURFACE(3,3,((#34166,#34167,#34168,#34169,#34170,#34171,#34172,
#34173,#34174,#34175),(#34176,#34177,#34178,#34179,#34180,#34181,#34182,
#34183,#34184,#34185),(#34186,#34187,#34188,#34189,#34190,#34191,#34192,
#34193,#34194,#34195),(#34196,#34197,#34198,#34199,#34200,#34201,#34202,
#34203,#34204,#34205)),.UNSPECIFIED.,.F.,.F.,.F.)
B_SPLINE_SURFACE_WITH_KNOTS((4,4),(4,1,1,1,1,1,1,4),(0.,1.),(-0.009053405764054,
0.,0.2128253131466,0.4067103404652,0.5817418357977,0.7383188923361,0.8773475428248,
0.9585687317144),.UNSPECIFIED.)
GEOMETRIC_REPRESENTATION_ITEM()
RATIONAL_B_SPLINE_SURFACE(((1.211237524847,1.211237524847,1.211237524847,
1.211237524847,1.211237524847,1.211237524847,1.211237524847,1.211237524847,
1.211237524847,1.211237524847),(0.9295874917176,0.9295874917176,0.9295874917176,
0.9295874917176,0.9295874917176,0.9295874917176,0.9295874917176,0.9295874917176,
0.9295874917176,0.9295874917176),(0.9295874917176,0.9295874917176,0.9295874917176,
0.9295874917176,0.9295874917176,0.9295874917176,0.9295874917176,0.9295874917176,
0.9295874917176,0.9295874917176),(1.211237524847,1.211237524847,1.211237524847,
1.211237524847,1.211237524847,1.211237524847,1.211237524847,1.211237524847,
1.211237524847,1.211237524847)))
REPRESENTATION_ITEM('')
SURFACE()
);
#175=(
BOUNDED_SURFACE()
B_SPLINE_SURFACE(3,3,((#34282,#34283,#34284,#34285,#34286,#34287,#34288,
#34289,#34290,#34291,#34292,#34293,#34294,#34295,#34296,#34297,#34298,#34299),
(#34300,#34301,#34302,#34303,#34304,#34305,#34306,#34307,#34308,#34309,
#34310,#34311,#34312,#34313,#34314,#34315,#34316,#34317),(#34318,#34319,
#34320,#34321,#34322,#34323,#34324,#34325,#34326,#34327,#34328,#34329,#34330,
#34331,#34332,#34333,#34334,#34335),(#34336,#34337,#34338,#34339,#34340,
#34341,#34342,#34343,#34344,#34345,#34346,#34347,#34348,#34349,#34350,#34351,
#34352,#34353)),.UNSPECIFIED.,.F.,.F.,.F.)
B_SPLINE_SURFACE_WITH_KNOTS((4,4),(4,1,1,1,1,1,1,1,1,1,1,1,1,1,1,4),(0.,
1.),(-0.009797090891202,0.,0.1252864769222,0.2381332273333,0.3395214867139,
0.4311702756169,0.5147945964105,0.5913458810972,0.6613379006761,0.7254151205055,
0.7843391271186,0.8380935847805,0.8886737238581,0.9411160876025,1.,1.010696795736),
 .UNSPECIFIED.)
GEOMETRIC_REPRESENTATION_ITEM()
RATIONAL_B_SPLINE_SURFACE(((1.088374512803,1.088374512803,1.088374512803,
1.088374512803,1.088374512803,1.088374512803,1.088374512803,1.088374512803,
1.088374512803,1.088374512803,1.088374512803,1.088374512803,1.088374512803,
1.088374512803,1.088374512803,1.088374512803,1.088374512803,1.088374512803),
(0.9705418290655,0.9705418290655,0.9705418290655,0.9705418290655,0.9705418290655,
0.9705418290655,0.9705418290655,0.9705418290655,0.9705418290655,0.9705418290655,
0.9705418290655,0.9705418290655,0.9705418290655,0.9705418290655,0.9705418290655,
0.9705418290655,0.9705418290655,0.9705418290655),(0.9705418290655,0.9705418290655,
0.9705418290655,0.9705418290655,0.9705418290655,0.9705418290655,0.9705418290655,
0.9705418290655,0.9705418290655,0.9705418290655,0.9705418290655,0.9705418290655,
0.9705418290655,0.9705418290655,0.9705418290655,0.9705418290655,0.9705418290655,
0.9705418290655),(1.088374512803,1.088374512803,1.088374512803,1.088374512803,
1.088374512803,1.088374512803,1.088374512803,1.088374512803,1.088374512803,
1.088374512803,1.088374512803,1.088374512803,1.088374512803,1.088374512803,
1.088374512803,1.088374512803,1.088374512803,1.088374512803)))
REPRESENTATION_ITEM('')
SURFACE()
);
#176=(
BOUNDED_SURFACE()
B_SPLINE_SURFACE(3,3,((#34354,#34355,#34356,#34357,#34358,#34359,#34360,
#34361,#34362,#34363,#34364),(#34365,#34366,#34367,#34368,#34369,#34370,
#34371,#34372,#34373,#34374,#34375),(#34376,#34377,#34378,#34379,#34380,
#34381,#34382,#34383,#34384,#34385,#34386),(#34387,#34388,#34389,#34390,
#34391,#34392,#34393,#34394,#34395,#34396,#34397)),.UNSPECIFIED.,.F.,.F.,
 .F.)
B_SPLINE_SURFACE_WITH_KNOTS((4,4),(4,1,1,1,1,1,1,1,4),(0.,1.),(-0.04050719629992,
0.,0.2121825428154,0.403201234845,0.5756502932434,0.7316337186034,0.8727661988069,
1.,1.048418925808),.UNSPECIFIED.)
GEOMETRIC_REPRESENTATION_ITEM()
RATIONAL_B_SPLINE_SURFACE(((1.008087784168,1.008087784168,1.008087784168,
1.008087784168,1.008087784168,1.008087784168,1.008087784168,1.008087784168,
1.008087784168,1.008087784168,1.008087784168),(0.997304071944,0.997304071944,
0.997304071944,0.997304071944,0.997304071944,0.997304071944,0.997304071944,
0.997304071944,0.997304071944,0.997304071944,0.997304071944),(0.997304071944,
0.997304071944,0.997304071944,0.997304071944,0.997304071944,0.997304071944,
0.997304071944,0.997304071944,0.997304071944,0.997304071944,0.997304071944),
(1.008087784168,1.008087784168,1.008087784168,1.008087784168,1.008087784168,
1.008087784168,1.008087784168,1.008087784168,1.008087784168,1.008087784168,
1.008087784168)))
REPRESENTATION_ITEM('')
SURFACE()
);
#177=(
BOUNDED_SURFACE()
B_SPLINE_SURFACE(3,3,((#34432,#34433,#34434,#34435,#34436,#34437,#34438),
(#34439,#34440,#34441,#34442,#34443,#34444,#34445),(#34446,#34447,#34448,
#34449,#34450,#34451,#34452),(#34453,#34454,#34455,#34456,#34457,#34458,
#34459)),.UNSPECIFIED.,.F.,.F.,.F.)
B_SPLINE_SURFACE_WITH_KNOTS((4,4),(4,1,1,1,4),(0.,1.),(-0.02191865670977,
0.,0.3711108308406,0.7030029886383,0.86664181477),.UNSPECIFIED.)
GEOMETRIC_REPRESENTATION_ITEM()
RATIONAL_B_SPLINE_SURFACE(((1.201671391236,1.201671391236,1.201671391236,
1.201671391236,1.201671391236,1.201671391236,1.201671391236),(0.9327762029212,
0.9327762029212,0.9327762029212,0.9327762029212,0.9327762029212,0.9327762029212,
0.9327762029212),(0.9327762029212,0.9327762029212,0.9327762029212,0.9327762029212,
0.9327762029212,0.9327762029212,0.9327762029212),(1.201671391236,1.201671391236,
1.201671391236,1.201671391236,1.201671391236,1.201671391236,1.201671391236)))
REPRESENTATION_ITEM('')
SURFACE()
);
#178=(
BOUNDED_SURFACE()
B_SPLINE_SURFACE(3,3,((#34461,#34462,#34463,#34464,#34465,#34466,#34467,
#34468),(#34469,#34470,#34471,#34472,#34473,#34474,#34475,#34476),(#34477,
#34478,#34479,#34480,#34481,#34482,#34483,#34484),(#34485,#34486,#34487,
#34488,#34489,#34490,#34491,#34492)),.UNSPECIFIED.,.F.,.F.,.F.)
B_SPLINE_SURFACE_WITH_KNOTS((4,4),(4,1,1,1,1,4),(0.,1.),(-0.01121526815079,
0.,0.3190669955162,0.6396376709117,1.,1.01119406465),.UNSPECIFIED.)
GEOMETRIC_REPRESENTATION_ITEM()
RATIONAL_B_SPLINE_SURFACE(((1.095350229537,1.095350229537,1.095350229537,
1.095350229537,1.095350229537,1.095350229537,1.095350229537,1.095350229537),
(0.9682165901542,0.9682165901542,0.9682165901542,0.9682165901542,0.9682165901542,
0.9682165901542,0.9682165901542,0.9682165901542),(0.9682165901542,0.9682165901542,
0.9682165901542,0.9682165901542,0.9682165901542,0.9682165901542,0.9682165901542,
0.9682165901542),(1.095350229537,1.095350229537,1.095350229537,1.095350229537,
1.095350229537,1.095350229537,1.095350229537,1.095350229537)))
REPRESENTATION_ITEM('')
SURFACE()
);
#179=(
BOUNDED_SURFACE()
B_SPLINE_SURFACE(3,3,((#34494,#34495,#34496,#34497,#34498,#34499,#34500,
#34501),(#34502,#34503,#34504,#34505,#34506,#34507,#34508,#34509),(#34510,
#34511,#34512,#34513,#34514,#34515,#34516,#34517),(#34518,#34519,#34520,
#34521,#34522,#34523,#34524,#34525)),.UNSPECIFIED.,.F.,.F.,.F.)
B_SPLINE_SURFACE_WITH_KNOTS((4,4),(4,1,1,1,1,4),(0.,1.),(-0.01123151971552,
0.,0.3226324635879,0.6411683732307,1.,1.011214131133),.UNSPECIFIED.)
GEOMETRIC_REPRESENTATION_ITEM()
RATIONAL_B_SPLINE_SURFACE(((1.095350237893,1.095350237893,1.095350237893,
1.095350237893,1.095350237893,1.095350237893,1.095350237893,1.095350237893),
(0.9682165873689,0.9682165873689,0.9682165873689,0.9682165873689,0.9682165873689,
0.9682165873689,0.9682165873689,0.9682165873689),(0.9682165873689,0.9682165873689,
0.9682165873689,0.9682165873689,0.9682165873689,0.9682165873689,0.9682165873689,
0.9682165873689),(1.095350237893,1.095350237893,1.095350237893,1.095350237893,
1.095350237893,1.095350237893,1.095350237893,1.095350237893)))
REPRESENTATION_ITEM('')
SURFACE()
);
#180=(
BOUNDED_SURFACE()
B_SPLINE_SURFACE(3,3,((#43761,#43762,#43763,#43764,#43765,#43766,#43767,
#43768,#43769,#43770,#43771,#43772,#43773,#43774,#43775),(#43776,#43777,
#43778,#43779,#43780,#43781,#43782,#43783,#43784,#43785,#43786,#43787,#43788,
#43789,#43790),(#43791,#43792,#43793,#43794,#43795,#43796,#43797,#43798,
#43799,#43800,#43801,#43802,#43803,#43804,#43805),(#43806,#43807,#43808,
#43809,#43810,#43811,#43812,#43813,#43814,#43815,#43816,#43817,#43818,#43819,
#43820)),.UNSPECIFIED.,.F.,.F.,.F.)
B_SPLINE_SURFACE_WITH_KNOTS((4,4),(4,1,1,1,1,1,1,1,1,1,1,1,4),(0.,1.),(-0.02367250505126,
0.,0.1568376273924,0.2958784950045,0.4193835102427,0.5294996966959,0.6286414323947,
0.7182158704286,0.7992496439752,0.8730760680591,0.9399209839788,1.,1.025375300283),
 .UNSPECIFIED.)
GEOMETRIC_REPRESENTATION_ITEM()
RATIONAL_B_SPLINE_SURFACE(((1.19686984414,1.19686984414,1.19686984414,1.19686984414,
1.19686984414,1.19686984414,1.19686984414,1.19686984414,1.19686984414,1.19686984414,
1.19686984414,1.19686984414,1.19686984414,1.19686984414,1.19686984414),
(0.9343767186201,0.9343767186201,0.9343767186201,0.9343767186201,0.9343767186201,
0.9343767186201,0.9343767186201,0.9343767186201,0.9343767186201,0.9343767186201,
0.9343767186201,0.9343767186201,0.9343767186201,0.9343767186201,0.9343767186201),
(0.9343767186201,0.9343767186201,0.9343767186201,0.9343767186201,0.9343767186201,
0.9343767186201,0.9343767186201,0.9343767186201,0.9343767186201,0.9343767186201,
0.9343767186201,0.9343767186201,0.9343767186201,0.9343767186201,0.9343767186201),
(1.19686984414,1.19686984414,1.19686984414,1.19686984414,1.19686984414,
1.19686984414,1.19686984414,1.19686984414,1.19686984414,1.19686984414,1.19686984414,
1.19686984414,1.19686984414,1.19686984414,1.19686984414)))
REPRESENTATION_ITEM('')
SURFACE()
);
#181=(
BOUNDED_SURFACE()
B_SPLINE_SURFACE(3,3,((#43843,#43844,#43845,#43846,#43847,#43848,#43849,
#43850,#43851,#43852,#43853,#43854,#43855,#43856,#43857),(#43858,#43859,
#43860,#43861,#43862,#43863,#43864,#43865,#43866,#43867,#43868,#43869,#43870,
#43871,#43872),(#43873,#43874,#43875,#43876,#43877,#43878,#43879,#43880,
#43881,#43882,#43883,#43884,#43885,#43886,#43887),(#43888,#43889,#43890,
#43891,#43892,#43893,#43894,#43895,#43896,#43897,#43898,#43899,#43900,#43901,
#43902)),.UNSPECIFIED.,.F.,.F.,.F.)
B_SPLINE_SURFACE_WITH_KNOTS((4,4),(4,1,1,1,1,1,1,1,1,1,1,1,4),(0.,1.),(-0.02541201080131,
0.,0.06012137477617,0.127023679674,0.2009097013355,0.2820155865859,0.3717063075714,
0.470928205433,0.5809950476801,0.7044646083568,0.8434955500304,1.,1.023466062398),
 .UNSPECIFIED.)
GEOMETRIC_REPRESENTATION_ITEM()
RATIONAL_B_SPLINE_SURFACE(((1.196861975576,1.196861975576,1.196861975576,
1.196861975576,1.196861975576,1.196861975576,1.196861975576,1.196861975576,
1.196861975576,1.196861975576,1.196861975576,1.196861975576,1.196861975576,
1.196861975576,1.196861975576),(0.9343793414748,0.9343793414748,0.9343793414748,
0.9343793414748,0.9343793414748,0.9343793414748,0.9343793414748,0.9343793414748,
0.9343793414748,0.9343793414748,0.9343793414748,0.9343793414748,0.9343793414748,
0.9343793414748,0.9343793414748),(0.9343793414748,0.9343793414748,0.9343793414748,
0.9343793414748,0.9343793414748,0.9343793414748,0.9343793414748,0.9343793414748,
0.9343793414748,0.9343793414748,0.9343793414748,0.9343793414748,0.9343793414748,
0.9343793414748,0.9343793414748),(1.196861975576,1.196861975576,1.196861975576,
1.196861975576,1.196861975576,1.196861975576,1.196861975576,1.196861975576,
1.196861975576,1.196861975576,1.196861975576,1.196861975576,1.196861975576,
1.196861975576,1.196861975576)))
REPRESENTATION_ITEM('')
SURFACE()
);
#182=(
BOUNDED_SURFACE()
B_SPLINE_SURFACE(3,3,((#44165,#44166,#44167,#44168,#44169,#44170,#44171,
#44172,#44173,#44174,#44175,#44176,#44177,#44178,#44179,#44180,#44181,#44182,
#44183,#44184,#44185),(#44186,#44187,#44188,#44189,#44190,#44191,#44192,
#44193,#44194,#44195,#44196,#44197,#44198,#44199,#44200,#44201,#44202,#44203,
#44204,#44205,#44206),(#44207,#44208,#44209,#44210,#44211,#44212,#44213,
#44214,#44215,#44216,#44217,#44218,#44219,#44220,#44221,#44222,#44223,#44224,
#44225,#44226,#44227),(#44228,#44229,#44230,#44231,#44232,#44233,#44234,
#44235,#44236,#44237,#44238,#44239,#44240,#44241,#44242,#44243,#44244,#44245,
#44246,#44247,#44248)),.UNSPECIFIED.,.F.,.F.,.F.)
B_SPLINE_SURFACE_WITH_KNOTS((4,4),(4,1,1,1,1,1,1,1,1,1,1,1,1,1,1,1,1,1,
4),(0.,1.),(-0.004474348485776,0.,0.02230597305244,0.04333157365729,0.06387325262822,
0.08408116383947,0.1041708278111,0.1243458370088,0.1448121265696,0.1657786860045,
0.187470853701,0.210486087144,0.2358855836333,0.2645487659469,0.2971408212892,
0.3344049750459,0.3761308583034,0.4203483673292,0.4513668076816),
 .UNSPECIFIED.)
GEOMETRIC_REPRESENTATION_ITEM()
RATIONAL_B_SPLINE_SURFACE(((1.162548312769,1.162548312769,1.162548312769,
1.162548312769,1.162548312769,1.162548312769,1.162548312769,1.162548312769,
1.162548312769,1.162548312769,1.162548312769,1.162548312769,1.162548312769,
1.162548312769,1.162548312769,1.162548312769,1.162548312769,1.162548312769,
1.162548312769,1.162548312769,1.162548312769),(0.9458172290769,0.9458172290769,
0.9458172290769,0.9458172290769,0.9458172290769,0.9458172290769,0.9458172290769,
0.9458172290769,0.9458172290769,0.9458172290769,0.9458172290769,0.9458172290769,
0.9458172290769,0.9458172290769,0.9458172290769,0.9458172290769,0.9458172290769,
0.9458172290769,0.9458172290769,0.9458172290769,0.9458172290769),(0.9458172290769,
0.9458172290769,0.9458172290769,0.9458172290769,0.9458172290769,0.9458172290769,
0.9458172290769,0.9458172290769,0.9458172290769,0.9458172290769,0.9458172290769,
0.9458172290769,0.9458172290769,0.9458172290769,0.9458172290769,0.9458172290769,
0.9458172290769,0.9458172290769,0.9458172290769,0.9458172290769,0.9458172290769),
(1.162548312769,1.162548312769,1.162548312769,1.162548312769,1.162548312769,
1.162548312769,1.162548312769,1.162548312769,1.162548312769,1.162548312769,
1.162548312769,1.162548312769,1.162548312769,1.162548312769,1.162548312769,
1.162548312769,1.162548312769,1.162548312769,1.162548312769,1.162548312769,
1.162548312769)))
REPRESENTATION_ITEM('')
SURFACE()
);
#183=(
BOUNDED_SURFACE()
B_SPLINE_SURFACE(3,3,((#44380,#44381,#44382,#44383,#44384,#44385,#44386,
#44387,#44388,#44389,#44390,#44391,#44392,#44393,#44394,#44395,#44396,#44397,
#44398,#44399,#44400,#44401,#44402),(#44403,#44404,#44405,#44406,#44407,
#44408,#44409,#44410,#44411,#44412,#44413,#44414,#44415,#44416,#44417,#44418,
#44419,#44420,#44421,#44422,#44423,#44424,#44425),(#44426,#44427,#44428,
#44429,#44430,#44431,#44432,#44433,#44434,#44435,#44436,#44437,#44438,#44439,
#44440,#44441,#44442,#44443,#44444,#44445,#44446,#44447,#44448),(#44449,
#44450,#44451,#44452,#44453,#44454,#44455,#44456,#44457,#44458,#44459,#44460,
#44461,#44462,#44463,#44464,#44465,#44466,#44467,#44468,#44469,#44470,#44471)),
 .UNSPECIFIED.,.F.,.F.,.F.)
B_SPLINE_SURFACE_WITH_KNOTS((4,4),(4,1,1,1,1,1,1,1,1,1,1,1,1,1,1,1,1,1,
1,1,4),(0.,1.),(0.4402361434422,0.4558088659294,0.476422669633,0.4969107659322,
0.5173847665671,0.5378040004898,0.5584587769075,0.5804853326365,0.6053681688744,
0.6337471320501,0.6648770320844,0.697628000239,0.7315220485564,0.7658606197272,
0.7995217313545,0.8327434657359,0.8676912667687,0.9066066156032,0.9504140537645,
1.,1.005363326625),.UNSPECIFIED.)
GEOMETRIC_REPRESENTATION_ITEM()
RATIONAL_B_SPLINE_SURFACE(((1.224498979605,1.224498979605,1.224498979605,
1.224498979605,1.224498979605,1.224498979605,1.224498979605,1.224498979605,
1.224498979605,1.224498979605,1.224498979605,1.224498979605,1.224498979605,
1.224498979605,1.224498979605,1.224498979605,1.224498979605,1.224498979605,
1.224498979605,1.224498979605,1.224498979605,1.224498979605,1.224498979605),
(0.9251670067983,0.9251670067983,0.9251670067983,0.9251670067983,0.9251670067983,
0.9251670067983,0.9251670067983,0.9251670067983,0.9251670067983,0.9251670067983,
0.9251670067983,0.9251670067983,0.9251670067983,0.9251670067983,0.9251670067983,
0.9251670067983,0.9251670067983,0.9251670067983,0.9251670067983,0.9251670067983,
0.9251670067983,0.9251670067983,0.9251670067983),(0.9251670067983,0.9251670067983,
0.9251670067983,0.9251670067983,0.9251670067983,0.9251670067983,0.9251670067983,
0.9251670067983,0.9251670067983,0.9251670067983,0.9251670067983,0.9251670067983,
0.9251670067983,0.9251670067983,0.9251670067983,0.9251670067983,0.9251670067983,
0.9251670067983,0.9251670067983,0.9251670067983,0.9251670067983,0.9251670067983,
0.9251670067983),(1.224498979605,1.224498979605,1.224498979605,1.224498979605,
1.224498979605,1.224498979605,1.224498979605,1.224498979605,1.224498979605,
1.224498979605,1.224498979605,1.224498979605,1.224498979605,1.224498979605,
1.224498979605,1.224498979605,1.224498979605,1.224498979605,1.224498979605,
1.224498979605,1.224498979605,1.224498979605,1.224498979605)))
REPRESENTATION_ITEM('')
SURFACE()
);
#184=(
BOUNDED_SURFACE()
B_SPLINE_SURFACE(3,3,((#44501,#44502,#44503,#44504,#44505,#44506,#44507,
#44508),(#44509,#44510,#44511,#44512,#44513,#44514,#44515,#44516),(#44517,
#44518,#44519,#44520,#44521,#44522,#44523,#44524),(#44525,#44526,#44527,
#44528,#44529,#44530,#44531,#44532)),.UNSPECIFIED.,.F.,.F.,.F.)
B_SPLINE_SURFACE_WITH_KNOTS((4,4),(4,1,1,1,1,4),(0.,1.),(-0.02000817581934,
0.,0.3335678568848,0.6667501113936,1.,1.020000171272),.UNSPECIFIED.)
GEOMETRIC_REPRESENTATION_ITEM()
RATIONAL_B_SPLINE_SURFACE(((1.001084776474,1.001084776474,1.001084776474,
1.001084776474,1.001084776474,1.001084776474,1.001084776474,1.001084776474),
(0.9996384078421,0.9996384078421,0.9996384078421,0.9996384078421,0.9996384078421,
0.9996384078421,0.9996384078421,0.9996384078421),(0.9996384078421,0.9996384078421,
0.9996384078421,0.9996384078421,0.9996384078421,0.9996384078421,0.9996384078421,
0.9996384078421),(1.001084776474,1.001084776474,1.001084776474,1.001084776474,
1.001084776474,1.001084776474,1.001084776474,1.001084776474)))
REPRESENTATION_ITEM('')
SURFACE()
);
#185=(
BOUNDED_SURFACE()
B_SPLINE_SURFACE(3,3,((#44717,#44718,#44719,#44720,#44721,#44722,#44723,
#44724,#44725),(#44726,#44727,#44728,#44729,#44730,#44731,#44732,#44733,
#44734),(#44735,#44736,#44737,#44738,#44739,#44740,#44741,#44742,#44743),
(#44744,#44745,#44746,#44747,#44748,#44749,#44750,#44751,#44752)),
 .UNSPECIFIED.,.F.,.F.,.F.)
B_SPLINE_SURFACE_WITH_KNOTS((4,4),(4,1,1,1,1,1,4),(0.,1.),(0.01341438395161,
0.2268259504049,0.4456307994234,0.6496269485443,0.8352622055157,1.,1.015518229442),
 .UNSPECIFIED.)
GEOMETRIC_REPRESENTATION_ITEM()
RATIONAL_B_SPLINE_SURFACE(((1.058064131412,1.058064131412,1.058064131412,
1.058064131412,1.058064131412,1.058064131412,1.058064131412,1.058064131412,
1.058064131412),(0.9806452895294,0.9806452895294,0.9806452895294,0.9806452895294,
0.9806452895294,0.9806452895294,0.9806452895294,0.9806452895294,0.9806452895294),
(0.9806452895294,0.9806452895294,0.9806452895294,0.9806452895294,0.9806452895294,
0.9806452895294,0.9806452895294,0.9806452895294,0.9806452895294),(1.058064131412,
1.058064131412,1.058064131412,1.058064131412,1.058064131412,1.058064131412,
1.058064131412,1.058064131412,1.058064131412)))
REPRESENTATION_ITEM('')
SURFACE()
);
#186=(
BOUNDED_SURFACE()
B_SPLINE_SURFACE(3,3,((#44798,#44799,#44800,#44801,#44802,#44803,#44804,
#44805,#44806,#44807,#44808),(#44809,#44810,#44811,#44812,#44813,#44814,
#44815,#44816,#44817,#44818,#44819),(#44820,#44821,#44822,#44823,#44824,
#44825,#44826,#44827,#44828,#44829,#44830),(#44831,#44832,#44833,#44834,
#44835,#44836,#44837,#44838,#44839,#44840,#44841)),.UNSPECIFIED.,.F.,.F.,
 .F.)
B_SPLINE_SURFACE_WITH_KNOTS((4,4),(4,1,1,1,1,1,1,1,4),(0.,1.),(-0.01514694021523,
0.,0.1434382549194,0.2925803126927,0.4539877256396,0.6288947339363,0.8127593843745,
1.,1.01468871823),.UNSPECIFIED.)
GEOMETRIC_REPRESENTATION_ITEM()
RATIONAL_B_SPLINE_SURFACE(((1.091722184379,1.091722184379,1.091722184379,
1.091722184379,1.091722184379,1.091722184379,1.091722184379,1.091722184379,
1.091722184379,1.091722184379,1.091722184379),(0.9694259385405,0.9694259385405,
0.9694259385405,0.9694259385405,0.9694259385405,0.9694259385405,0.9694259385405,
0.9694259385405,0.9694259385405,0.9694259385405,0.9694259385405),(0.9694259385405,
0.9694259385405,0.9694259385405,0.9694259385405,0.9694259385405,0.9694259385405,
0.9694259385405,0.9694259385405,0.9694259385405,0.9694259385405,0.9694259385405),
(1.091722184379,1.091722184379,1.091722184379,1.091722184379,1.091722184379,
1.091722184379,1.091722184379,1.091722184379,1.091722184379,1.091722184379,
1.091722184379)))
REPRESENTATION_ITEM('')
SURFACE()
);
#187=(
BOUNDED_SURFACE()
B_SPLINE_SURFACE(3,3,((#44843,#44844,#44845,#44846,#44847,#44848,#44849,
#44850,#44851,#44852),(#44853,#44854,#44855,#44856,#44857,#44858,#44859,
#44860,#44861,#44862),(#44863,#44864,#44865,#44866,#44867,#44868,#44869,
#44870,#44871,#44872),(#44873,#44874,#44875,#44876,#44877,#44878,#44879,
#44880,#44881,#44882)),.UNSPECIFIED.,.F.,.F.,.F.)
B_SPLINE_SURFACE_WITH_KNOTS((4,4),(4,1,1,1,1,1,1,4),(0.,1.),(-0.1017343672885,
0.,0.1958839083417,0.3858642890747,0.5744654073669,0.7741715521339,1.,1.116420456884),
 .UNSPECIFIED.)
GEOMETRIC_REPRESENTATION_ITEM()
RATIONAL_B_SPLINE_SURFACE(((1.126722516535,1.126722516535,1.126722516535,
1.126722516535,1.126722516535,1.126722516535,1.126722516535,1.126722516535,
1.126722516535,1.126722516535),(0.9577591611551,0.9577591611551,0.9577591611551,
0.9577591611551,0.9577591611551,0.9577591611551,0.9577591611551,0.9577591611551,
0.9577591611551,0.9577591611551),(0.9577591611551,0.9577591611551,0.9577591611551,
0.9577591611551,0.9577591611551,0.9577591611551,0.9577591611551,0.9577591611551,
0.9577591611551,0.9577591611551),(1.126722516535,1.126722516535,1.126722516535,
1.126722516535,1.126722516535,1.126722516535,1.126722516535,1.126722516535,
1.126722516535,1.126722516535)))
REPRESENTATION_ITEM('')
SURFACE()
);
#188=(
BOUNDED_SURFACE()
B_SPLINE_SURFACE(3,3,((#44916,#44917,#44918,#44919,#44920,#44921,#44922,
#44923,#44924,#44925,#44926,#44927,#44928,#44929),(#44930,#44931,#44932,
#44933,#44934,#44935,#44936,#44937,#44938,#44939,#44940,#44941,#44942,#44943),
(#44944,#44945,#44946,#44947,#44948,#44949,#44950,#44951,#44952,#44953,
#44954,#44955,#44956,#44957),(#44958,#44959,#44960,#44961,#44962,#44963,
#44964,#44965,#44966,#44967,#44968,#44969,#44970,#44971)),.UNSPECIFIED.,
 .F.,.F.,.F.)
B_SPLINE_SURFACE_WITH_KNOTS((4,4),(4,1,1,1,1,1,1,1,1,1,1,4),(0.,1.),(-0.01844658935295,
0.,0.1044814008579,0.2134723510049,0.3264520754444,0.4425667333534,0.5596708840584,
0.6752555152391,0.7879010159006,0.8964334098892,1.,1.018329622104),
 .UNSPECIFIED.)
GEOMETRIC_REPRESENTATION_ITEM()
RATIONAL_B_SPLINE_SURFACE(((1.093920437843,1.093920437843,1.093920437843,
1.093920437843,1.093920437843,1.093920437843,1.093920437843,1.093920437843,
1.093920437843,1.093920437843,1.093920437843,1.093920437843,1.093920437843,
1.093920437843),(0.9686931873855,0.9686931873855,0.9686931873855,0.9686931873855,
0.9686931873855,0.9686931873855,0.9686931873855,0.9686931873855,0.9686931873855,
0.9686931873855,0.9686931873855,0.9686931873855,0.9686931873855,0.9686931873855),
(0.9686931873855,0.9686931873855,0.9686931873855,0.9686931873855,0.9686931873855,
0.9686931873855,0.9686931873855,0.9686931873855,0.9686931873855,0.9686931873855,
0.9686931873855,0.9686931873855,0.9686931873855,0.9686931873855),(1.093920437843,
1.093920437843,1.093920437843,1.093920437843,1.093920437843,1.093920437843,
1.093920437843,1.093920437843,1.093920437843,1.093920437843,1.093920437843,
1.093920437843,1.093920437843,1.093920437843)))
REPRESENTATION_ITEM('')
SURFACE()
);
#189=(
BOUNDED_SURFACE()
B_SPLINE_SURFACE(3,3,((#45064,#45065,#45066,#45067,#45068,#45069,#45070,
#45071,#45072,#45073,#45074,#45075),(#45076,#45077,#45078,#45079,#45080,
#45081,#45082,#45083,#45084,#45085,#45086,#45087),(#45088,#45089,#45090,
#45091,#45092,#45093,#45094,#45095,#45096,#45097,#45098,#45099),(#45100,
#45101,#45102,#45103,#45104,#45105,#45106,#45107,#45108,#45109,#45110,#45111)),
 .UNSPECIFIED.,.F.,.F.,.F.)
B_SPLINE_SURFACE_WITH_KNOTS((4,4),(4,1,1,1,1,1,1,1,1,4),(0.,1.),(-0.030614617578,
0.,0.1495462512719,0.2937414136624,0.4389937202877,0.5830269670076,0.7175783131859,
0.8510090101071,1.,1.030661227764),.UNSPECIFIED.)
GEOMETRIC_REPRESENTATION_ITEM()
RATIONAL_B_SPLINE_SURFACE(((1.129761691476,1.129761691476,1.129761691476,
1.129761691476,1.129761691476,1.129761691476,1.129761691476,1.129761691476,
1.129761691476,1.129761691476,1.129761691476,1.129761691476),(0.9567461028415,
0.9567461028415,0.9567461028415,0.9567461028415,0.9567461028415,0.9567461028415,
0.9567461028415,0.9567461028415,0.9567461028415,0.9567461028415,0.9567461028415,
0.9567461028415),(0.9567461028415,0.9567461028415,0.9567461028415,0.9567461028415,
0.9567461028415,0.9567461028415,0.9567461028415,0.9567461028415,0.9567461028415,
0.9567461028415,0.9567461028415,0.9567461028415),(1.129761691476,1.129761691476,
1.129761691476,1.129761691476,1.129761691476,1.129761691476,1.129761691476,
1.129761691476,1.129761691476,1.129761691476,1.129761691476,1.129761691476)))
REPRESENTATION_ITEM('')
SURFACE()
);
#190=(
BOUNDED_SURFACE()
B_SPLINE_SURFACE(2,2,((#45185,#45186,#45187),(#45188,#45189,#45190),(#45191,
#45192,#45193)),.UNSPECIFIED.,.F.,.F.,.F.)
B_SPLINE_SURFACE_WITH_KNOTS((3,3),(3,3),(-1.57079632679603,1.03155351707746E-11),
(-0.78539816371462,0.785398163714621),.UNSPECIFIED.)
GEOMETRIC_REPRESENTATION_ITEM()
RATIONAL_B_SPLINE_SURFACE(((1.,0.707106780962273,1.),(0.707106781182504,
0.499999999838555,0.707106781182504),(1.,0.707106780962273,1.)))
REPRESENTATION_ITEM('')
SURFACE()
);
#191=(
BOUNDED_SURFACE()
B_SPLINE_SURFACE(3,3,((#45244,#45245,#45246,#45247,#45248,#45249,#45250,
#45251,#45252,#45253,#45254,#45255,#45256,#45257,#45258,#45259,#45260,#45261,
#45262,#45263),(#45264,#45265,#45266,#45267,#45268,#45269,#45270,#45271,
#45272,#45273,#45274,#45275,#45276,#45277,#45278,#45279,#45280,#45281,#45282,
#45283),(#45284,#45285,#45286,#45287,#45288,#45289,#45290,#45291,#45292,
#45293,#45294,#45295,#45296,#45297,#45298,#45299,#45300,#45301,#45302,#45303),
(#45304,#45305,#45306,#45307,#45308,#45309,#45310,#45311,#45312,#45313,
#45314,#45315,#45316,#45317,#45318,#45319,#45320,#45321,#45322,#45323)),
 .UNSPECIFIED.,.F.,.F.,.F.)
B_SPLINE_SURFACE_WITH_KNOTS((4,4),(4,1,1,1,1,1,1,1,1,1,1,1,1,1,1,1,1,4),
(0.,1.),(0.5974830130601,0.6214330811425,0.6582317938511,0.6909396382487,
0.7201206288693,0.746316287089,0.7702754291775,0.7929187871877,0.814921182593,
0.8365329597553,0.8579099550699,0.8792500682455,0.9008111437527,0.9227739349606,
0.9458934201391,0.9712943791051,1.,1.003985211551),.UNSPECIFIED.)
GEOMETRIC_REPRESENTATION_ITEM()
RATIONAL_B_SPLINE_SURFACE(((1.163141288766,1.163141288766,1.163141288766,
1.163141288766,1.163141288766,1.163141288766,1.163141288766,1.163141288766,
1.163141288766,1.163141288766,1.163141288766,1.163141288766,1.163141288766,
1.163141288766,1.163141288766,1.163141288766,1.163141288766,1.163141288766,
1.163141288766,1.163141288766),(0.9456195704113,0.9456195704113,0.9456195704113,
0.9456195704113,0.9456195704113,0.9456195704113,0.9456195704113,0.9456195704113,
0.9456195704113,0.9456195704113,0.9456195704113,0.9456195704113,0.9456195704113,
0.9456195704113,0.9456195704113,0.9456195704113,0.9456195704113,0.9456195704113,
0.9456195704113,0.9456195704113),(0.9456195704113,0.9456195704113,0.9456195704113,
0.9456195704113,0.9456195704113,0.9456195704113,0.9456195704113,0.9456195704113,
0.9456195704113,0.9456195704113,0.9456195704113,0.9456195704113,0.9456195704113,
0.9456195704113,0.9456195704113,0.9456195704113,0.9456195704113,0.9456195704113,
0.9456195704113,0.9456195704113),(1.163141288766,1.163141288766,1.163141288766,
1.163141288766,1.163141288766,1.163141288766,1.163141288766,1.163141288766,
1.163141288766,1.163141288766,1.163141288766,1.163141288766,1.163141288766,
1.163141288766,1.163141288766,1.163141288766,1.163141288766,1.163141288766,
1.163141288766,1.163141288766)))
REPRESENTATION_ITEM('')
SURFACE()
);
#192=(
BOUNDED_SURFACE()
B_SPLINE_SURFACE(3,3,((#45441,#45442,#45443,#45444,#45445,#45446,#45447,
#45448,#45449,#45450,#45451,#45452,#45453,#45454,#45455,#45456,#45457,#45458),
(#45459,#45460,#45461,#45462,#45463,#45464,#45465,#45466,#45467,#45468,
#45469,#45470,#45471,#45472,#45473,#45474,#45475,#45476),(#45477,#45478,
#45479,#45480,#45481,#45482,#45483,#45484,#45485,#45486,#45487,#45488,#45489,
#45490,#45491,#45492,#45493,#45494),(#45495,#45496,#45497,#45498,#45499,
#45500,#45501,#45502,#45503,#45504,#45505,#45506,#45507,#45508,#45509,#45510,
#45511,#45512)),.UNSPECIFIED.,.F.,.F.,.F.)
B_SPLINE_SURFACE_WITH_KNOTS((4,4),(4,1,1,1,1,1,1,1,1,1,1,1,1,1,1,4),(0.,
1.),(-0.003641476161696,0.,0.03996584306645,0.07565969810702,0.107705792552,
0.1364673868443,0.1623976598809,0.1860106967015,0.2078779981353,0.2287055315989,
0.2494804366836,0.2705832190163,0.2914915459405,0.3122164361973,0.3338956761934,
0.3478416898621),.UNSPECIFIED.)
GEOMETRIC_REPRESENTATION_ITEM()
RATIONAL_B_SPLINE_SURFACE(((1.224501069917,1.224501069917,1.224501069917,
1.224501069917,1.224501069917,1.224501069917,1.224501069917,1.224501069917,
1.224501069917,1.224501069917,1.224501069917,1.224501069917,1.224501069917,
1.224501069917,1.224501069917,1.224501069917,1.224501069917,1.224501069917),
(0.9251663100277,0.9251663100277,0.9251663100277,0.9251663100277,0.9251663100277,
0.9251663100277,0.9251663100277,0.9251663100277,0.9251663100277,0.9251663100277,
0.9251663100277,0.9251663100277,0.9251663100277,0.9251663100277,0.9251663100277,
0.9251663100277,0.9251663100277,0.9251663100277),(0.9251663100277,0.9251663100277,
0.9251663100277,0.9251663100277,0.9251663100277,0.9251663100277,0.9251663100277,
0.9251663100277,0.9251663100277,0.9251663100277,0.9251663100277,0.9251663100277,
0.9251663100277,0.9251663100277,0.9251663100277,0.9251663100277,0.9251663100277,
0.9251663100277),(1.224501069917,1.224501069917,1.224501069917,1.224501069917,
1.224501069917,1.224501069917,1.224501069917,1.224501069917,1.224501069917,
1.224501069917,1.224501069917,1.224501069917,1.224501069917,1.224501069917,
1.224501069917,1.224501069917,1.224501069917,1.224501069917)))
REPRESENTATION_ITEM('')
SURFACE()
);
#193=(
BOUNDED_SURFACE()
B_SPLINE_SURFACE(3,3,((#45594,#45595,#45596,#45597,#45598,#45599,#45600,
#45601,#45602,#45603,#45604,#45605,#45606),(#45607,#45608,#45609,#45610,
#45611,#45612,#45613,#45614,#45615,#45616,#45617,#45618,#45619),(#45620,
#45621,#45622,#45623,#45624,#45625,#45626,#45627,#45628,#45629,#45630,#45631,
#45632),(#45633,#45634,#45635,#45636,#45637,#45638,#45639,#45640,#45641,
#45642,#45643,#45644,#45645)),.UNSPECIFIED.,.F.,.F.,.F.)
B_SPLINE_SURFACE_WITH_KNOTS((4,4),(4,1,1,1,1,1,1,1,1,1,4),(0.,1.),(-0.0103387915936,
0.,0.1251367424062,0.2492492298603,0.3735032958992,0.4979081598552,0.6224043335643,
0.7477267861541,0.8737422387189,1.,1.010148865997),.UNSPECIFIED.)
GEOMETRIC_REPRESENTATION_ITEM()
RATIONAL_B_SPLINE_SURFACE(((1.000215851129,1.000215851129,1.000215851129,
1.000215851129,1.000215851129,1.000215851129,1.000215851129,1.000215851129,
1.000215851129,1.000215851129,1.000215851129,1.000215851129,1.000215851129),
(0.9999280496237,0.9999280496237,0.9999280496237,0.9999280496237,0.9999280496237,
0.9999280496237,0.9999280496237,0.9999280496237,0.9999280496237,0.9999280496237,
0.9999280496237,0.9999280496237,0.9999280496237),(0.9999280496237,0.9999280496237,
0.9999280496237,0.9999280496237,0.9999280496237,0.9999280496237,0.9999280496237,
0.9999280496237,0.9999280496237,0.9999280496237,0.9999280496237,0.9999280496237,
0.9999280496237),(1.000215851129,1.000215851129,1.000215851129,1.000215851129,
1.000215851129,1.000215851129,1.000215851129,1.000215851129,1.000215851129,
1.000215851129,1.000215851129,1.000215851129,1.000215851129)))
REPRESENTATION_ITEM('')
SURFACE()
);
#194=(
BOUNDED_SURFACE()
B_SPLINE_SURFACE(3,3,((#45713,#45714,#45715,#45716,#45717,#45718,#45719,
#45720),(#45721,#45722,#45723,#45724,#45725,#45726,#45727,#45728),(#45729,
#45730,#45731,#45732,#45733,#45734,#45735,#45736),(#45737,#45738,#45739,
#45740,#45741,#45742,#45743,#45744)),.UNSPECIFIED.,.F.,.F.,.F.)
B_SPLINE_SURFACE_WITH_KNOTS((4,4),(4,1,1,1,1,4),(0.,1.),(-0.02002688240655,
0.,0.3332292460223,0.6664005931354,1.,1.020557756204),.UNSPECIFIED.)
GEOMETRIC_REPRESENTATION_ITEM()
RATIONAL_B_SPLINE_SURFACE(((1.00007870989,1.00007870989,1.00007870989,1.00007870989,
1.00007870989,1.00007870989,1.00007870989,1.00007870989),(0.9999737633701,
0.9999737633701,0.9999737633701,0.9999737633701,0.9999737633701,0.9999737633701,
0.9999737633701,0.9999737633701),(0.9999737633701,0.9999737633701,0.9999737633701,
0.9999737633701,0.9999737633701,0.9999737633701,0.9999737633701,0.9999737633701),
(1.00007870989,1.00007870989,1.00007870989,1.00007870989,1.00007870989,
1.00007870989,1.00007870989,1.00007870989)))
REPRESENTATION_ITEM('')
SURFACE()
);
#195=(
BOUNDED_SURFACE()
B_SPLINE_SURFACE(3,3,((#45748,#45749,#45750,#45751,#45752,#45753,#45754,
#45755,#45756,#45757,#45758,#45759,#45760,#45761,#45762,#45763,#45764,#45765,
#45766),(#45767,#45768,#45769,#45770,#45771,#45772,#45773,#45774,#45775,
#45776,#45777,#45778,#45779,#45780,#45781,#45782,#45783,#45784,#45785),
(#45786,#45787,#45788,#45789,#45790,#45791,#45792,#45793,#45794,#45795,
#45796,#45797,#45798,#45799,#45800,#45801,#45802,#45803,#45804),(#45805,
#45806,#45807,#45808,#45809,#45810,#45811,#45812,#45813,#45814,#45815,#45816,
#45817,#45818,#45819,#45820,#45821,#45822,#45823)),.UNSPECIFIED.,.F.,.F.,
 .F.)
B_SPLINE_SURFACE_WITH_KNOTS((4,4),(4,1,1,1,1,1,1,1,1,1,1,1,1,1,1,1,4),(0.,
1.),(-0.01435280055262,0.,0.1052237534203,0.2024514847669,0.2919074772468,
0.3731001338908,0.4462221459727,0.5125974112795,0.574182113677,0.6331082197362,
0.6912681104287,0.7496322505172,0.8078577516813,0.8672149095682,0.9304407269683,
1.,1.014830854834),.UNSPECIFIED.)
GEOMETRIC_REPRESENTATION_ITEM()
RATIONAL_B_SPLINE_SURFACE(((1.087955100757,1.087955100757,1.087955100757,
1.087955100757,1.087955100757,1.087955100757,1.087955100757,1.087955100757,
1.087955100757,1.087955100757,1.087955100757,1.087955100757,1.087955100757,
1.087955100757,1.087955100757,1.087955100757,1.087955100757,1.087955100757,
1.087955100757),(0.970681633081,0.970681633081,0.970681633081,0.970681633081,
0.970681633081,0.970681633081,0.970681633081,0.970681633081,0.970681633081,
0.970681633081,0.970681633081,0.970681633081,0.970681633081,0.970681633081,
0.970681633081,0.970681633081,0.970681633081,0.970681633081,0.970681633081),
(0.970681633081,0.970681633081,0.970681633081,0.970681633081,0.970681633081,
0.970681633081,0.970681633081,0.970681633081,0.970681633081,0.970681633081,
0.970681633081,0.970681633081,0.970681633081,0.970681633081,0.970681633081,
0.970681633081,0.970681633081,0.970681633081,0.970681633081),(1.087955100757,
1.087955100757,1.087955100757,1.087955100757,1.087955100757,1.087955100757,
1.087955100757,1.087955100757,1.087955100757,1.087955100757,1.087955100757,
1.087955100757,1.087955100757,1.087955100757,1.087955100757,1.087955100757,
1.087955100757,1.087955100757,1.087955100757)))
REPRESENTATION_ITEM('')
SURFACE()
);
#196=(
BOUNDED_SURFACE()
B_SPLINE_SURFACE(3,3,((#45942,#45943,#45944,#45945,#45946,#45947,#45948,
#45949,#45950,#45951),(#45952,#45953,#45954,#45955,#45956,#45957,#45958,
#45959,#45960,#45961),(#45962,#45963,#45964,#45965,#45966,#45967,#45968,
#45969,#45970,#45971),(#45972,#45973,#45974,#45975,#45976,#45977,#45978,
#45979,#45980,#45981)),.UNSPECIFIED.,.F.,.F.,.F.)
B_SPLINE_SURFACE_WITH_KNOTS((4,4),(4,1,1,1,1,1,1,4),(0.,1.),(-0.01569017456562,
0.,0.1634721590841,0.348317956625,0.5531428960446,0.7725802144006,1.,1.008112438365),
 .UNSPECIFIED.)
GEOMETRIC_REPRESENTATION_ITEM()
RATIONAL_B_SPLINE_SURFACE(((1.059581909356,1.059581909356,1.059581909356,
1.059581909356,1.059581909356,1.059581909356,1.059581909356,1.059581909356,
1.059581909356,1.059581909356),(0.9801393635479,0.9801393635479,0.9801393635479,
0.9801393635479,0.9801393635479,0.9801393635479,0.9801393635479,0.9801393635479,
0.9801393635479,0.9801393635479),(0.9801393635479,0.9801393635479,0.9801393635479,
0.9801393635479,0.9801393635479,0.9801393635479,0.9801393635479,0.9801393635479,
0.9801393635479,0.9801393635479),(1.059581909356,1.059581909356,1.059581909356,
1.059581909356,1.059581909356,1.059581909356,1.059581909356,1.059581909356,
1.059581909356,1.059581909356)))
REPRESENTATION_ITEM('')
SURFACE()
);
#197=(
BOUNDED_SURFACE()
B_SPLINE_SURFACE(3,3,((#45982,#45983,#45984,#45985,#45986,#45987,#45988,
#45989,#45990,#45991),(#45992,#45993,#45994,#45995,#45996,#45997,#45998,
#45999,#46000,#46001),(#46002,#46003,#46004,#46005,#46006,#46007,#46008,
#46009,#46010,#46011),(#46012,#46013,#46014,#46015,#46016,#46017,#46018,
#46019,#46020,#46021)),.UNSPECIFIED.,.F.,.F.,.F.)
B_SPLINE_SURFACE_WITH_KNOTS((4,4),(4,1,1,1,1,1,1,4),(0.,1.),(-0.1276752045009,
0.,0.177977214136,0.3579508099613,0.5526671794136,0.7657440822575,1.,1.101553192821),
 .UNSPECIFIED.)
GEOMETRIC_REPRESENTATION_ITEM()
RATIONAL_B_SPLINE_SURFACE(((1.12652088875,1.12652088875,1.12652088875,1.12652088875,
1.12652088875,1.12652088875,1.12652088875,1.12652088875,1.12652088875,1.12652088875),
(0.9578263704167,0.9578263704167,0.9578263704167,0.9578263704167,0.9578263704167,
0.9578263704167,0.9578263704167,0.9578263704167,0.9578263704167,0.9578263704167),
(0.9578263704167,0.9578263704167,0.9578263704167,0.9578263704167,0.9578263704167,
0.9578263704167,0.9578263704167,0.9578263704167,0.9578263704167,0.9578263704167),
(1.12652088875,1.12652088875,1.12652088875,1.12652088875,1.12652088875,
1.12652088875,1.12652088875,1.12652088875,1.12652088875,1.12652088875)))
REPRESENTATION_ITEM('')
SURFACE()
);
#198=(
BOUNDED_SURFACE()
B_SPLINE_SURFACE(2,2,((#46210,#46211,#46212,#46213,#46214,#46215,#46216,
#46217,#46218),(#46219,#46220,#46221,#46222,#46223,#46224,#46225,#46226,
#46227),(#46228,#46229,#46230,#46231,#46232,#46233,#46234,#46235,#46236)),
 .UNSPECIFIED.,.F.,.T.,.F.)
B_SPLINE_SURFACE_WITH_KNOTS((3,3),(3,2,2,2,3),(-1.57079632679222,-1.09244241804695),
(-3.14159265358979,-1.5707963267949,0.,1.5707963267949,3.14159265358979),
 .UNSPECIFIED.)
GEOMETRIC_REPRESENTATION_ITEM()
RATIONAL_B_SPLINE_SURFACE(((1.,0.707106781186548,1.,0.707106781186548,1.,
0.707106781186548,1.,0.707106781186548,1.),(0.971533285943088,0.686977774638807,
0.971533285943088,0.686977774638807,0.971533285943088,0.686977774638807,
0.971533285943088,0.686977774638807,0.971533285943088),(1.,0.707106781186548,
1.,0.707106781186548,1.,0.707106781186548,1.,0.707106781186548,1.)))
REPRESENTATION_ITEM('')
SURFACE()
);
#199=CONICAL_SURFACE('',#9705,1.393148400081,0.349065850398866);
#200=CONICAL_SURFACE('',#9711,1.308493649054,1.0471975511966);
#201=CONICAL_SURFACE('',#9717,1.393148400081,0.349065850398866);
#202=CONICAL_SURFACE('',#9881,49.77255842762,0.0349065850398866);
#203=CONICAL_SURFACE('',#9886,49.77255839012,0.0349065850398866);
#204=CONICAL_SURFACE('',#9904,1.925,0.785398163397448);
#205=CONICAL_SURFACE('',#9938,1.725,0.785398163397448);
#206=CONICAL_SURFACE('',#9944,1.175,0.785398163397448);
#207=TOROIDAL_SURFACE('',#9675,6.705,4.705);
#208=TOROIDAL_SURFACE('',#9702,3.2,0.25);
#209=TOROIDAL_SURFACE('',#9712,1.707288968431,0.4);
#210=TOROIDAL_SURFACE('',#9799,4.3,0.5);
#211=TOROIDAL_SURFACE('',#9804,49.4822348431,0.5);
#212=TOROIDAL_SURFACE('',#9832,49.4822348431,0.5);
#213=TOROIDAL_SURFACE('',#9848,49.4822348431,0.5);
#214=TOROIDAL_SURFACE('',#9853,4.3,0.5);
#215=TOROIDAL_SURFACE('',#9863,4.3,0.5);
#216=TOROIDAL_SURFACE('',#9865,3.3,0.5);
#217=TOROIDAL_SURFACE('',#9869,4.3,0.5);
#218=TOROIDAL_SURFACE('',#9879,49.4822348431,0.5);
#219=TOROIDAL_SURFACE('',#9940,1.594974746831,0.7);
#220=TOROIDAL_SURFACE('',#9991,6.,1.);
#221=TOROIDAL_SURFACE('',#10030,9.,1.);
#222=TOROIDAL_SURFACE('',#10036,1.5,0.5);
#223=TOROIDAL_SURFACE('',#10044,2.5,0.5);
#224=TOROIDAL_SURFACE('',#10048,2.5,0.5);
#225=TOROIDAL_SURFACE('',#10055,1.5,0.5);
#226=TOROIDAL_SURFACE('',#10057,7.5,0.5);
#227=TOROIDAL_SURFACE('',#10063,7.5,0.5);
#228=TOROIDAL_SURFACE('',#10121,2.5,0.5);
#229=TOROIDAL_SURFACE('',#10126,7.5,0.5);
#230=TOROIDAL_SURFACE('',#10140,6.2,0.8);
#231=TOROIDAL_SURFACE('',#10172,3.35,0.75);
#232=SHAPE_REPRESENTATION_RELATIONSHIP('SRR','None',#52211,#245);
#233=SHAPE_REPRESENTATION_RELATIONSHIP('SRR','None',#52212,#246);
#234=SHAPE_REPRESENTATION_RELATIONSHIP('SRR','None',#52213,#247);
#235=SHAPE_REPRESENTATION_RELATIONSHIP('SRR','None',#52214,#248);
#236=SHAPE_REPRESENTATION_RELATIONSHIP('SRR','None',#52215,#249);
#237=SHAPE_REPRESENTATION_RELATIONSHIP('SRR','None',#52216,#250);
#238=SHAPE_REPRESENTATION_RELATIONSHIP('SRR','None',#52217,#251);
#239=SHAPE_REPRESENTATION_RELATIONSHIP('SRR','None',#52218,#252);
#240=SHAPE_REPRESENTATION_RELATIONSHIP('SRR','None',#52219,#253);
#241=SHAPE_REPRESENTATION_RELATIONSHIP('SRR','None',#52220,#254);
#242=SHAPE_REPRESENTATION_RELATIONSHIP('SRR','None',#52221,#255);
#243=SHAPE_REPRESENTATION_RELATIONSHIP('SRR','None',#52222,#256);
#244=SHAPE_REPRESENTATION_RELATIONSHIP('SRR','None',#52223,#257);
#245=ADVANCED_BREP_SHAPE_REPRESENTATION('',(#271),#52151);
#246=ADVANCED_BREP_SHAPE_REPRESENTATION('',(#272),#52152);
#247=ADVANCED_BREP_SHAPE_REPRESENTATION('',(#273),#52153);
#248=ADVANCED_BREP_SHAPE_REPRESENTATION('',(#274),#52154);
#249=ADVANCED_BREP_SHAPE_REPRESENTATION('',(#275),#52155);
#250=ADVANCED_BREP_SHAPE_REPRESENTATION('',(#276),#52156);
#251=ADVANCED_BREP_SHAPE_REPRESENTATION('',(#277),#52157);
#252=ADVANCED_BREP_SHAPE_REPRESENTATION('',(#278),#52158);
#253=ADVANCED_BREP_SHAPE_REPRESENTATION('',(#279),#52159);
#254=ADVANCED_BREP_SHAPE_REPRESENTATION('',(#280),#52160);
#255=ADVANCED_BREP_SHAPE_REPRESENTATION('',(#281),#52161);
#256=ADVANCED_BREP_SHAPE_REPRESENTATION('',(#282),#52162);
#257=ADVANCED_BREP_SHAPE_REPRESENTATION('',(#283),#52163);
#258=STYLED_ITEM('',(#52318),#271);
#259=STYLED_ITEM('',(#52311),#272);
#260=STYLED_ITEM('',(#52318),#273);
#261=STYLED_ITEM('',(#52325),#274);
#262=STYLED_ITEM('',(#52325),#275);
#263=STYLED_ITEM('',(#52318),#276);
#264=STYLED_ITEM('',(#52325),#277);
#265=STYLED_ITEM('',(#52297),#278);
#266=STYLED_ITEM('',(#52325),#279);
#267=STYLED_ITEM('',(#52318),#280);
#268=STYLED_ITEM('',(#52325),#281);
#269=STYLED_ITEM('',(#52325),#282);
#270=STYLED_ITEM('',(#52332),#283);
#271=MANIFOLD_SOLID_BREP('Body1',#9118);
#272=MANIFOLD_SOLID_BREP('Body1',#9119);
#273=MANIFOLD_SOLID_BREP('Body1',#9120);
#274=MANIFOLD_SOLID_BREP('Body1',#9121);
#275=MANIFOLD_SOLID_BREP('Body1',#9122);
#276=MANIFOLD_SOLID_BREP('Body1',#9123);
#277=MANIFOLD_SOLID_BREP('Body1',#9124);
#278=MANIFOLD_SOLID_BREP('Body1',#9125);
#279=MANIFOLD_SOLID_BREP('Body1',#9126);
#280=MANIFOLD_SOLID_BREP('Body1',#9127);
#281=MANIFOLD_SOLID_BREP('Body1',#9128);
#282=MANIFOLD_SOLID_BREP('Body1',#9129);
#283=MANIFOLD_SOLID_BREP('Body1',#9130);
#284=SPHERICAL_SURFACE('',#9300,12.5);
#285=SPHERICAL_SURFACE('',#9677,5.);
#286=SPHERICAL_SURFACE('',#10190,50.);
#287=SPHERICAL_SURFACE('',#10195,49.5);
#288=FACE_BOUND('',#1072,.T.);
#289=FACE_BOUND('',#1091,.T.);
#290=FACE_BOUND('',#1095,.T.);
#291=FACE_BOUND('',#1103,.T.);
#292=FACE_BOUND('',#1106,.T.);
#293=FACE_BOUND('',#1236,.T.);
#294=FACE_BOUND('',#1240,.T.);
#295=FACE_BOUND('',#1241,.T.);
#296=FACE_BOUND('',#1251,.T.);
#297=FACE_BOUND('',#1273,.T.);
#298=FACE_BOUND('',#1276,.T.);
#299=FACE_BOUND('',#1298,.T.);
#300=FACE_BOUND('',#1400,.T.);
#301=FACE_BOUND('',#1406,.T.);
#302=FACE_BOUND('',#1409,.T.);
#303=FACE_BOUND('',#1425,.T.);
#304=FACE_BOUND('',#1477,.T.);
#305=FACE_BOUND('',#1481,.T.);
#306=FACE_BOUND('',#1499,.T.);
#307=FACE_BOUND('',#1501,.T.);
#308=FACE_BOUND('',#1503,.T.);
#309=FACE_BOUND('',#1506,.T.);
#310=FACE_BOUND('',#1507,.T.);
#311=FACE_BOUND('',#1510,.T.);
#312=FACE_BOUND('',#1545,.T.);
#313=FACE_BOUND('',#1548,.T.);
#314=FACE_BOUND('',#1551,.T.);
#315=FACE_BOUND('',#1578,.T.);
#316=FACE_BOUND('',#1581,.T.);
#317=FACE_BOUND('',#1584,.T.);
#318=FACE_BOUND('',#1587,.T.);
#319=FACE_BOUND('',#1591,.T.);
#320=FACE_BOUND('',#1616,.T.);
#321=FACE_BOUND('',#1619,.T.);
#322=FACE_BOUND('',#1622,.T.);
#323=B_SPLINE_SURFACE_WITH_KNOTS('',3,3,((#13144,#13145,#13146,#13147,#13148,
#13149,#13150,#13151,#13152,#13153,#13154,#13155,#13156,#13157,#13158,#13159,
#13160,#13161,#13162,#13163,#13164,#13165,#13166,#13167,#13168,#13169,#13170,
#13171,#13172,#13173,#13174,#13175,#13176,#13177,#13178),(#13179,#13180,
#13181,#13182,#13183,#13184,#13185,#13186,#13187,#13188,#13189,#13190,#13191,
#13192,#13193,#13194,#13195,#13196,#13197,#13198,#13199,#13200,#13201,#13202,
#13203,#13204,#13205,#13206,#13207,#13208,#13209,#13210,#13211,#13212,#13213),
(#13214,#13215,#13216,#13217,#13218,#13219,#13220,#13221,#13222,#13223,
#13224,#13225,#13226,#13227,#13228,#13229,#13230,#13231,#13232,#13233,#13234,
#13235,#13236,#13237,#13238,#13239,#13240,#13241,#13242,#13243,#13244,#13245,
#13246,#13247,#13248),(#13249,#13250,#13251,#13252,#13253,#13254,#13255,
#13256,#13257,#13258,#13259,#13260,#13261,#13262,#13263,#13264,#13265,#13266,
#13267,#13268,#13269,#13270,#13271,#13272,#13273,#13274,#13275,#13276,#13277,
#13278,#13279,#13280,#13281,#13282,#13283)),.UNSPECIFIED.,.F.,.F.,.F.,(4,
4),(4,1,1,1,1,1,1,1,1,1,1,1,1,1,1,1,1,1,1,1,1,1,1,1,1,1,1,1,1,1,1,1,4),
(0.3338579451982,1.029778418438),(-0.02,0.0125,0.045,0.0775,0.11,0.1425,
0.175,0.2075,0.24,0.2725,0.305,0.3375,0.37,0.4025,0.435,0.4675,0.5,0.5325,
0.565,0.5975,0.63,0.6625,0.695,0.7275,0.76,0.7925,0.825,0.8575,0.89,0.9225,
0.955,0.9875,1.02),.UNSPECIFIED.);
#324=B_SPLINE_SURFACE_WITH_KNOTS('',3,3,((#13372,#13373,#13374,#13375,#13376,
#13377,#13378,#13379,#13380,#13381,#13382,#13383,#13384,#13385,#13386,#13387,
#13388,#13389,#13390,#13391,#13392,#13393,#13394,#13395,#13396,#13397,#13398,
#13399,#13400,#13401,#13402,#13403,#13404,#13405,#13406),(#13407,#13408,
#13409,#13410,#13411,#13412,#13413,#13414,#13415,#13416,#13417,#13418,#13419,
#13420,#13421,#13422,#13423,#13424,#13425,#13426,#13427,#13428,#13429,#13430,
#13431,#13432,#13433,#13434,#13435,#13436,#13437,#13438,#13439,#13440,#13441),
(#13442,#13443,#13444,#13445,#13446,#13447,#13448,#13449,#13450,#13451,
#13452,#13453,#13454,#13455,#13456,#13457,#13458,#13459,#13460,#13461,#13462,
#13463,#13464,#13465,#13466,#13467,#13468,#13469,#13470,#13471,#13472,#13473,
#13474,#13475,#13476),(#13477,#13478,#13479,#13480,#13481,#13482,#13483,
#13484,#13485,#13486,#13487,#13488,#13489,#13490,#13491,#13492,#13493,#13494,
#13495,#13496,#13497,#13498,#13499,#13500,#13501,#13502,#13503,#13504,#13505,
#13506,#13507,#13508,#13509,#13510,#13511)),.UNSPECIFIED.,.F.,.F.,.F.,(4,
4),(4,1,1,1,1,1,1,1,1,1,1,1,1,1,1,1,1,1,1,1,1,1,1,1,1,1,1,1,1,1,1,1,4),
(0.3338579451982,1.029778418438),(-0.02,0.0125,0.045,0.0775,0.11,0.1425,
0.175,0.2075,0.24,0.2725,0.305,0.3375,0.37,0.4025,0.435,0.4675,0.5,0.5325,
0.565,0.5975,0.63,0.6625,0.695,0.7275,0.76,0.7925,0.825,0.8575,0.89,0.9225,
0.955,0.9875,1.02),.UNSPECIFIED.);
#325=B_SPLINE_SURFACE_WITH_KNOTS('',3,3,((#13626,#13627,#13628,#13629,#13630,
#13631,#13632,#13633,#13634,#13635,#13636,#13637,#13638,#13639,#13640,#13641,
#13642,#13643,#13644,#13645,#13646,#13647,#13648,#13649,#13650,#13651,#13652,
#13653,#13654,#13655,#13656,#13657,#13658,#13659,#13660),(#13661,#13662,
#13663,#13664,#13665,#13666,#13667,#13668,#13669,#13670,#13671,#13672,#13673,
#13674,#13675,#13676,#13677,#13678,#13679,#13680,#13681,#13682,#13683,#13684,
#13685,#13686,#13687,#13688,#13689,#13690,#13691,#13692,#13693,#13694,#13695),
(#13696,#13697,#13698,#13699,#13700,#13701,#13702,#13703,#13704,#13705,
#13706,#13707,#13708,#13709,#13710,#13711,#13712,#13713,#13714,#13715,#13716,
#13717,#13718,#13719,#13720,#13721,#13722,#13723,#13724,#13725,#13726,#13727,
#13728,#13729,#13730),(#13731,#13732,#13733,#13734,#13735,#13736,#13737,
#13738,#13739,#13740,#13741,#13742,#13743,#13744,#13745,#13746,#13747,#13748,
#13749,#13750,#13751,#13752,#13753,#13754,#13755,#13756,#13757,#13758,#13759,
#13760,#13761,#13762,#13763,#13764,#13765)),.UNSPECIFIED.,.F.,.F.,.F.,(4,
4),(4,1,1,1,1,1,1,1,1,1,1,1,1,1,1,1,1,1,1,1,1,1,1,1,1,1,1,1,1,1,1,1,4),
(-0.02977841843818,0.6661420548018),(-0.02,0.0125,0.045,0.0775,0.11,0.1425,
0.175,0.2075,0.24,0.2725,0.305,0.3375,0.37,0.4025,0.435,0.4675,0.5,0.5325,
0.565,0.5975,0.63,0.6625,0.695,0.7275,0.76,0.7925,0.825,0.8575,0.89,0.9225,
0.955,0.9875,1.02),.UNSPECIFIED.);
#326=B_SPLINE_SURFACE_WITH_KNOTS('',3,3,((#13854,#13855,#13856,#13857,#13858,
#13859,#13860,#13861,#13862,#13863,#13864,#13865,#13866,#13867,#13868,#13869,
#13870,#13871,#13872,#13873,#13874,#13875,#13876,#13877,#13878,#13879,#13880,
#13881,#13882,#13883,#13884,#13885,#13886,#13887,#13888),(#13889,#13890,
#13891,#13892,#13893,#13894,#13895,#13896,#13897,#13898,#13899,#13900,#13901,
#13902,#13903,#13904,#13905,#13906,#13907,#13908,#13909,#13910,#13911,#13912,
#13913,#13914,#13915,#13916,#13917,#13918,#13919,#13920,#13921,#13922,#13923),
(#13924,#13925,#13926,#13927,#13928,#13929,#13930,#13931,#13932,#13933,
#13934,#13935,#13936,#13937,#13938,#13939,#13940,#13941,#13942,#13943,#13944,
#13945,#13946,#13947,#13948,#13949,#13950,#13951,#13952,#13953,#13954,#13955,
#13956,#13957,#13958),(#13959,#13960,#13961,#13962,#13963,#13964,#13965,
#13966,#13967,#13968,#13969,#13970,#13971,#13972,#13973,#13974,#13975,#13976,
#13977,#13978,#13979,#13980,#13981,#13982,#13983,#13984,#13985,#13986,#13987,
#13988,#13989,#13990,#13991,#13992,#13993)),.UNSPECIFIED.,.F.,.F.,.F.,(4,
4),(4,1,1,1,1,1,1,1,1,1,1,1,1,1,1,1,1,1,1,1,1,1,1,1,1,1,1,1,1,1,1,1,4),
(-0.02977841843818,0.6661420548018),(-0.02,0.0125,0.045,0.0775,0.11,0.1425,
0.175,0.2075,0.24,0.2725,0.305,0.3375,0.37,0.4025,0.435,0.4675,0.5,0.5325,
0.565,0.5975,0.63,0.6625,0.695,0.7275,0.76,0.7925,0.825,0.8575,0.89,0.9225,
0.955,0.9875,1.02),.UNSPECIFIED.);
#327=B_SPLINE_SURFACE_WITH_KNOTS('',3,3,((#14080,#14081,#14082,#14083,#14084,
#14085,#14086,#14087,#14088,#14089,#14090,#14091,#14092,#14093,#14094,#14095,
#14096,#14097,#14098,#14099,#14100,#14101,#14102,#14103,#14104,#14105,#14106,
#14107,#14108,#14109,#14110,#14111,#14112,#14113,#14114),(#14115,#14116,
#14117,#14118,#14119,#14120,#14121,#14122,#14123,#14124,#14125,#14126,#14127,
#14128,#14129,#14130,#14131,#14132,#14133,#14134,#14135,#14136,#14137,#14138,
#14139,#14140,#14141,#14142,#14143,#14144,#14145,#14146,#14147,#14148,#14149),
(#14150,#14151,#14152,#14153,#14154,#14155,#14156,#14157,#14158,#14159,
#14160,#14161,#14162,#14163,#14164,#14165,#14166,#14167,#14168,#14169,#14170,
#14171,#14172,#14173,#14174,#14175,#14176,#14177,#14178,#14179,#14180,#14181,
#14182,#14183,#14184),(#14185,#14186,#14187,#14188,#14189,#14190,#14191,
#14192,#14193,#14194,#14195,#14196,#14197,#14198,#14199,#14200,#14201,#14202,
#14203,#14204,#14205,#14206,#14207,#14208,#14209,#14210,#14211,#14212,#14213,
#14214,#14215,#14216,#14217,#14218,#14219)),.UNSPECIFIED.,.F.,.F.,.F.,(4,
4),(4,1,1,1,1,1,1,1,1,1,1,1,1,1,1,1,1,1,1,1,1,1,1,1,1,1,1,1,1,1,1,1,4),
(-0.1795055630679,1.179505563068),(-0.02,0.0125,0.045,0.0775,0.11,0.1425,
0.175,0.2075,0.24,0.2725,0.305,0.3375,0.37,0.4025,0.435,0.4675,0.5,0.5325,
0.565,0.5975,0.63,0.6625,0.695,0.7275,0.76,0.7925,0.825,0.8575,0.89,0.9225,
0.955,0.9875,1.02),.UNSPECIFIED.);
#328=B_SPLINE_SURFACE_WITH_KNOTS('',3,3,((#14625,#14626,#14627,#14628,#14629,
#14630,#14631,#14632,#14633,#14634,#14635,#14636,#14637,#14638,#14639,#14640,
#14641,#14642,#14643,#14644,#14645,#14646,#14647,#14648,#14649,#14650,#14651,
#14652,#14653,#14654,#14655,#14656,#14657,#14658,#14659),(#14660,#14661,
#14662,#14663,#14664,#14665,#14666,#14667,#14668,#14669,#14670,#14671,#14672,
#14673,#14674,#14675,#14676,#14677,#14678,#14679,#14680,#14681,#14682,#14683,
#14684,#14685,#14686,#14687,#14688,#14689,#14690,#14691,#14692,#14693,#14694),
(#14695,#14696,#14697,#14698,#14699,#14700,#14701,#14702,#14703,#14704,
#14705,#14706,#14707,#14708,#14709,#14710,#14711,#14712,#14713,#14714,#14715,
#14716,#14717,#14718,#14719,#14720,#14721,#14722,#14723,#14724,#14725,#14726,
#14727,#14728,#14729),(#14730,#14731,#14732,#14733,#14734,#14735,#14736,
#14737,#14738,#14739,#14740,#14741,#14742,#14743,#14744,#14745,#14746,#14747,
#14748,#14749,#14750,#14751,#14752,#14753,#14754,#14755,#14756,#14757,#14758,
#14759,#14760,#14761,#14762,#14763,#14764)),.UNSPECIFIED.,.F.,.F.,.F.,(4,
4),(4,1,1,1,1,1,1,1,1,1,1,1,1,1,1,1,1,1,1,1,1,1,1,1,1,1,1,1,1,1,1,1,4),
(-0.1795055630679,1.179505563068),(-0.02,0.0125,0.045,0.0775,0.11,0.1425,
0.175,0.2075,0.24,0.2725,0.305,0.3375,0.37,0.4025,0.435,0.4675,0.5,0.5325,
0.565,0.5975,0.63,0.6625,0.695,0.7275,0.76,0.7925,0.825,0.8575,0.89,0.9225,
0.955,0.9875,1.02),.UNSPECIFIED.);
#329=B_SPLINE_SURFACE_WITH_KNOTS('',3,3,((#14766,#14767,#14768,#14769,#14770,
#14771,#14772,#14773,#14774,#14775,#14776,#14777,#14778,#14779,#14780,#14781,
#14782,#14783,#14784,#14785,#14786,#14787,#14788,#14789,#14790,#14791,#14792,
#14793,#14794,#14795,#14796,#14797,#14798,#14799,#14800),(#14801,#14802,
#14803,#14804,#14805,#14806,#14807,#14808,#14809,#14810,#14811,#14812,#14813,
#14814,#14815,#14816,#14817,#14818,#14819,#14820,#14821,#14822,#14823,#14824,
#14825,#14826,#14827,#14828,#14829,#14830,#14831,#14832,#14833,#14834,#14835),
(#14836,#14837,#14838,#14839,#14840,#14841,#14842,#14843,#14844,#14845,
#14846,#14847,#14848,#14849,#14850,#14851,#14852,#14853,#14854,#14855,#14856,
#14857,#14858,#14859,#14860,#14861,#14862,#14863,#14864,#14865,#14866,#14867,
#14868,#14869,#14870),(#14871,#14872,#14873,#14874,#14875,#14876,#14877,
#14878,#14879,#14880,#14881,#14882,#14883,#14884,#14885,#14886,#14887,#14888,
#14889,#14890,#14891,#14892,#14893,#14894,#14895,#14896,#14897,#14898,#14899,
#14900,#14901,#14902,#14903,#14904,#14905)),.UNSPECIFIED.,.F.,.F.,.F.,(4,
4),(4,1,1,1,1,1,1,1,1,1,1,1,1,1,1,1,1,1,1,1,1,1,1,1,1,1,1,1,1,1,1,1,4),
(-0.1795055630679,1.179505563068),(-0.02,0.0125,0.045,0.0775,0.11,0.1425,
0.175,0.2075,0.24,0.2725,0.305,0.3375,0.37,0.4025,0.435,0.4675,0.5,0.5325,
0.565,0.5975,0.63,0.6625,0.695,0.7275,0.76,0.7925,0.825,0.8575,0.89,0.9225,
0.955,0.9875,1.02),.UNSPECIFIED.);
#330=B_SPLINE_SURFACE_WITH_KNOTS('',3,3,((#15309,#15310,#15311,#15312,#15313,
#15314,#15315,#15316,#15317,#15318,#15319,#15320,#15321,#15322,#15323,#15324,
#15325,#15326,#15327,#15328,#15329,#15330,#15331,#15332,#15333,#15334,#15335,
#15336,#15337,#15338,#15339,#15340,#15341,#15342,#15343),(#15344,#15345,
#15346,#15347,#15348,#15349,#15350,#15351,#15352,#15353,#15354,#15355,#15356,
#15357,#15358,#15359,#15360,#15361,#15362,#15363,#15364,#15365,#15366,#15367,
#15368,#15369,#15370,#15371,#15372,#15373,#15374,#15375,#15376,#15377,#15378),
(#15379,#15380,#15381,#15382,#15383,#15384,#15385,#15386,#15387,#15388,
#15389,#15390,#15391,#15392,#15393,#15394,#15395,#15396,#15397,#15398,#15399,
#15400,#15401,#15402,#15403,#15404,#15405,#15406,#15407,#15408,#15409,#15410,
#15411,#15412,#15413),(#15414,#15415,#15416,#15417,#15418,#15419,#15420,
#15421,#15422,#15423,#15424,#15425,#15426,#15427,#15428,#15429,#15430,#15431,
#15432,#15433,#15434,#15435,#15436,#15437,#15438,#15439,#15440,#15441,#15442,
#15443,#15444,#15445,#15446,#15447,#15448)),.UNSPECIFIED.,.F.,.F.,.F.,(4,
4),(4,1,1,1,1,1,1,1,1,1,1,1,1,1,1,1,1,1,1,1,1,1,1,1,1,1,1,1,1,1,1,1,4),
(-0.1795055630679,1.179505563068),(-0.02,0.0125,0.045,0.0775,0.11,0.1425,
0.175,0.2075,0.24,0.2725,0.305,0.3375,0.37,0.4025,0.435,0.4675,0.5,0.5325,
0.565,0.5975,0.63,0.6625,0.695,0.7275,0.76,0.7925,0.825,0.8575,0.89,0.9225,
0.955,0.9875,1.02),.UNSPECIFIED.);
#331=B_SPLINE_SURFACE_WITH_KNOTS('',3,3,((#15538,#15539,#15540,#15541,#15542,
#15543,#15544,#15545,#15546,#15547,#15548,#15549,#15550,#15551,#15552,#15553,
#15554,#15555,#15556,#15557,#15558,#15559,#15560,#15561,#15562,#15563,#15564,
#15565,#15566,#15567,#15568,#15569,#15570,#15571,#15572),(#15573,#15574,
#15575,#15576,#15577,#15578,#15579,#15580,#15581,#15582,#15583,#15584,#15585,
#15586,#15587,#15588,#15589,#15590,#15591,#15592,#15593,#15594,#15595,#15596,
#15597,#15598,#15599,#15600,#15601,#15602,#15603,#15604,#15605,#15606,#15607),
(#15608,#15609,#15610,#15611,#15612,#15613,#15614,#15615,#15616,#15617,
#15618,#15619,#15620,#15621,#15622,#15623,#15624,#15625,#15626,#15627,#15628,
#15629,#15630,#15631,#15632,#15633,#15634,#15635,#15636,#15637,#15638,#15639,
#15640,#15641,#15642),(#15643,#15644,#15645,#15646,#15647,#15648,#15649,
#15650,#15651,#15652,#15653,#15654,#15655,#15656,#15657,#15658,#15659,#15660,
#15661,#15662,#15663,#15664,#15665,#15666,#15667,#15668,#15669,#15670,#15671,
#15672,#15673,#15674,#15675,#15676,#15677)),.UNSPECIFIED.,.F.,.F.,.F.,(4,
4),(4,1,1,1,1,1,1,1,1,1,1,1,1,1,1,1,1,1,1,1,1,1,1,1,1,1,1,1,1,1,1,1,4),
(-0.1560934940397,1.15609349404),(-0.02,0.0125,0.045,0.0775,0.11,0.1425,
0.175,0.2075,0.24,0.2725,0.305,0.3375,0.37,0.4025,0.435,0.4675,0.5,0.5325,
0.565,0.5975,0.63,0.6625,0.695,0.7275,0.76,0.7925,0.825,0.8575,0.89,0.9225,
0.955,0.9875,1.02),.UNSPECIFIED.);
#332=B_SPLINE_SURFACE_WITH_KNOTS('',3,3,((#15921,#15922,#15923,#15924,#15925,
#15926,#15927,#15928,#15929,#15930,#15931,#15932,#15933,#15934,#15935,#15936,
#15937,#15938,#15939,#15940,#15941,#15942,#15943,#15944,#15945,#15946,#15947,
#15948,#15949,#15950,#15951,#15952,#15953,#15954,#15955),(#15956,#15957,
#15958,#15959,#15960,#15961,#15962,#15963,#15964,#15965,#15966,#15967,#15968,
#15969,#15970,#15971,#15972,#15973,#15974,#15975,#15976,#15977,#15978,#15979,
#15980,#15981,#15982,#15983,#15984,#15985,#15986,#15987,#15988,#15989,#15990),
(#15991,#15992,#15993,#15994,#15995,#15996,#15997,#15998,#15999,#16000,
#16001,#16002,#16003,#16004,#16005,#16006,#16007,#16008,#16009,#16010,#16011,
#16012,#16013,#16014,#16015,#16016,#16017,#16018,#16019,#16020,#16021,#16022,
#16023,#16024,#16025),(#16026,#16027,#16028,#16029,#16030,#16031,#16032,
#16033,#16034,#16035,#16036,#16037,#16038,#16039,#16040,#16041,#16042,#16043,
#16044,#16045,#16046,#16047,#16048,#16049,#16050,#16051,#16052,#16053,#16054,
#16055,#16056,#16057,#16058,#16059,#16060)),.UNSPECIFIED.,.F.,.F.,.F.,(4,
4),(4,1,1,1,1,1,1,1,1,1,1,1,1,1,1,1,1,1,1,1,1,1,1,1,1,1,1,1,1,1,1,1,4),
(-0.1560934940397,1.15609349404),(-0.02,0.0125,0.045,0.0775,0.11,0.1425,
0.175,0.2075,0.24,0.2725,0.305,0.3375,0.37,0.4025,0.435,0.4675,0.5,0.5325,
0.565,0.5975,0.63,0.6625,0.695,0.7275,0.76,0.7925,0.825,0.8575,0.89,0.9225,
0.955,0.9875,1.02),.UNSPECIFIED.);
#333=B_SPLINE_SURFACE_WITH_KNOTS('',3,3,((#16228,#16229,#16230,#16231,#16232,
#16233,#16234,#16235,#16236,#16237,#16238,#16239,#16240,#16241,#16242,#16243,
#16244,#16245,#16246,#16247,#16248,#16249,#16250,#16251,#16252,#16253,#16254,
#16255,#16256,#16257,#16258,#16259,#16260,#16261,#16262),(#16263,#16264,
#16265,#16266,#16267,#16268,#16269,#16270,#16271,#16272,#16273,#16274,#16275,
#16276,#16277,#16278,#16279,#16280,#16281,#16282,#16283,#16284,#16285,#16286,
#16287,#16288,#16289,#16290,#16291,#16292,#16293,#16294,#16295,#16296,#16297),
(#16298,#16299,#16300,#16301,#16302,#16303,#16304,#16305,#16306,#16307,
#16308,#16309,#16310,#16311,#16312,#16313,#16314,#16315,#16316,#16317,#16318,
#16319,#16320,#16321,#16322,#16323,#16324,#16325,#16326,#16327,#16328,#16329,
#16330,#16331,#16332),(#16333,#16334,#16335,#16336,#16337,#16338,#16339,
#16340,#16341,#16342,#16343,#16344,#16345,#16346,#16347,#16348,#16349,#16350,
#16351,#16352,#16353,#16354,#16355,#16356,#16357,#16358,#16359,#16360,#16361,
#16362,#16363,#16364,#16365,#16366,#16367)),.UNSPECIFIED.,.F.,.F.,.F.,(4,
4),(4,1,1,1,1,1,1,1,1,1,1,1,1,1,1,1,1,1,1,1,1,1,1,1,1,1,1,1,1,1,1,1,4),
(-0.2613852056804,1.26138520568),(-0.02,0.0125,0.045,0.0775,0.11,0.1425,
0.175,0.2075,0.24,0.2725,0.305,0.3375,0.37,0.4025,0.435,0.4675,0.5,0.5325,
0.565,0.5975,0.63,0.6625,0.695,0.7275,0.76,0.7925,0.825,0.8575,0.89,0.9225,
0.955,0.9875,1.02),.UNSPECIFIED.);
#334=B_SPLINE_SURFACE_WITH_KNOTS('',3,3,((#16369,#16370,#16371,#16372,#16373,
#16374,#16375,#16376,#16377,#16378,#16379,#16380,#16381,#16382,#16383,#16384,
#16385,#16386,#16387,#16388,#16389,#16390,#16391,#16392,#16393,#16394,#16395,
#16396,#16397,#16398,#16399,#16400,#16401,#16402,#16403),(#16404,#16405,
#16406,#16407,#16408,#16409,#16410,#16411,#16412,#16413,#16414,#16415,#16416,
#16417,#16418,#16419,#16420,#16421,#16422,#16423,#16424,#16425,#16426,#16427,
#16428,#16429,#16430,#16431,#16432,#16433,#16434,#16435,#16436,#16437,#16438),
(#16439,#16440,#16441,#16442,#16443,#16444,#16445,#16446,#16447,#16448,
#16449,#16450,#16451,#16452,#16453,#16454,#16455,#16456,#16457,#16458,#16459,
#16460,#16461,#16462,#16463,#16464,#16465,#16466,#16467,#16468,#16469,#16470,
#16471,#16472,#16473),(#16474,#16475,#16476,#16477,#16478,#16479,#16480,
#16481,#16482,#16483,#16484,#16485,#16486,#16487,#16488,#16489,#16490,#16491,
#16492,#16493,#16494,#16495,#16496,#16497,#16498,#16499,#16500,#16501,#16502,
#16503,#16504,#16505,#16506,#16507,#16508)),.UNSPECIFIED.,.F.,.F.,.F.,(4,
4),(4,1,1,1,1,1,1,1,1,1,1,1,1,1,1,1,1,1,1,1,1,1,1,1,1,1,1,1,1,1,1,1,4),
(-0.2613852056804,1.26138520568),(-0.02,0.0125,0.045,0.0775,0.11,0.1425,
0.175,0.2075,0.24,0.2725,0.305,0.3375,0.37,0.4025,0.435,0.4675,0.5,0.5325,
0.565,0.5975,0.63,0.6625,0.695,0.7275,0.76,0.7925,0.825,0.8575,0.89,0.9225,
0.955,0.9875,1.02),.UNSPECIFIED.);
#335=B_SPLINE_SURFACE_WITH_KNOTS('',3,3,((#16732,#16733,#16734,#16735,#16736,
#16737,#16738,#16739,#16740,#16741,#16742,#16743,#16744,#16745,#16746,#16747,
#16748,#16749,#16750,#16751,#16752,#16753,#16754,#16755,#16756,#16757,#16758,
#16759,#16760,#16761,#16762,#16763,#16764,#16765,#16766),(#16767,#16768,
#16769,#16770,#16771,#16772,#16773,#16774,#16775,#16776,#16777,#16778,#16779,
#16780,#16781,#16782,#16783,#16784,#16785,#16786,#16787,#16788,#16789,#16790,
#16791,#16792,#16793,#16794,#16795,#16796,#16797,#16798,#16799,#16800,#16801),
(#16802,#16803,#16804,#16805,#16806,#16807,#16808,#16809,#16810,#16811,
#16812,#16813,#16814,#16815,#16816,#16817,#16818,#16819,#16820,#16821,#16822,
#16823,#16824,#16825,#16826,#16827,#16828,#16829,#16830,#16831,#16832,#16833,
#16834,#16835,#16836),(#16837,#16838,#16839,#16840,#16841,#16842,#16843,
#16844,#16845,#16846,#16847,#16848,#16849,#16850,#16851,#16852,#16853,#16854,
#16855,#16856,#16857,#16858,#16859,#16860,#16861,#16862,#16863,#16864,#16865,
#16866,#16867,#16868,#16869,#16870,#16871)),.UNSPECIFIED.,.F.,.F.,.F.,(4,
4),(4,1,1,1,1,1,1,1,1,1,1,1,1,1,1,1,1,1,1,1,1,1,1,1,1,1,1,1,1,1,1,1,4),
(-0.1560934940397,1.15609349404),(-0.02,0.0125,0.045,0.0775,0.11,0.1425,
0.175,0.2075,0.24,0.2725,0.305,0.3375,0.37,0.4025,0.435,0.4675,0.5,0.5325,
0.565,0.5975,0.63,0.6625,0.695,0.7275,0.76,0.7925,0.825,0.8575,0.89,0.9225,
0.955,0.9875,1.02),.UNSPECIFIED.);
#336=B_SPLINE_SURFACE_WITH_KNOTS('',3,3,((#17004,#17005,#17006,#17007,#17008,
#17009,#17010,#17011,#17012,#17013,#17014,#17015,#17016,#17017,#17018,#17019,
#17020,#17021,#17022,#17023,#17024,#17025,#17026,#17027,#17028,#17029,#17030,
#17031,#17032,#17033,#17034,#17035,#17036,#17037,#17038),(#17039,#17040,
#17041,#17042,#17043,#17044,#17045,#17046,#17047,#17048,#17049,#17050,#17051,
#17052,#17053,#17054,#17055,#17056,#17057,#17058,#17059,#17060,#17061,#17062,
#17063,#17064,#17065,#17066,#17067,#17068,#17069,#17070,#17071,#17072,#17073),
(#17074,#17075,#17076,#17077,#17078,#17079,#17080,#17081,#17082,#17083,
#17084,#17085,#17086,#17087,#17088,#17089,#17090,#17091,#17092,#17093,#17094,
#17095,#17096,#17097,#17098,#17099,#17100,#17101,#17102,#17103,#17104,#17105,
#17106,#17107,#17108),(#17109,#17110,#17111,#17112,#17113,#17114,#17115,
#17116,#17117,#17118,#17119,#17120,#17121,#17122,#17123,#17124,#17125,#17126,
#17127,#17128,#17129,#17130,#17131,#17132,#17133,#17134,#17135,#17136,#17137,
#17138,#17139,#17140,#17141,#17142,#17143)),.UNSPECIFIED.,.F.,.F.,.F.,(4,
4),(4,1,1,1,1,1,1,1,1,1,1,1,1,1,1,1,1,1,1,1,1,1,1,1,1,1,1,1,1,1,1,1,4),
(-0.1560934940397,1.15609349404),(-0.02,0.0125,0.045,0.0775,0.11,0.1425,
0.175,0.2075,0.24,0.2725,0.305,0.3375,0.37,0.4025,0.435,0.4675,0.5,0.5325,
0.565,0.5975,0.63,0.6625,0.695,0.7275,0.76,0.7925,0.825,0.8575,0.89,0.9225,
0.955,0.9875,1.02),.UNSPECIFIED.);
#337=B_SPLINE_SURFACE_WITH_KNOTS('',3,3,((#17202,#17203,#17204,#17205,#17206,
#17207,#17208,#17209,#17210,#17211,#17212,#17213,#17214,#17215,#17216,#17217,
#17218,#17219,#17220,#17221,#17222,#17223,#17224,#17225,#17226,#17227,#17228,
#17229,#17230,#17231,#17232,#17233,#17234,#17235,#17236),(#17237,#17238,
#17239,#17240,#17241,#17242,#17243,#17244,#17245,#17246,#17247,#17248,#17249,
#17250,#17251,#17252,#17253,#17254,#17255,#17256,#17257,#17258,#17259,#17260,
#17261,#17262,#17263,#17264,#17265,#17266,#17267,#17268,#17269,#17270,#17271),
(#17272,#17273,#17274,#17275,#17276,#17277,#17278,#17279,#17280,#17281,
#17282,#17283,#17284,#17285,#17286,#17287,#17288,#17289,#17290,#17291,#17292,
#17293,#17294,#17295,#17296,#17297,#17298,#17299,#17300,#17301,#17302,#17303,
#17304,#17305,#17306),(#17307,#17308,#17309,#17310,#17311,#17312,#17313,
#17314,#17315,#17316,#17317,#17318,#17319,#17320,#17321,#17322,#17323,#17324,
#17325,#17326,#17327,#17328,#17329,#17330,#17331,#17332,#17333,#17334,#17335,
#17336,#17337,#17338,#17339,#17340,#17341)),.UNSPECIFIED.,.F.,.F.,.F.,(4,
4),(4,1,1,1,1,1,1,1,1,1,1,1,1,1,1,1,1,1,1,1,1,1,1,1,1,1,1,1,1,1,1,1,4),
(-0.1560934940397,1.15609349404),(-0.02,0.0125,0.045,0.0775,0.11,0.1425,
0.175,0.2075,0.24,0.2725,0.305,0.3375,0.37,0.4025,0.435,0.4675,0.5,0.5325,
0.565,0.5975,0.63,0.6625,0.695,0.7275,0.76,0.7925,0.825,0.8575,0.89,0.9225,
0.955,0.9875,1.02),.UNSPECIFIED.);
#338=B_SPLINE_SURFACE_WITH_KNOTS('',3,3,((#17618,#17619,#17620,#17621,#17622,
#17623,#17624,#17625,#17626,#17627,#17628,#17629,#17630,#17631,#17632,#17633,
#17634,#17635,#17636,#17637,#17638,#17639,#17640,#17641,#17642,#17643,#17644,
#17645,#17646,#17647,#17648,#17649,#17650,#17651,#17652),(#17653,#17654,
#17655,#17656,#17657,#17658,#17659,#17660,#17661,#17662,#17663,#17664,#17665,
#17666,#17667,#17668,#17669,#17670,#17671,#17672,#17673,#17674,#17675,#17676,
#17677,#17678,#17679,#17680,#17681,#17682,#17683,#17684,#17685,#17686,#17687),
(#17688,#17689,#17690,#17691,#17692,#17693,#17694,#17695,#17696,#17697,
#17698,#17699,#17700,#17701,#17702,#17703,#17704,#17705,#17706,#17707,#17708,
#17709,#17710,#17711,#17712,#17713,#17714,#17715,#17716,#17717,#17718,#17719,
#17720,#17721,#17722),(#17723,#17724,#17725,#17726,#17727,#17728,#17729,
#17730,#17731,#17732,#17733,#17734,#17735,#17736,#17737,#17738,#17739,#17740,
#17741,#17742,#17743,#17744,#17745,#17746,#17747,#17748,#17749,#17750,#17751,
#17752,#17753,#17754,#17755,#17756,#17757)),.UNSPECIFIED.,.F.,.F.,.F.,(4,
4),(4,1,1,1,1,1,1,1,1,1,1,1,1,1,1,1,1,1,1,1,1,1,1,1,1,1,1,1,1,1,1,1,4),
(-0.1560934940397,1.15609349404),(-0.02,0.0125,0.045,0.0775,0.11,0.1425,
0.175,0.2075,0.24,0.2725,0.305,0.3375,0.37,0.4025,0.435,0.4675,0.5,0.5325,
0.565,0.5975,0.63,0.6625,0.695,0.7275,0.76,0.7925,0.825,0.8575,0.89,0.9225,
0.955,0.9875,1.02),.UNSPECIFIED.);
#339=B_SPLINE_SURFACE_WITH_KNOTS('',3,3,((#17870,#17871,#17872,#17873,#17874,
#17875,#17876,#17877,#17878,#17879,#17880,#17881,#17882,#17883,#17884,#17885,
#17886,#17887,#17888,#17889,#17890,#17891,#17892,#17893,#17894,#17895,#17896,
#17897,#17898,#17899,#17900,#17901,#17902,#17903,#17904),(#17905,#17906,
#17907,#17908,#17909,#17910,#17911,#17912,#17913,#17914,#17915,#17916,#17917,
#17918,#17919,#17920,#17921,#17922,#17923,#17924,#17925,#17926,#17927,#17928,
#17929,#17930,#17931,#17932,#17933,#17934,#17935,#17936,#17937,#17938,#17939),
(#17940,#17941,#17942,#17943,#17944,#17945,#17946,#17947,#17948,#17949,
#17950,#17951,#17952,#17953,#17954,#17955,#17956,#17957,#17958,#17959,#17960,
#17961,#17962,#17963,#17964,#17965,#17966,#17967,#17968,#17969,#17970,#17971,
#17972,#17973,#17974),(#17975,#17976,#17977,#17978,#17979,#17980,#17981,
#17982,#17983,#17984,#17985,#17986,#17987,#17988,#17989,#17990,#17991,#17992,
#17993,#17994,#17995,#17996,#17997,#17998,#17999,#18000,#18001,#18002,#18003,
#18004,#18005,#18006,#18007,#18008,#18009)),.UNSPECIFIED.,.F.,.F.,.F.,(4,
4),(4,1,1,1,1,1,1,1,1,1,1,1,1,1,1,1,1,1,1,1,1,1,1,1,1,1,1,1,1,1,1,1,4),
(-0.1560934940397,1.15609349404),(-0.02,0.0125,0.045,0.0775,0.11,0.1425,
0.175,0.2075,0.24,0.2725,0.305,0.3375,0.37,0.4025,0.435,0.4675,0.5,0.5325,
0.565,0.5975,0.63,0.6625,0.695,0.7275,0.76,0.7925,0.825,0.8575,0.89,0.9225,
0.955,0.9875,1.02),.UNSPECIFIED.);
#340=B_SPLINE_SURFACE_WITH_KNOTS('',3,3,((#18261,#18262,#18263,#18264,#18265,
#18266,#18267,#18268,#18269,#18270,#18271,#18272,#18273,#18274,#18275,#18276,
#18277,#18278,#18279,#18280,#18281,#18282,#18283,#18284,#18285,#18286,#18287,
#18288,#18289,#18290,#18291,#18292,#18293,#18294,#18295),(#18296,#18297,
#18298,#18299,#18300,#18301,#18302,#18303,#18304,#18305,#18306,#18307,#18308,
#18309,#18310,#18311,#18312,#18313,#18314,#18315,#18316,#18317,#18318,#18319,
#18320,#18321,#18322,#18323,#18324,#18325,#18326,#18327,#18328,#18329,#18330),
(#18331,#18332,#18333,#18334,#18335,#18336,#18337,#18338,#18339,#18340,
#18341,#18342,#18343,#18344,#18345,#18346,#18347,#18348,#18349,#18350,#18351,
#18352,#18353,#18354,#18355,#18356,#18357,#18358,#18359,#18360,#18361,#18362,
#18363,#18364,#18365),(#18366,#18367,#18368,#18369,#18370,#18371,#18372,
#18373,#18374,#18375,#18376,#18377,#18378,#18379,#18380,#18381,#18382,#18383,
#18384,#18385,#18386,#18387,#18388,#18389,#18390,#18391,#18392,#18393,#18394,
#18395,#18396,#18397,#18398,#18399,#18400)),.UNSPECIFIED.,.F.,.F.,.F.,(4,
4),(4,1,1,1,1,1,1,1,1,1,1,1,1,1,1,1,1,1,1,1,1,1,1,1,1,1,1,1,1,1,1,1,4),
(-0.1560934940397,1.15609349404),(-0.0177116462091,0.01106977888069,0.03985120397047,
0.06863262906025,0.09741405415003,0.1261954792398,0.1549769043296,0.1837583294194,
0.2125397545092,0.2413211795989,0.2701026046887,0.2988840297785,0.3276654548683,
0.3564468799581,0.3852283050479,0.4140097301376,0.4427911552274,0.4715725803172,
0.500354005407,0.5291354304968,0.5579168555866,0.5866982806763,0.6154797057661,
0.6442611308559,0.6730425559457,0.7018239810355,0.7306054061252,0.759386831215,
0.7881682563048,0.8169496813946,0.8457311064844,0.8745125315742,0.9032939566639),
 .UNSPECIFIED.);
#341=B_SPLINE_SURFACE_WITH_KNOTS('',3,3,((#18688,#18689,#18690,#18691,#18692,
#18693,#18694,#18695,#18696,#18697,#18698,#18699,#18700,#18701,#18702,#18703,
#18704,#18705,#18706,#18707,#18708,#18709,#18710,#18711,#18712,#18713,#18714,
#18715,#18716,#18717,#18718,#18719,#18720,#18721,#18722),(#18723,#18724,
#18725,#18726,#18727,#18728,#18729,#18730,#18731,#18732,#18733,#18734,#18735,
#18736,#18737,#18738,#18739,#18740,#18741,#18742,#18743,#18744,#18745,#18746,
#18747,#18748,#18749,#18750,#18751,#18752,#18753,#18754,#18755,#18756,#18757),
(#18758,#18759,#18760,#18761,#18762,#18763,#18764,#18765,#18766,#18767,
#18768,#18769,#18770,#18771,#18772,#18773,#18774,#18775,#18776,#18777,#18778,
#18779,#18780,#18781,#18782,#18783,#18784,#18785,#18786,#18787,#18788,#18789,
#18790,#18791,#18792),(#18793,#18794,#18795,#18796,#18797,#18798,#18799,
#18800,#18801,#18802,#18803,#18804,#18805,#18806,#18807,#18808,#18809,#18810,
#18811,#18812,#18813,#18814,#18815,#18816,#18817,#18818,#18819,#18820,#18821,
#18822,#18823,#18824,#18825,#18826,#18827)),.UNSPECIFIED.,.F.,.F.,.F.,(4,
4),(4,1,1,1,1,1,1,1,1,1,1,1,1,1,1,1,1,1,1,1,1,1,1,1,1,1,1,1,1,1,1,1,4),
(-0.2613852056804,1.26138520568),(-0.01995502045757,0.01247188778598,0.04489879602953,
0.07732570427308,0.1097526125166,0.1421795207602,0.1746064290037,0.2070333372473,
0.2394602454908,0.2718871537344,0.3043140619779,0.3367409702215,0.369167878465,
0.4015947867086,0.4340216949521,0.4664486031957,0.4988755114392,0.5313024196828,
0.5637293279263,0.5961562361699,0.6285831444134,0.661010052657,0.6934369609005,
0.7258638691441,0.7582907773876,0.7907176856312,0.8231445938748,0.8555715021183,
0.8879984103619,0.9204253186054,0.952852226849,0.9852791350925,1.017706043336),
 .UNSPECIFIED.);
#342=B_SPLINE_SURFACE_WITH_KNOTS('',3,3,((#18829,#18830,#18831,#18832,#18833,
#18834,#18835,#18836,#18837,#18838,#18839,#18840,#18841,#18842,#18843,#18844,
#18845,#18846,#18847,#18848,#18849,#18850,#18851,#18852,#18853,#18854,#18855,
#18856,#18857,#18858,#18859,#18860,#18861,#18862,#18863),(#18864,#18865,
#18866,#18867,#18868,#18869,#18870,#18871,#18872,#18873,#18874,#18875,#18876,
#18877,#18878,#18879,#18880,#18881,#18882,#18883,#18884,#18885,#18886,#18887,
#18888,#18889,#18890,#18891,#18892,#18893,#18894,#18895,#18896,#18897,#18898),
(#18899,#18900,#18901,#18902,#18903,#18904,#18905,#18906,#18907,#18908,
#18909,#18910,#18911,#18912,#18913,#18914,#18915,#18916,#18917,#18918,#18919,
#18920,#18921,#18922,#18923,#18924,#18925,#18926,#18927,#18928,#18929,#18930,
#18931,#18932,#18933),(#18934,#18935,#18936,#18937,#18938,#18939,#18940,
#18941,#18942,#18943,#18944,#18945,#18946,#18947,#18948,#18949,#18950,#18951,
#18952,#18953,#18954,#18955,#18956,#18957,#18958,#18959,#18960,#18961,#18962,
#18963,#18964,#18965,#18966,#18967,#18968)),.UNSPECIFIED.,.F.,.F.,.F.,(4,
4),(4,1,1,1,1,1,1,1,1,1,1,1,1,1,1,1,1,1,1,1,1,1,1,1,1,1,1,1,1,1,1,1,4),
(-0.2613852056804,1.26138520568),(-0.02,0.0125,0.045,0.0775,0.11,0.1425,
0.175,0.2075,0.24,0.2725,0.305,0.3375,0.37,0.4025,0.435,0.4675,0.5,0.5325,
0.565,0.5975,0.63,0.6625,0.695,0.7275,0.76,0.7925,0.825,0.8575,0.89,0.9225,
0.955,0.9875,1.02),.UNSPECIFIED.);
#343=B_SPLINE_SURFACE_WITH_KNOTS('',3,3,((#20414,#20415,#20416,#20417,#20418,
#20419,#20420,#20421,#20422,#20423,#20424,#20425,#20426,#20427,#20428,#20429,
#20430,#20431,#20432,#20433,#20434,#20435,#20436,#20437,#20438,#20439,#20440,
#20441,#20442,#20443,#20444,#20445,#20446,#20447,#20448),(#20449,#20450,
#20451,#20452,#20453,#20454,#20455,#20456,#20457,#20458,#20459,#20460,#20461,
#20462,#20463,#20464,#20465,#20466,#20467,#20468,#20469,#20470,#20471,#20472,
#20473,#20474,#20475,#20476,#20477,#20478,#20479,#20480,#20481,#20482,#20483),
(#20484,#20485,#20486,#20487,#20488,#20489,#20490,#20491,#20492,#20493,
#20494,#20495,#20496,#20497,#20498,#20499,#20500,#20501,#20502,#20503,#20504,
#20505,#20506,#20507,#20508,#20509,#20510,#20511,#20512,#20513,#20514,#20515,
#20516,#20517,#20518),(#20519,#20520,#20521,#20522,#20523,#20524,#20525,
#20526,#20527,#20528,#20529,#20530,#20531,#20532,#20533,#20534,#20535,#20536,
#20537,#20538,#20539,#20540,#20541,#20542,#20543,#20544,#20545,#20546,#20547,
#20548,#20549,#20550,#20551,#20552,#20553)),.UNSPECIFIED.,.F.,.F.,.F.,(4,
4),(4,1,1,1,1,1,1,1,1,1,1,1,1,1,1,1,1,1,1,1,1,1,1,1,1,1,1,1,1,1,1,1,4),
(-0.1053316651847,1.105331665185),(-0.01760502747868,0.01100314217417,0.03961131182703,
0.06821948147988,0.09682765113273,0.1254358207856,0.1540439904384,0.1826521600913,
0.2112603297441,0.239868499397,0.2684766690498,0.2970848387027,0.3256930083555,
0.3543011780084,0.3829093476613,0.4115175173141,0.440125686967,0.4687338566198,
0.4973420262727,0.5259501959255,0.5545583655784,0.5831665352312,0.6117747048841,
0.6403828745369,0.6689910441898,0.6975992138426,0.7262073834955,0.7548155531483,
0.7834237228012,0.812031892454,0.8406400621069,0.8692482317597,0.8978564014126),
 .UNSPECIFIED.);
#344=B_SPLINE_SURFACE_WITH_KNOTS('',3,3,((#20875,#20876,#20877,#20878,#20879,
#20880,#20881,#20882,#20883,#20884,#20885,#20886,#20887,#20888,#20889,#20890,
#20891,#20892,#20893,#20894,#20895,#20896,#20897,#20898,#20899,#20900,#20901,
#20902,#20903,#20904,#20905,#20906,#20907,#20908,#20909),(#20910,#20911,
#20912,#20913,#20914,#20915,#20916,#20917,#20918,#20919,#20920,#20921,#20922,
#20923,#20924,#20925,#20926,#20927,#20928,#20929,#20930,#20931,#20932,#20933,
#20934,#20935,#20936,#20937,#20938,#20939,#20940,#20941,#20942,#20943,#20944),
(#20945,#20946,#20947,#20948,#20949,#20950,#20951,#20952,#20953,#20954,
#20955,#20956,#20957,#20958,#20959,#20960,#20961,#20962,#20963,#20964,#20965,
#20966,#20967,#20968,#20969,#20970,#20971,#20972,#20973,#20974,#20975,#20976,
#20977,#20978,#20979),(#20980,#20981,#20982,#20983,#20984,#20985,#20986,
#20987,#20988,#20989,#20990,#20991,#20992,#20993,#20994,#20995,#20996,#20997,
#20998,#20999,#21000,#21001,#21002,#21003,#21004,#21005,#21006,#21007,#21008,
#21009,#21010,#21011,#21012,#21013,#21014)),.UNSPECIFIED.,.F.,.F.,.F.,(4,
4),(4,1,1,1,1,1,1,1,1,1,1,1,1,1,1,1,1,1,1,1,1,1,1,1,1,1,1,1,1,1,1,1,4),
(-0.1053316651848,1.105331665185),(-0.02,0.0125,0.045,0.0775,0.11,0.1425,
0.175,0.2075,0.24,0.2725,0.305,0.3375,0.37,0.4025,0.435,0.4675,0.5,0.5325,
0.565,0.5975,0.63,0.6625,0.695,0.7275,0.76,0.7925,0.825,0.8575,0.89,0.9225,
0.955,0.9875,1.02),.UNSPECIFIED.);
#345=B_SPLINE_SURFACE_WITH_KNOTS('',3,3,((#21330,#21331,#21332,#21333,#21334,
#21335,#21336,#21337,#21338,#21339,#21340,#21341,#21342,#21343,#21344,#21345,
#21346,#21347,#21348,#21349,#21350,#21351,#21352,#21353,#21354,#21355,#21356,
#21357,#21358,#21359,#21360,#21361,#21362,#21363,#21364),(#21365,#21366,
#21367,#21368,#21369,#21370,#21371,#21372,#21373,#21374,#21375,#21376,#21377,
#21378,#21379,#21380,#21381,#21382,#21383,#21384,#21385,#21386,#21387,#21388,
#21389,#21390,#21391,#21392,#21393,#21394,#21395,#21396,#21397,#21398,#21399),
(#21400,#21401,#21402,#21403,#21404,#21405,#21406,#21407,#21408,#21409,
#21410,#21411,#21412,#21413,#21414,#21415,#21416,#21417,#21418,#21419,#21420,
#21421,#21422,#21423,#21424,#21425,#21426,#21427,#21428,#21429,#21430,#21431,
#21432,#21433,#21434),(#21435,#21436,#21437,#21438,#21439,#21440,#21441,
#21442,#21443,#21444,#21445,#21446,#21447,#21448,#21449,#21450,#21451,#21452,
#21453,#21454,#21455,#21456,#21457,#21458,#21459,#21460,#21461,#21462,#21463,
#21464,#21465,#21466,#21467,#21468,#21469)),.UNSPECIFIED.,.F.,.F.,.F.,(4,
4),(4,1,1,1,1,1,1,1,1,1,1,1,1,1,1,1,1,1,1,1,1,1,1,1,1,1,1,1,1,1,1,1,4),
(-0.3507678241798,1.35076782418),(-0.01888802807688,0.01180501754805,0.04249806317297,
0.0731911087979,0.1038841544228,0.1345772000478,0.1652702456727,0.1959632912976,
0.2266563369225,0.2573493825475,0.2880424281724,0.3187354737973,0.3494285194222,
0.3801215650472,0.4108146106721,0.441507656297,0.4722007019219,0.5028937475469,
0.5335867931718,0.5642798387967,0.5949728844216,0.6256659300466,0.6563589756715,
0.6870520212964,0.7177450669213,0.7484381125463,0.7791311581712,0.8098242037961,
0.840517249421,0.871210295046,0.9019033406709,0.9325963862958,0.9632894319207),
 .UNSPECIFIED.);
#346=B_SPLINE_SURFACE_WITH_KNOTS('',3,3,((#21471,#21472,#21473,#21474,#21475,
#21476,#21477,#21478,#21479,#21480,#21481,#21482,#21483,#21484,#21485,#21486,
#21487,#21488,#21489,#21490,#21491,#21492,#21493,#21494,#21495,#21496,#21497,
#21498,#21499,#21500,#21501,#21502,#21503,#21504,#21505),(#21506,#21507,
#21508,#21509,#21510,#21511,#21512,#21513,#21514,#21515,#21516,#21517,#21518,
#21519,#21520,#21521,#21522,#21523,#21524,#21525,#21526,#21527,#21528,#21529,
#21530,#21531,#21532,#21533,#21534,#21535,#21536,#21537,#21538,#21539,#21540),
(#21541,#21542,#21543,#21544,#21545,#21546,#21547,#21548,#21549,#21550,
#21551,#21552,#21553,#21554,#21555,#21556,#21557,#21558,#21559,#21560,#21561,
#21562,#21563,#21564,#21565,#21566,#21567,#21568,#21569,#21570,#21571,#21572,
#21573,#21574,#21575),(#21576,#21577,#21578,#21579,#21580,#21581,#21582,
#21583,#21584,#21585,#21586,#21587,#21588,#21589,#21590,#21591,#21592,#21593,
#21594,#21595,#21596,#21597,#21598,#21599,#21600,#21601,#21602,#21603,#21604,
#21605,#21606,#21607,#21608,#21609,#21610)),.UNSPECIFIED.,.F.,.F.,.F.,(4,
4),(4,1,1,1,1,1,1,1,1,1,1,1,1,1,1,1,1,1,1,1,1,1,1,1,1,1,1,1,1,1,1,1,4),
(-0.3507678241798,1.35076782418),(-0.02,0.0125,0.045,0.0775,0.11,0.1425,
0.175,0.2075,0.24,0.2725,0.305,0.3375,0.37,0.4025,0.435,0.4675,0.5,0.5325,
0.565,0.5975,0.63,0.6625,0.695,0.7275,0.76,0.7925,0.825,0.8575,0.89,0.9225,
0.955,0.9875,1.02),.UNSPECIFIED.);
#347=B_SPLINE_SURFACE_WITH_KNOTS('',3,3,((#21858,#21859,#21860,#21861,#21862,
#21863,#21864,#21865,#21866,#21867,#21868,#21869,#21870,#21871,#21872,#21873,
#21874,#21875,#21876,#21877,#21878,#21879,#21880,#21881,#21882,#21883,#21884,
#21885,#21886,#21887,#21888,#21889,#21890,#21891,#21892),(#21893,#21894,
#21895,#21896,#21897,#21898,#21899,#21900,#21901,#21902,#21903,#21904,#21905,
#21906,#21907,#21908,#21909,#21910,#21911,#21912,#21913,#21914,#21915,#21916,
#21917,#21918,#21919,#21920,#21921,#21922,#21923,#21924,#21925,#21926,#21927),
(#21928,#21929,#21930,#21931,#21932,#21933,#21934,#21935,#21936,#21937,
#21938,#21939,#21940,#21941,#21942,#21943,#21944,#21945,#21946,#21947,#21948,
#21949,#21950,#21951,#21952,#21953,#21954,#21955,#21956,#21957,#21958,#21959,
#21960,#21961,#21962),(#21963,#21964,#21965,#21966,#21967,#21968,#21969,
#21970,#21971,#21972,#21973,#21974,#21975,#21976,#21977,#21978,#21979,#21980,
#21981,#21982,#21983,#21984,#21985,#21986,#21987,#21988,#21989,#21990,#21991,
#21992,#21993,#21994,#21995,#21996,#21997)),.UNSPECIFIED.,.F.,.F.,.F.,(4,
4),(4,1,1,1,1,1,1,1,1,1,1,1,1,1,1,1,1,1,1,1,1,1,1,1,1,1,1,1,1,1,1,1,4),
(-0.3507678241798,1.35076782418),(-0.02,0.0125,0.045,0.0775,0.11,0.1425,
0.175,0.2075,0.24,0.2725,0.305,0.3375,0.37,0.4025,0.435,0.4675,0.5,0.5325,
0.565,0.5975,0.63,0.6625,0.695,0.7275,0.76,0.7925,0.825,0.8575,0.89,0.9225,
0.955,0.9875,1.02),.UNSPECIFIED.);
#348=B_SPLINE_SURFACE_WITH_KNOTS('',3,3,((#22245,#22246,#22247,#22248,#22249,
#22250,#22251,#22252,#22253,#22254,#22255,#22256,#22257,#22258,#22259,#22260,
#22261,#22262,#22263,#22264,#22265,#22266,#22267,#22268,#22269,#22270,#22271,
#22272,#22273,#22274,#22275,#22276,#22277,#22278,#22279),(#22280,#22281,
#22282,#22283,#22284,#22285,#22286,#22287,#22288,#22289,#22290,#22291,#22292,
#22293,#22294,#22295,#22296,#22297,#22298,#22299,#22300,#22301,#22302,#22303,
#22304,#22305,#22306,#22307,#22308,#22309,#22310,#22311,#22312,#22313,#22314),
(#22315,#22316,#22317,#22318,#22319,#22320,#22321,#22322,#22323,#22324,
#22325,#22326,#22327,#22328,#22329,#22330,#22331,#22332,#22333,#22334,#22335,
#22336,#22337,#22338,#22339,#22340,#22341,#22342,#22343,#22344,#22345,#22346,
#22347,#22348,#22349),(#22350,#22351,#22352,#22353,#22354,#22355,#22356,
#22357,#22358,#22359,#22360,#22361,#22362,#22363,#22364,#22365,#22366,#22367,
#22368,#22369,#22370,#22371,#22372,#22373,#22374,#22375,#22376,#22377,#22378,
#22379,#22380,#22381,#22382,#22383,#22384)),.UNSPECIFIED.,.F.,.F.,.F.,(4,
4),(4,1,1,1,1,1,1,1,1,1,1,1,1,1,1,1,1,1,1,1,1,1,1,1,1,1,1,1,1,1,1,1,4),
(-0.3507678241798,1.35076782418),(-0.02,0.0125,0.045,0.0775,0.11,0.1425,
0.175,0.2075,0.24,0.2725,0.305,0.3375,0.37,0.4025,0.435,0.4675,0.5,0.5325,
0.565,0.5975,0.63,0.6625,0.695,0.7275,0.76,0.7925,0.825,0.8575,0.89,0.9225,
0.955,0.9875,1.02),.UNSPECIFIED.);
#349=B_SPLINE_SURFACE_WITH_KNOTS('',3,3,((#22632,#22633,#22634,#22635,#22636,
#22637,#22638,#22639,#22640,#22641,#22642,#22643,#22644,#22645,#22646,#22647,
#22648,#22649,#22650,#22651,#22652,#22653,#22654,#22655,#22656,#22657,#22658,
#22659,#22660,#22661,#22662,#22663,#22664,#22665,#22666),(#22667,#22668,
#22669,#22670,#22671,#22672,#22673,#22674,#22675,#22676,#22677,#22678,#22679,
#22680,#22681,#22682,#22683,#22684,#22685,#22686,#22687,#22688,#22689,#22690,
#22691,#22692,#22693,#22694,#22695,#22696,#22697,#22698,#22699,#22700,#22701),
(#22702,#22703,#22704,#22705,#22706,#22707,#22708,#22709,#22710,#22711,
#22712,#22713,#22714,#22715,#22716,#22717,#22718,#22719,#22720,#22721,#22722,
#22723,#22724,#22725,#22726,#22727,#22728,#22729,#22730,#22731,#22732,#22733,
#22734,#22735,#22736),(#22737,#22738,#22739,#22740,#22741,#22742,#22743,
#22744,#22745,#22746,#22747,#22748,#22749,#22750,#22751,#22752,#22753,#22754,
#22755,#22756,#22757,#22758,#22759,#22760,#22761,#22762,#22763,#22764,#22765,
#22766,#22767,#22768,#22769,#22770,#22771)),.UNSPECIFIED.,.F.,.F.,.F.,(4,
4),(4,1,1,1,1,1,1,1,1,1,1,1,1,1,1,1,1,1,1,1,1,1,1,1,1,1,1,1,1,1,1,1,4),
(-0.3507678241798,1.35076782418),(-0.02,0.0125,0.045,0.0775,0.11,0.1425,
0.175,0.2075,0.24,0.2725,0.305,0.3375,0.37,0.4025,0.435,0.4675,0.5,0.5325,
0.565,0.5975,0.63,0.6625,0.695,0.7275,0.76,0.7925,0.825,0.8575,0.89,0.9225,
0.955,0.9875,1.02),.UNSPECIFIED.);
#350=B_SPLINE_SURFACE_WITH_KNOTS('',3,3,((#23060,#23061,#23062,#23063,#23064,
#23065,#23066,#23067,#23068,#23069,#23070,#23071,#23072,#23073,#23074,#23075,
#23076,#23077,#23078,#23079,#23080,#23081,#23082,#23083,#23084,#23085,#23086,
#23087,#23088,#23089,#23090,#23091,#23092,#23093,#23094),(#23095,#23096,
#23097,#23098,#23099,#23100,#23101,#23102,#23103,#23104,#23105,#23106,#23107,
#23108,#23109,#23110,#23111,#23112,#23113,#23114,#23115,#23116,#23117,#23118,
#23119,#23120,#23121,#23122,#23123,#23124,#23125,#23126,#23127,#23128,#23129),
(#23130,#23131,#23132,#23133,#23134,#23135,#23136,#23137,#23138,#23139,
#23140,#23141,#23142,#23143,#23144,#23145,#23146,#23147,#23148,#23149,#23150,
#23151,#23152,#23153,#23154,#23155,#23156,#23157,#23158,#23159,#23160,#23161,
#23162,#23163,#23164),(#23165,#23166,#23167,#23168,#23169,#23170,#23171,
#23172,#23173,#23174,#23175,#23176,#23177,#23178,#23179,#23180,#23181,#23182,
#23183,#23184,#23185,#23186,#23187,#23188,#23189,#23190,#23191,#23192,#23193,
#23194,#23195,#23196,#23197,#23198,#23199)),.UNSPECIFIED.,.F.,.F.,.F.,(4,
4),(4,1,1,1,1,1,1,1,1,1,1,1,1,1,1,1,1,1,1,1,1,1,1,1,1,1,1,1,1,1,1,1,4),
(-0.1053316651848,1.105331665185),(-0.02,0.0125,0.045,0.0775,0.11,0.1425,
0.175,0.2075,0.24,0.2725,0.305,0.3375,0.37,0.4025,0.435,0.4675,0.5,0.5325,
0.565,0.5975,0.63,0.6625,0.695,0.7275,0.76,0.7925,0.825,0.8575,0.89,0.9225,
0.955,0.9875,1.02),.UNSPECIFIED.);
#351=B_SPLINE_SURFACE_WITH_KNOTS('',3,3,((#23447,#23448,#23449,#23450,#23451,
#23452,#23453,#23454,#23455,#23456,#23457,#23458,#23459,#23460,#23461,#23462,
#23463,#23464,#23465,#23466,#23467,#23468,#23469,#23470,#23471,#23472,#23473,
#23474,#23475,#23476,#23477,#23478,#23479,#23480,#23481),(#23482,#23483,
#23484,#23485,#23486,#23487,#23488,#23489,#23490,#23491,#23492,#23493,#23494,
#23495,#23496,#23497,#23498,#23499,#23500,#23501,#23502,#23503,#23504,#23505,
#23506,#23507,#23508,#23509,#23510,#23511,#23512,#23513,#23514,#23515,#23516),
(#23517,#23518,#23519,#23520,#23521,#23522,#23523,#23524,#23525,#23526,
#23527,#23528,#23529,#23530,#23531,#23532,#23533,#23534,#23535,#23536,#23537,
#23538,#23539,#23540,#23541,#23542,#23543,#23544,#23545,#23546,#23547,#23548,
#23549,#23550,#23551),(#23552,#23553,#23554,#23555,#23556,#23557,#23558,
#23559,#23560,#23561,#23562,#23563,#23564,#23565,#23566,#23567,#23568,#23569,
#23570,#23571,#23572,#23573,#23574,#23575,#23576,#23577,#23578,#23579,#23580,
#23581,#23582,#23583,#23584,#23585,#23586)),.UNSPECIFIED.,.F.,.F.,.F.,(4,
4),(4,1,1,1,1,1,1,1,1,1,1,1,1,1,1,1,1,1,1,1,1,1,1,1,1,1,1,1,1,1,1,1,4),
(-0.1053316651847,1.105331665185),(-0.02,0.0125,0.045,0.0775,0.11,0.1425,
0.175,0.2075,0.24,0.2725,0.305,0.3375,0.37,0.4025,0.435,0.4675,0.5,0.5325,
0.565,0.5975,0.63,0.6625,0.695,0.7275,0.76,0.7925,0.825,0.8575,0.89,0.9225,
0.955,0.9875,1.02),.UNSPECIFIED.);
#352=B_SPLINE_SURFACE_WITH_KNOTS('',3,3,((#23641,#23642,#23643,#23644,#23645,
#23646,#23647,#23648,#23649,#23650,#23651,#23652,#23653,#23654,#23655,#23656,
#23657,#23658,#23659,#23660,#23661,#23662,#23663,#23664,#23665,#23666,#23667,
#23668,#23669,#23670,#23671,#23672,#23673,#23674,#23675),(#23676,#23677,
#23678,#23679,#23680,#23681,#23682,#23683,#23684,#23685,#23686,#23687,#23688,
#23689,#23690,#23691,#23692,#23693,#23694,#23695,#23696,#23697,#23698,#23699,
#23700,#23701,#23702,#23703,#23704,#23705,#23706,#23707,#23708,#23709,#23710),
(#23711,#23712,#23713,#23714,#23715,#23716,#23717,#23718,#23719,#23720,
#23721,#23722,#23723,#23724,#23725,#23726,#23727,#23728,#23729,#23730,#23731,
#23732,#23733,#23734,#23735,#23736,#23737,#23738,#23739,#23740,#23741,#23742,
#23743,#23744,#23745),(#23746,#23747,#23748,#23749,#23750,#23751,#23752,
#23753,#23754,#23755,#23756,#23757,#23758,#23759,#23760,#23761,#23762,#23763,
#23764,#23765,#23766,#23767,#23768,#23769,#23770,#23771,#23772,#23773,#23774,
#23775,#23776,#23777,#23778,#23779,#23780)),.UNSPECIFIED.,.F.,.F.,.F.,(4,
4),(4,1,1,1,1,1,1,1,1,1,1,1,1,1,1,1,1,1,1,1,1,1,1,1,1,1,1,1,1,1,1,1,4),
(-0.1053316651847,1.105331665185),(-0.02,0.0125,0.045,0.0775,0.11,0.1425,
0.175,0.2075,0.24,0.2725,0.305,0.3375,0.37,0.4025,0.435,0.4675,0.5,0.5325,
0.565,0.5975,0.63,0.6625,0.695,0.7275,0.76,0.7925,0.825,0.8575,0.89,0.9225,
0.955,0.9875,1.02),.UNSPECIFIED.);
#353=B_SPLINE_SURFACE_WITH_KNOTS('',3,3,((#24018,#24019,#24020,#24021,#24022,
#24023,#24024,#24025,#24026,#24027,#24028,#24029,#24030,#24031,#24032,#24033,
#24034,#24035,#24036,#24037,#24038,#24039,#24040,#24041,#24042,#24043,#24044,
#24045,#24046,#24047,#24048,#24049,#24050,#24051,#24052),(#24053,#24054,
#24055,#24056,#24057,#24058,#24059,#24060,#24061,#24062,#24063,#24064,#24065,
#24066,#24067,#24068,#24069,#24070,#24071,#24072,#24073,#24074,#24075,#24076,
#24077,#24078,#24079,#24080,#24081,#24082,#24083,#24084,#24085,#24086,#24087),
(#24088,#24089,#24090,#24091,#24092,#24093,#24094,#24095,#24096,#24097,
#24098,#24099,#24100,#24101,#24102,#24103,#24104,#24105,#24106,#24107,#24108,
#24109,#24110,#24111,#24112,#24113,#24114,#24115,#24116,#24117,#24118,#24119,
#24120,#24121,#24122),(#24123,#24124,#24125,#24126,#24127,#24128,#24129,
#24130,#24131,#24132,#24133,#24134,#24135,#24136,#24137,#24138,#24139,#24140,
#24141,#24142,#24143,#24144,#24145,#24146,#24147,#24148,#24149,#24150,#24151,
#24152,#24153,#24154,#24155,#24156,#24157)),.UNSPECIFIED.,.F.,.F.,.F.,(4,
4),(4,1,1,1,1,1,1,1,1,1,1,1,1,1,1,1,1,1,1,1,1,1,1,1,1,1,1,1,1,1,1,1,4),
(-0.1053316651848,1.105331665185),(-0.02,0.0125,0.045,0.0775,0.11,0.1425,
0.175,0.2075,0.24,0.2725,0.305,0.3375,0.37,0.4025,0.435,0.4675,0.5,0.5325,
0.565,0.5975,0.63,0.6625,0.695,0.7275,0.76,0.7925,0.825,0.8575,0.89,0.9225,
0.955,0.9875,1.02),.UNSPECIFIED.);
#354=B_SPLINE_SURFACE_WITH_KNOTS('',3,3,((#24159,#24160,#24161,#24162,#24163,
#24164,#24165,#24166,#24167,#24168,#24169,#24170,#24171,#24172,#24173,#24174,
#24175,#24176,#24177,#24178,#24179,#24180,#24181,#24182,#24183,#24184,#24185,
#24186,#24187,#24188,#24189,#24190,#24191,#24192,#24193),(#24194,#24195,
#24196,#24197,#24198,#24199,#24200,#24201,#24202,#24203,#24204,#24205,#24206,
#24207,#24208,#24209,#24210,#24211,#24212,#24213,#24214,#24215,#24216,#24217,
#24218,#24219,#24220,#24221,#24222,#24223,#24224,#24225,#24226,#24227,#24228),
(#24229,#24230,#24231,#24232,#24233,#24234,#24235,#24236,#24237,#24238,
#24239,#24240,#24241,#24242,#24243,#24244,#24245,#24246,#24247,#24248,#24249,
#24250,#24251,#24252,#24253,#24254,#24255,#24256,#24257,#24258,#24259,#24260,
#24261,#24262,#24263),(#24264,#24265,#24266,#24267,#24268,#24269,#24270,
#24271,#24272,#24273,#24274,#24275,#24276,#24277,#24278,#24279,#24280,#24281,
#24282,#24283,#24284,#24285,#24286,#24287,#24288,#24289,#24290,#24291,#24292,
#24293,#24294,#24295,#24296,#24297,#24298)),.UNSPECIFIED.,.F.,.F.,.F.,(4,
4),(4,1,1,1,1,1,1,1,1,1,1,1,1,1,1,1,1,1,1,1,1,1,1,1,1,1,1,1,1,1,1,1,4),
(-0.1053316651848,1.105331665185),(-0.02,0.0125,0.045,0.0775,0.11,0.1425,
0.175,0.2075,0.24,0.2725,0.305,0.3375,0.37,0.4025,0.435,0.4675,0.5,0.5325,
0.565,0.5975,0.63,0.6625,0.695,0.7275,0.76,0.7925,0.825,0.8575,0.89,0.9225,
0.955,0.9875,1.02),.UNSPECIFIED.);
#355=B_SPLINE_SURFACE_WITH_KNOTS('',3,3,((#24485,#24486,#24487,#24488,#24489,
#24490,#24491,#24492,#24493,#24494,#24495,#24496,#24497,#24498,#24499,#24500,
#24501,#24502,#24503,#24504,#24505,#24506,#24507,#24508,#24509,#24510,#24511,
#24512,#24513,#24514,#24515,#24516,#24517,#24518,#24519),(#24520,#24521,
#24522,#24523,#24524,#24525,#24526,#24527,#24528,#24529,#24530,#24531,#24532,
#24533,#24534,#24535,#24536,#24537,#24538,#24539,#24540,#24541,#24542,#24543,
#24544,#24545,#24546,#24547,#24548,#24549,#24550,#24551,#24552,#24553,#24554),
(#24555,#24556,#24557,#24558,#24559,#24560,#24561,#24562,#24563,#24564,
#24565,#24566,#24567,#24568,#24569,#24570,#24571,#24572,#24573,#24574,#24575,
#24576,#24577,#24578,#24579,#24580,#24581,#24582,#24583,#24584,#24585,#24586,
#24587,#24588,#24589),(#24590,#24591,#24592,#24593,#24594,#24595,#24596,
#24597,#24598,#24599,#24600,#24601,#24602,#24603,#24604,#24605,#24606,#24607,
#24608,#24609,#24610,#24611,#24612,#24613,#24614,#24615,#24616,#24617,#24618,
#24619,#24620,#24621,#24622,#24623,#24624)),.UNSPECIFIED.,.F.,.F.,.F.,(4,
4),(4,1,1,1,1,1,1,1,1,1,1,1,1,1,1,1,1,1,1,1,1,1,1,1,1,1,1,1,1,1,1,1,4),
(-0.1053316651847,1.105331665185),(-0.02,0.0125,0.045,0.0775,0.11,0.1425,
0.175,0.2075,0.24,0.2725,0.305,0.3375,0.37,0.4025,0.435,0.4675,0.5,0.5325,
0.565,0.5975,0.63,0.6625,0.695,0.7275,0.76,0.7925,0.825,0.8575,0.89,0.9225,
0.955,0.9875,1.02),.UNSPECIFIED.);
#356=B_SPLINE_SURFACE_WITH_KNOTS('',3,3,((#24675,#24676,#24677,#24678,#24679,
#24680,#24681,#24682,#24683,#24684,#24685,#24686,#24687,#24688,#24689,#24690,
#24691,#24692,#24693,#24694,#24695,#24696,#24697,#24698,#24699,#24700,#24701,
#24702,#24703,#24704,#24705,#24706,#24707,#24708,#24709),(#24710,#24711,
#24712,#24713,#24714,#24715,#24716,#24717,#24718,#24719,#24720,#24721,#24722,
#24723,#24724,#24725,#24726,#24727,#24728,#24729,#24730,#24731,#24732,#24733,
#24734,#24735,#24736,#24737,#24738,#24739,#24740,#24741,#24742,#24743,#24744),
(#24745,#24746,#24747,#24748,#24749,#24750,#24751,#24752,#24753,#24754,
#24755,#24756,#24757,#24758,#24759,#24760,#24761,#24762,#24763,#24764,#24765,
#24766,#24767,#24768,#24769,#24770,#24771,#24772,#24773,#24774,#24775,#24776,
#24777,#24778,#24779),(#24780,#24781,#24782,#24783,#24784,#24785,#24786,
#24787,#24788,#24789,#24790,#24791,#24792,#24793,#24794,#24795,#24796,#24797,
#24798,#24799,#24800,#24801,#24802,#24803,#24804,#24805,#24806,#24807,#24808,
#24809,#24810,#24811,#24812,#24813,#24814)),.UNSPECIFIED.,.F.,.F.,.F.,(4,
4),(4,1,1,1,1,1,1,1,1,1,1,1,1,1,1,1,1,1,1,1,1,1,1,1,1,1,1,1,1,1,1,1,4),
(-0.1053316651847,1.105331665185),(-0.02,0.0125,0.045,0.0775,0.11,0.1425,
0.175,0.2075,0.24,0.2725,0.305,0.3375,0.37,0.4025,0.435,0.4675,0.5,0.5325,
0.565,0.5975,0.63,0.6625,0.695,0.7275,0.76,0.7925,0.825,0.8575,0.89,0.9225,
0.955,0.9875,1.02),.UNSPECIFIED.);
#357=B_SPLINE_SURFACE_WITH_KNOTS('',3,3,((#24997,#24998,#24999,#25000,#25001,
#25002,#25003,#25004,#25005,#25006,#25007,#25008,#25009,#25010,#25011,#25012,
#25013,#25014,#25015,#25016,#25017,#25018,#25019,#25020,#25021,#25022,#25023,
#25024,#25025,#25026,#25027,#25028,#25029,#25030,#25031),(#25032,#25033,
#25034,#25035,#25036,#25037,#25038,#25039,#25040,#25041,#25042,#25043,#25044,
#25045,#25046,#25047,#25048,#25049,#25050,#25051,#25052,#25053,#25054,#25055,
#25056,#25057,#25058,#25059,#25060,#25061,#25062,#25063,#25064,#25065,#25066),
(#25067,#25068,#25069,#25070,#25071,#25072,#25073,#25074,#25075,#25076,
#25077,#25078,#25079,#25080,#25081,#25082,#25083,#25084,#25085,#25086,#25087,
#25088,#25089,#25090,#25091,#25092,#25093,#25094,#25095,#25096,#25097,#25098,
#25099,#25100,#25101),(#25102,#25103,#25104,#25105,#25106,#25107,#25108,
#25109,#25110,#25111,#25112,#25113,#25114,#25115,#25116,#25117,#25118,#25119,
#25120,#25121,#25122,#25123,#25124,#25125,#25126,#25127,#25128,#25129,#25130,
#25131,#25132,#25133,#25134,#25135,#25136)),.UNSPECIFIED.,.F.,.F.,.F.,(4,
4),(4,1,1,1,1,1,1,1,1,1,1,1,1,1,1,1,1,1,1,1,1,1,1,1,1,1,1,1,1,1,1,1,4),
(-0.1053316651848,1.105331665185),(-0.02,0.0125,0.045,0.0775,0.11,0.1425,
0.175,0.2075,0.24,0.2725,0.305,0.3375,0.37,0.4025,0.435,0.4675,0.5,0.5325,
0.565,0.5975,0.63,0.6625,0.695,0.7275,0.76,0.7925,0.825,0.8575,0.89,0.9225,
0.955,0.9875,1.02),.UNSPECIFIED.);
#358=B_SPLINE_SURFACE_WITH_KNOTS('',3,3,((#25222,#25223,#25224,#25225,#25226,
#25227,#25228,#25229,#25230,#25231,#25232,#25233,#25234,#25235,#25236,#25237,
#25238,#25239,#25240,#25241,#25242,#25243,#25244,#25245,#25246,#25247,#25248,
#25249,#25250,#25251,#25252,#25253,#25254,#25255,#25256),(#25257,#25258,
#25259,#25260,#25261,#25262,#25263,#25264,#25265,#25266,#25267,#25268,#25269,
#25270,#25271,#25272,#25273,#25274,#25275,#25276,#25277,#25278,#25279,#25280,
#25281,#25282,#25283,#25284,#25285,#25286,#25287,#25288,#25289,#25290,#25291),
(#25292,#25293,#25294,#25295,#25296,#25297,#25298,#25299,#25300,#25301,
#25302,#25303,#25304,#25305,#25306,#25307,#25308,#25309,#25310,#25311,#25312,
#25313,#25314,#25315,#25316,#25317,#25318,#25319,#25320,#25321,#25322,#25323,
#25324,#25325,#25326),(#25327,#25328,#25329,#25330,#25331,#25332,#25333,
#25334,#25335,#25336,#25337,#25338,#25339,#25340,#25341,#25342,#25343,#25344,
#25345,#25346,#25347,#25348,#25349,#25350,#25351,#25352,#25353,#25354,#25355,
#25356,#25357,#25358,#25359,#25360,#25361)),.UNSPECIFIED.,.F.,.F.,.F.,(4,
4),(4,1,1,1,1,1,1,1,1,1,1,1,1,1,1,1,1,1,1,1,1,1,1,1,1,1,1,1,1,1,1,1,4),
(-0.2772301033111,1.277230103311),(-0.02,0.0125,0.045,0.0775,0.11,0.1425,
0.175,0.2075,0.24,0.2725,0.305,0.3375,0.37,0.4025,0.435,0.4675,0.5,0.5325,
0.565,0.5975,0.63,0.6625,0.695,0.7275,0.76,0.7925,0.825,0.8575,0.89,0.9225,
0.955,0.9875,1.02),.UNSPECIFIED.);
#359=B_SPLINE_SURFACE_WITH_KNOTS('',3,3,((#25881,#25882,#25883,#25884,#25885,
#25886,#25887,#25888,#25889,#25890,#25891,#25892,#25893,#25894,#25895,#25896,
#25897,#25898,#25899,#25900,#25901,#25902,#25903,#25904,#25905,#25906,#25907,
#25908,#25909,#25910,#25911,#25912,#25913,#25914,#25915),(#25916,#25917,
#25918,#25919,#25920,#25921,#25922,#25923,#25924,#25925,#25926,#25927,#25928,
#25929,#25930,#25931,#25932,#25933,#25934,#25935,#25936,#25937,#25938,#25939,
#25940,#25941,#25942,#25943,#25944,#25945,#25946,#25947,#25948,#25949,#25950),
(#25951,#25952,#25953,#25954,#25955,#25956,#25957,#25958,#25959,#25960,
#25961,#25962,#25963,#25964,#25965,#25966,#25967,#25968,#25969,#25970,#25971,
#25972,#25973,#25974,#25975,#25976,#25977,#25978,#25979,#25980,#25981,#25982,
#25983,#25984,#25985),(#25986,#25987,#25988,#25989,#25990,#25991,#25992,
#25993,#25994,#25995,#25996,#25997,#25998,#25999,#26000,#26001,#26002,#26003,
#26004,#26005,#26006,#26007,#26008,#26009,#26010,#26011,#26012,#26013,#26014,
#26015,#26016,#26017,#26018,#26019,#26020)),.UNSPECIFIED.,.F.,.F.,.F.,(4,
4),(4,1,1,1,1,1,1,1,1,1,1,1,1,1,1,1,1,1,1,1,1,1,1,1,1,1,1,1,1,1,1,1,4),
(-0.03619071925572,1.036190719256),(-0.02,0.0125,0.045,0.0775,0.11,0.1425,
0.175,0.2075,0.24,0.2725,0.305,0.3375,0.37,0.4025,0.435,0.4675,0.5,0.5325,
0.565,0.5975,0.63,0.6625,0.695,0.7275,0.76,0.7925,0.825,0.8575,0.89,0.9225,
0.955,0.9875,1.02),.UNSPECIFIED.);
#360=B_SPLINE_SURFACE_WITH_KNOTS('',3,3,((#26236,#26237,#26238,#26239,#26240,
#26241,#26242,#26243,#26244,#26245,#26246,#26247,#26248,#26249,#26250,#26251,
#26252,#26253,#26254,#26255,#26256,#26257,#26258,#26259,#26260,#26261,#26262,
#26263,#26264,#26265,#26266,#26267,#26268,#26269,#26270),(#26271,#26272,
#26273,#26274,#26275,#26276,#26277,#26278,#26279,#26280,#26281,#26282,#26283,
#26284,#26285,#26286,#26287,#26288,#26289,#26290,#26291,#26292,#26293,#26294,
#26295,#26296,#26297,#26298,#26299,#26300,#26301,#26302,#26303,#26304,#26305),
(#26306,#26307,#26308,#26309,#26310,#26311,#26312,#26313,#26314,#26315,
#26316,#26317,#26318,#26319,#26320,#26321,#26322,#26323,#26324,#26325,#26326,
#26327,#26328,#26329,#26330,#26331,#26332,#26333,#26334,#26335,#26336,#26337,
#26338,#26339,#26340),(#26341,#26342,#26343,#26344,#26345,#26346,#26347,
#26348,#26349,#26350,#26351,#26352,#26353,#26354,#26355,#26356,#26357,#26358,
#26359,#26360,#26361,#26362,#26363,#26364,#26365,#26366,#26367,#26368,#26369,
#26370,#26371,#26372,#26373,#26374,#26375)),.UNSPECIFIED.,.F.,.F.,.F.,(4,
4),(4,1,1,1,1,1,1,1,1,1,1,1,1,1,1,1,1,1,1,1,1,1,1,1,1,1,1,1,1,1,1,1,4),
(-0.03619071925572,1.036190719256),(0.01365127283277,0.04507905090427,0.07650682897578,
0.1079346070473,0.1393623851188,0.1707901631903,0.2022179412618,0.2336457193333,
0.2650734974048,0.2965012754763,0.3279290535478,0.3593568316193,0.3907846096908,
0.4222123877623,0.4536401658338,0.4850679439053,0.5164957219768,0.5479235000484,
0.5793512781199,0.6107790561914,0.6422068342629,0.6736346123344,0.7050623904059,
0.7364901684774,0.7679179465489,0.7993457246204,0.8307735026919,0.8622012807634,
0.8936290588349,0.9250568369064,0.9564846149779,0.9879123930494,1.019340171121),
 .UNSPECIFIED.);
#361=B_SPLINE_SURFACE_WITH_KNOTS('',3,3,((#26377,#26378,#26379,#26380,#26381,
#26382,#26383,#26384,#26385,#26386,#26387,#26388,#26389,#26390,#26391,#26392,
#26393,#26394,#26395,#26396,#26397,#26398,#26399,#26400,#26401,#26402,#26403,
#26404,#26405,#26406,#26407,#26408,#26409,#26410,#26411),(#26412,#26413,
#26414,#26415,#26416,#26417,#26418,#26419,#26420,#26421,#26422,#26423,#26424,
#26425,#26426,#26427,#26428,#26429,#26430,#26431,#26432,#26433,#26434,#26435,
#26436,#26437,#26438,#26439,#26440,#26441,#26442,#26443,#26444,#26445,#26446),
(#26447,#26448,#26449,#26450,#26451,#26452,#26453,#26454,#26455,#26456,
#26457,#26458,#26459,#26460,#26461,#26462,#26463,#26464,#26465,#26466,#26467,
#26468,#26469,#26470,#26471,#26472,#26473,#26474,#26475,#26476,#26477,#26478,
#26479,#26480,#26481),(#26482,#26483,#26484,#26485,#26486,#26487,#26488,
#26489,#26490,#26491,#26492,#26493,#26494,#26495,#26496,#26497,#26498,#26499,
#26500,#26501,#26502,#26503,#26504,#26505,#26506,#26507,#26508,#26509,#26510,
#26511,#26512,#26513,#26514,#26515,#26516)),.UNSPECIFIED.,.F.,.F.,.F.,(4,
4),(4,1,1,1,1,1,1,1,1,1,1,1,1,1,1,1,1,1,1,1,1,1,1,1,1,1,1,1,1,1,1,1,4),
(-0.03619071925572,1.036190719256),(-0.02,0.0125,0.045,0.0775,0.11,0.1425,
0.175,0.2075,0.24,0.2725,0.305,0.3375,0.37,0.4025,0.435,0.4675,0.5,0.5325,
0.565,0.5975,0.63,0.6625,0.695,0.7275,0.76,0.7925,0.825,0.8575,0.89,0.9225,
0.955,0.9875,1.02),.UNSPECIFIED.);
#362=B_SPLINE_SURFACE_WITH_KNOTS('',3,3,((#26768,#26769,#26770,#26771,#26772,
#26773,#26774,#26775,#26776,#26777,#26778,#26779,#26780,#26781,#26782,#26783,
#26784,#26785,#26786,#26787,#26788,#26789,#26790,#26791,#26792,#26793,#26794,
#26795,#26796,#26797,#26798,#26799,#26800,#26801,#26802),(#26803,#26804,
#26805,#26806,#26807,#26808,#26809,#26810,#26811,#26812,#26813,#26814,#26815,
#26816,#26817,#26818,#26819,#26820,#26821,#26822,#26823,#26824,#26825,#26826,
#26827,#26828,#26829,#26830,#26831,#26832,#26833,#26834,#26835,#26836,#26837),
(#26838,#26839,#26840,#26841,#26842,#26843,#26844,#26845,#26846,#26847,
#26848,#26849,#26850,#26851,#26852,#26853,#26854,#26855,#26856,#26857,#26858,
#26859,#26860,#26861,#26862,#26863,#26864,#26865,#26866,#26867,#26868,#26869,
#26870,#26871,#26872),(#26873,#26874,#26875,#26876,#26877,#26878,#26879,
#26880,#26881,#26882,#26883,#26884,#26885,#26886,#26887,#26888,#26889,#26890,
#26891,#26892,#26893,#26894,#26895,#26896,#26897,#26898,#26899,#26900,#26901,
#26902,#26903,#26904,#26905,#26906,#26907)),.UNSPECIFIED.,.F.,.F.,.F.,(4,
4),(4,1,1,1,1,1,1,1,1,1,1,1,1,1,1,1,1,1,1,1,1,1,1,1,1,1,1,1,1,1,1,1,4),
(-0.2772301033111,1.277230103311),(-0.02,0.0125,0.045,0.0775,0.11,0.1425,
0.175,0.2075,0.24,0.2725,0.305,0.3375,0.37,0.4025,0.435,0.4675,0.5,0.5325,
0.565,0.5975,0.63,0.6625,0.695,0.7275,0.76,0.7925,0.825,0.8575,0.89,0.9225,
0.955,0.9875,1.02),.UNSPECIFIED.);
#363=B_SPLINE_SURFACE_WITH_KNOTS('',3,3,((#27028,#27029,#27030,#27031,#27032,
#27033,#27034,#27035,#27036,#27037,#27038,#27039,#27040,#27041,#27042,#27043,
#27044,#27045,#27046,#27047,#27048,#27049,#27050,#27051,#27052,#27053,#27054,
#27055,#27056,#27057,#27058,#27059,#27060,#27061,#27062),(#27063,#27064,
#27065,#27066,#27067,#27068,#27069,#27070,#27071,#27072,#27073,#27074,#27075,
#27076,#27077,#27078,#27079,#27080,#27081,#27082,#27083,#27084,#27085,#27086,
#27087,#27088,#27089,#27090,#27091,#27092,#27093,#27094,#27095,#27096,#27097),
(#27098,#27099,#27100,#27101,#27102,#27103,#27104,#27105,#27106,#27107,
#27108,#27109,#27110,#27111,#27112,#27113,#27114,#27115,#27116,#27117,#27118,
#27119,#27120,#27121,#27122,#27123,#27124,#27125,#27126,#27127,#27128,#27129,
#27130,#27131,#27132),(#27133,#27134,#27135,#27136,#27137,#27138,#27139,
#27140,#27141,#27142,#27143,#27144,#27145,#27146,#27147,#27148,#27149,#27150,
#27151,#27152,#27153,#27154,#27155,#27156,#27157,#27158,#27159,#27160,#27161,
#27162,#27163,#27164,#27165,#27166,#27167)),.UNSPECIFIED.,.F.,.F.,.F.,(4,
4),(4,1,1,1,1,1,1,1,1,1,1,1,1,1,1,1,1,1,1,1,1,1,1,1,1,1,1,1,1,1,1,1,4),
(-0.03619071925572,1.036190719256),(-0.02,0.0125,0.045,0.0775,0.11,0.1425,
0.175,0.2075,0.24,0.2725,0.305,0.3375,0.37,0.4025,0.435,0.4675,0.5,0.5325,
0.565,0.5975,0.63,0.6625,0.695,0.7275,0.76,0.7925,0.825,0.8575,0.89,0.9225,
0.955,0.9875,1.02),.UNSPECIFIED.);
#364=B_SPLINE_SURFACE_WITH_KNOTS('',3,3,((#27212,#27213,#27214,#27215,#27216,
#27217,#27218,#27219,#27220,#27221,#27222,#27223,#27224,#27225,#27226,#27227,
#27228,#27229,#27230,#27231,#27232,#27233,#27234,#27235,#27236,#27237,#27238,
#27239,#27240,#27241,#27242,#27243,#27244,#27245,#27246),(#27247,#27248,
#27249,#27250,#27251,#27252,#27253,#27254,#27255,#27256,#27257,#27258,#27259,
#27260,#27261,#27262,#27263,#27264,#27265,#27266,#27267,#27268,#27269,#27270,
#27271,#27272,#27273,#27274,#27275,#27276,#27277,#27278,#27279,#27280,#27281),
(#27282,#27283,#27284,#27285,#27286,#27287,#27288,#27289,#27290,#27291,
#27292,#27293,#27294,#27295,#27296,#27297,#27298,#27299,#27300,#27301,#27302,
#27303,#27304,#27305,#27306,#27307,#27308,#27309,#27310,#27311,#27312,#27313,
#27314,#27315,#27316),(#27317,#27318,#27319,#27320,#27321,#27322,#27323,
#27324,#27325,#27326,#27327,#27328,#27329,#27330,#27331,#27332,#27333,#27334,
#27335,#27336,#27337,#27338,#27339,#27340,#27341,#27342,#27343,#27344,#27345,
#27346,#27347,#27348,#27349,#27350,#27351)),.UNSPECIFIED.,.F.,.F.,.F.,(4,
4),(4,1,1,1,1,1,1,1,1,1,1,1,1,1,1,1,1,1,1,1,1,1,1,1,1,1,1,1,1,1,1,1,4),
(-0.03619071925572,1.036190719256),(-0.02,0.0125,0.045,0.0775,0.11,0.1425,
0.175,0.2075,0.24,0.2725,0.305,0.3375,0.37,0.4025,0.435,0.4675,0.5,0.5325,
0.565,0.5975,0.63,0.6625,0.695,0.7275,0.76,0.7925,0.825,0.8575,0.89,0.9225,
0.955,0.9875,1.02),.UNSPECIFIED.);
#365=B_SPLINE_SURFACE_WITH_KNOTS('',3,3,((#27603,#27604,#27605,#27606,#27607,
#27608,#27609,#27610,#27611,#27612,#27613,#27614,#27615,#27616,#27617,#27618,
#27619,#27620,#27621,#27622,#27623,#27624,#27625,#27626,#27627,#27628,#27629,
#27630,#27631,#27632,#27633,#27634,#27635,#27636,#27637),(#27638,#27639,
#27640,#27641,#27642,#27643,#27644,#27645,#27646,#27647,#27648,#27649,#27650,
#27651,#27652,#27653,#27654,#27655,#27656,#27657,#27658,#27659,#27660,#27661,
#27662,#27663,#27664,#27665,#27666,#27667,#27668,#27669,#27670,#27671,#27672),
(#27673,#27674,#27675,#27676,#27677,#27678,#27679,#27680,#27681,#27682,
#27683,#27684,#27685,#27686,#27687,#27688,#27689,#27690,#27691,#27692,#27693,
#27694,#27695,#27696,#27697,#27698,#27699,#27700,#27701,#27702,#27703,#27704,
#27705,#27706,#27707),(#27708,#27709,#27710,#27711,#27712,#27713,#27714,
#27715,#27716,#27717,#27718,#27719,#27720,#27721,#27722,#27723,#27724,#27725,
#27726,#27727,#27728,#27729,#27730,#27731,#27732,#27733,#27734,#27735,#27736,
#27737,#27738,#27739,#27740,#27741,#27742)),.UNSPECIFIED.,.F.,.F.,.F.,(4,
4),(4,1,1,1,1,1,1,1,1,1,1,1,1,1,1,1,1,1,1,1,1,1,1,1,1,1,1,1,1,1,1,1,4),
(-0.2772301033111,1.277230103311),(-0.02,0.0125,0.045,0.0775,0.11,0.1425,
0.175,0.2075,0.24,0.2725,0.305,0.3375,0.37,0.4025,0.435,0.4675,0.5,0.5325,
0.565,0.5975,0.63,0.6625,0.695,0.7275,0.76,0.7925,0.825,0.8575,0.89,0.9225,
0.955,0.9875,1.02),.UNSPECIFIED.);
#366=B_SPLINE_SURFACE_WITH_KNOTS('',3,3,((#27863,#27864,#27865,#27866,#27867,
#27868,#27869,#27870,#27871,#27872,#27873,#27874,#27875,#27876,#27877,#27878,
#27879,#27880,#27881,#27882,#27883,#27884,#27885,#27886,#27887,#27888,#27889,
#27890,#27891,#27892,#27893,#27894,#27895,#27896,#27897),(#27898,#27899,
#27900,#27901,#27902,#27903,#27904,#27905,#27906,#27907,#27908,#27909,#27910,
#27911,#27912,#27913,#27914,#27915,#27916,#27917,#27918,#27919,#27920,#27921,
#27922,#27923,#27924,#27925,#27926,#27927,#27928,#27929,#27930,#27931,#27932),
(#27933,#27934,#27935,#27936,#27937,#27938,#27939,#27940,#27941,#27942,
#27943,#27944,#27945,#27946,#27947,#27948,#27949,#27950,#27951,#27952,#27953,
#27954,#27955,#27956,#27957,#27958,#27959,#27960,#27961,#27962,#27963,#27964,
#27965,#27966,#27967),(#27968,#27969,#27970,#27971,#27972,#27973,#27974,
#27975,#27976,#27977,#27978,#27979,#27980,#27981,#27982,#27983,#27984,#27985,
#27986,#27987,#27988,#27989,#27990,#27991,#27992,#27993,#27994,#27995,#27996,
#27997,#27998,#27999,#28000,#28001,#28002)),.UNSPECIFIED.,.F.,.F.,.F.,(4,
4),(4,1,1,1,1,1,1,1,1,1,1,1,1,1,1,1,1,1,1,1,1,1,1,1,1,1,1,1,1,1,1,1,4),
(-0.03619071925572,1.036190719256),(-0.02,0.0125,0.045,0.0775,0.11,0.1425,
0.175,0.2075,0.24,0.2725,0.305,0.3375,0.37,0.4025,0.435,0.4675,0.5,0.5325,
0.565,0.5975,0.63,0.6625,0.695,0.7275,0.76,0.7925,0.825,0.8575,0.89,0.9225,
0.955,0.9875,1.02),.UNSPECIFIED.);
#367=B_SPLINE_SURFACE_WITH_KNOTS('',3,3,((#28047,#28048,#28049,#28050,#28051,
#28052,#28053,#28054,#28055,#28056,#28057,#28058,#28059,#28060,#28061,#28062,
#28063,#28064,#28065,#28066,#28067,#28068,#28069,#28070,#28071,#28072,#28073,
#28074,#28075,#28076,#28077,#28078,#28079,#28080,#28081),(#28082,#28083,
#28084,#28085,#28086,#28087,#28088,#28089,#28090,#28091,#28092,#28093,#28094,
#28095,#28096,#28097,#28098,#28099,#28100,#28101,#28102,#28103,#28104,#28105,
#28106,#28107,#28108,#28109,#28110,#28111,#28112,#28113,#28114,#28115,#28116),
(#28117,#28118,#28119,#28120,#28121,#28122,#28123,#28124,#28125,#28126,
#28127,#28128,#28129,#28130,#28131,#28132,#28133,#28134,#28135,#28136,#28137,
#28138,#28139,#28140,#28141,#28142,#28143,#28144,#28145,#28146,#28147,#28148,
#28149,#28150,#28151),(#28152,#28153,#28154,#28155,#28156,#28157,#28158,
#28159,#28160,#28161,#28162,#28163,#28164,#28165,#28166,#28167,#28168,#28169,
#28170,#28171,#28172,#28173,#28174,#28175,#28176,#28177,#28178,#28179,#28180,
#28181,#28182,#28183,#28184,#28185,#28186)),.UNSPECIFIED.,.F.,.F.,.F.,(4,
4),(4,1,1,1,1,1,1,1,1,1,1,1,1,1,1,1,1,1,1,1,1,1,1,1,1,1,1,1,1,1,1,1,4),
(-0.03619071925572,1.036190719256),(-0.02,0.0125,0.045,0.0775,0.11,0.1425,
0.175,0.2075,0.24,0.2725,0.305,0.3375,0.37,0.4025,0.435,0.4675,0.5,0.5325,
0.565,0.5975,0.63,0.6625,0.695,0.7275,0.76,0.7925,0.825,0.8575,0.89,0.9225,
0.955,0.9875,1.02),.UNSPECIFIED.);
#368=B_SPLINE_SURFACE_WITH_KNOTS('',3,3,((#28449,#28450,#28451,#28452,#28453,
#28454,#28455,#28456,#28457,#28458,#28459,#28460,#28461,#28462,#28463,#28464,
#28465,#28466,#28467,#28468,#28469,#28470,#28471,#28472,#28473,#28474,#28475,
#28476,#28477,#28478,#28479,#28480,#28481,#28482,#28483),(#28484,#28485,
#28486,#28487,#28488,#28489,#28490,#28491,#28492,#28493,#28494,#28495,#28496,
#28497,#28498,#28499,#28500,#28501,#28502,#28503,#28504,#28505,#28506,#28507,
#28508,#28509,#28510,#28511,#28512,#28513,#28514,#28515,#28516,#28517,#28518),
(#28519,#28520,#28521,#28522,#28523,#28524,#28525,#28526,#28527,#28528,
#28529,#28530,#28531,#28532,#28533,#28534,#28535,#28536,#28537,#28538,#28539,
#28540,#28541,#28542,#28543,#28544,#28545,#28546,#28547,#28548,#28549,#28550,
#28551,#28552,#28553),(#28554,#28555,#28556,#28557,#28558,#28559,#28560,
#28561,#28562,#28563,#28564,#28565,#28566,#28567,#28568,#28569,#28570,#28571,
#28572,#28573,#28574,#28575,#28576,#28577,#28578,#28579,#28580,#28581,#28582,
#28583,#28584,#28585,#28586,#28587,#28588)),.UNSPECIFIED.,.F.,.F.,.F.,(4,
4),(4,1,1,1,1,1,1,1,1,1,1,1,1,1,1,1,1,1,1,1,1,1,1,1,1,1,1,1,1,1,1,1,4),
(-0.03619071925572,1.036190719256),(-0.02,0.0125,0.045,0.0775,0.11,0.1425,
0.175,0.2075,0.24,0.2725,0.305,0.3375,0.37,0.4025,0.435,0.4675,0.5,0.5325,
0.565,0.5975,0.63,0.6625,0.695,0.7275,0.76,0.7925,0.825,0.8575,0.89,0.9225,
0.955,0.9875,1.02),.UNSPECIFIED.);
#369=B_SPLINE_SURFACE_WITH_KNOTS('',3,3,((#28780,#28781,#28782,#28783,#28784,
#28785,#28786,#28787,#28788,#28789,#28790,#28791,#28792,#28793,#28794,#28795,
#28796,#28797,#28798,#28799,#28800,#28801,#28802,#28803,#28804,#28805,#28806,
#28807,#28808,#28809,#28810,#28811,#28812,#28813,#28814),(#28815,#28816,
#28817,#28818,#28819,#28820,#28821,#28822,#28823,#28824,#28825,#28826,#28827,
#28828,#28829,#28830,#28831,#28832,#28833,#28834,#28835,#28836,#28837,#28838,
#28839,#28840,#28841,#28842,#28843,#28844,#28845,#28846,#28847,#28848,#28849),
(#28850,#28851,#28852,#28853,#28854,#28855,#28856,#28857,#28858,#28859,
#28860,#28861,#28862,#28863,#28864,#28865,#28866,#28867,#28868,#28869,#28870,
#28871,#28872,#28873,#28874,#28875,#28876,#28877,#28878,#28879,#28880,#28881,
#28882,#28883,#28884),(#28885,#28886,#28887,#28888,#28889,#28890,#28891,
#28892,#28893,#28894,#28895,#28896,#28897,#28898,#28899,#28900,#28901,#28902,
#28903,#28904,#28905,#28906,#28907,#28908,#28909,#28910,#28911,#28912,#28913,
#28914,#28915,#28916,#28917,#28918,#28919)),.UNSPECIFIED.,.F.,.F.,.F.,(4,
4),(4,1,1,1,1,1,1,1,1,1,1,1,1,1,1,1,1,1,1,1,1,1,1,1,1,1,1,1,1,1,1,1,4),
(-0.2772301033111,1.277230103311),(-0.02,0.0125,0.045,0.0775,0.11,0.1425,
0.175,0.2075,0.24,0.2725,0.305,0.3375,0.37,0.4025,0.435,0.4675,0.5,0.5325,
0.565,0.5975,0.63,0.6625,0.695,0.7275,0.76,0.7925,0.825,0.8575,0.89,0.9225,
0.955,0.9875,1.02),.UNSPECIFIED.);
#370=B_SPLINE_SURFACE_WITH_KNOTS('',3,3,((#34681,#34682,#34683,#34684,#34685,
#34686,#34687,#34688,#34689,#34690,#34691,#34692,#34693,#34694,#34695,#34696,
#34697,#34698,#34699,#34700,#34701,#34702,#34703,#34704,#34705,#34706,#34707,
#34708,#34709,#34710,#34711,#34712,#34713,#34714,#34715),(#34716,#34717,
#34718,#34719,#34720,#34721,#34722,#34723,#34724,#34725,#34726,#34727,#34728,
#34729,#34730,#34731,#34732,#34733,#34734,#34735,#34736,#34737,#34738,#34739,
#34740,#34741,#34742,#34743,#34744,#34745,#34746,#34747,#34748,#34749,#34750),
(#34751,#34752,#34753,#34754,#34755,#34756,#34757,#34758,#34759,#34760,
#34761,#34762,#34763,#34764,#34765,#34766,#34767,#34768,#34769,#34770,#34771,
#34772,#34773,#34774,#34775,#34776,#34777,#34778,#34779,#34780,#34781,#34782,
#34783,#34784,#34785),(#34786,#34787,#34788,#34789,#34790,#34791,#34792,
#34793,#34794,#34795,#34796,#34797,#34798,#34799,#34800,#34801,#34802,#34803,
#34804,#34805,#34806,#34807,#34808,#34809,#34810,#34811,#34812,#34813,#34814,
#34815,#34816,#34817,#34818,#34819,#34820)),.UNSPECIFIED.,.F.,.F.,.F.,(4,
4),(4,1,1,1,1,1,1,1,1,1,1,1,1,1,1,1,1,1,1,1,1,1,1,1,1,1,1,1,1,1,1,1,4),
(-0.05164332951995,1.05164332952),(-0.02,0.0125,0.045,0.0775,0.11,0.1425,
0.175,0.2075,0.24,0.2725,0.305,0.3375,0.37,0.4025,0.435,0.4675,0.5,0.5325,
0.565,0.5975,0.63,0.6625,0.695,0.7275,0.76,0.7925,0.825,0.8575,0.89,0.9225,
0.955,0.9875,1.02),.UNSPECIFIED.);
#371=B_SPLINE_SURFACE_WITH_KNOTS('',3,3,((#35063,#35064,#35065,#35066,#35067,
#35068,#35069,#35070,#35071,#35072,#35073,#35074,#35075,#35076,#35077,#35078,
#35079,#35080,#35081,#35082,#35083,#35084,#35085,#35086,#35087,#35088,#35089,
#35090,#35091,#35092,#35093,#35094,#35095,#35096,#35097),(#35098,#35099,
#35100,#35101,#35102,#35103,#35104,#35105,#35106,#35107,#35108,#35109,#35110,
#35111,#35112,#35113,#35114,#35115,#35116,#35117,#35118,#35119,#35120,#35121,
#35122,#35123,#35124,#35125,#35126,#35127,#35128,#35129,#35130,#35131,#35132),
(#35133,#35134,#35135,#35136,#35137,#35138,#35139,#35140,#35141,#35142,
#35143,#35144,#35145,#35146,#35147,#35148,#35149,#35150,#35151,#35152,#35153,
#35154,#35155,#35156,#35157,#35158,#35159,#35160,#35161,#35162,#35163,#35164,
#35165,#35166,#35167),(#35168,#35169,#35170,#35171,#35172,#35173,#35174,
#35175,#35176,#35177,#35178,#35179,#35180,#35181,#35182,#35183,#35184,#35185,
#35186,#35187,#35188,#35189,#35190,#35191,#35192,#35193,#35194,#35195,#35196,
#35197,#35198,#35199,#35200,#35201,#35202)),.UNSPECIFIED.,.F.,.F.,.F.,(4,
4),(4,1,1,1,1,1,1,1,1,1,1,1,1,1,1,1,1,1,1,1,1,1,1,1,1,1,1,1,1,1,1,1,4),
(-0.05164332951996,1.05164332952),(-0.02,0.0125,0.045,0.0775,0.11,0.1425,
0.175,0.2075,0.24,0.2725,0.305,0.3375,0.37,0.4025,0.435,0.4675,0.5,0.5325,
0.565,0.5975,0.63,0.6625,0.695,0.7275,0.76,0.7925,0.825,0.8575,0.89,0.9225,
0.955,0.9875,1.02),.UNSPECIFIED.);
#372=B_SPLINE_SURFACE_WITH_KNOTS('',3,3,((#35371,#35372,#35373,#35374,#35375,
#35376,#35377,#35378,#35379,#35380,#35381,#35382,#35383,#35384,#35385,#35386,
#35387,#35388,#35389,#35390,#35391,#35392,#35393,#35394,#35395,#35396,#35397,
#35398,#35399,#35400,#35401,#35402,#35403,#35404,#35405),(#35406,#35407,
#35408,#35409,#35410,#35411,#35412,#35413,#35414,#35415,#35416,#35417,#35418,
#35419,#35420,#35421,#35422,#35423,#35424,#35425,#35426,#35427,#35428,#35429,
#35430,#35431,#35432,#35433,#35434,#35435,#35436,#35437,#35438,#35439,#35440),
(#35441,#35442,#35443,#35444,#35445,#35446,#35447,#35448,#35449,#35450,
#35451,#35452,#35453,#35454,#35455,#35456,#35457,#35458,#35459,#35460,#35461,
#35462,#35463,#35464,#35465,#35466,#35467,#35468,#35469,#35470,#35471,#35472,
#35473,#35474,#35475),(#35476,#35477,#35478,#35479,#35480,#35481,#35482,
#35483,#35484,#35485,#35486,#35487,#35488,#35489,#35490,#35491,#35492,#35493,
#35494,#35495,#35496,#35497,#35498,#35499,#35500,#35501,#35502,#35503,#35504,
#35505,#35506,#35507,#35508,#35509,#35510)),.UNSPECIFIED.,.F.,.F.,.F.,(4,
4),(4,1,1,1,1,1,1,1,1,1,1,1,1,1,1,1,1,1,1,1,1,1,1,1,1,1,1,1,1,1,1,1,4),
(-0.05164332951995,1.05164332952),(-0.02,0.0125,0.045,0.0775,0.11,0.1425,
0.175,0.2075,0.24,0.2725,0.305,0.3375,0.37,0.4025,0.435,0.4675,0.5,0.5325,
0.565,0.5975,0.63,0.6625,0.695,0.7275,0.76,0.7925,0.825,0.8575,0.89,0.9225,
0.955,0.9875,1.02),.UNSPECIFIED.);
#373=B_SPLINE_SURFACE_WITH_KNOTS('',3,3,((#35746,#35747,#35748,#35749,#35750,
#35751,#35752,#35753,#35754,#35755,#35756,#35757,#35758,#35759,#35760,#35761,
#35762,#35763,#35764,#35765,#35766,#35767,#35768,#35769,#35770,#35771,#35772,
#35773,#35774,#35775,#35776,#35777,#35778,#35779,#35780),(#35781,#35782,
#35783,#35784,#35785,#35786,#35787,#35788,#35789,#35790,#35791,#35792,#35793,
#35794,#35795,#35796,#35797,#35798,#35799,#35800,#35801,#35802,#35803,#35804,
#35805,#35806,#35807,#35808,#35809,#35810,#35811,#35812,#35813,#35814,#35815),
(#35816,#35817,#35818,#35819,#35820,#35821,#35822,#35823,#35824,#35825,
#35826,#35827,#35828,#35829,#35830,#35831,#35832,#35833,#35834,#35835,#35836,
#35837,#35838,#35839,#35840,#35841,#35842,#35843,#35844,#35845,#35846,#35847,
#35848,#35849,#35850),(#35851,#35852,#35853,#35854,#35855,#35856,#35857,
#35858,#35859,#35860,#35861,#35862,#35863,#35864,#35865,#35866,#35867,#35868,
#35869,#35870,#35871,#35872,#35873,#35874,#35875,#35876,#35877,#35878,#35879,
#35880,#35881,#35882,#35883,#35884,#35885)),.UNSPECIFIED.,.F.,.F.,.F.,(4,
4),(4,1,1,1,1,1,1,1,1,1,1,1,1,1,1,1,1,1,1,1,1,1,1,1,1,1,1,1,1,1,1,1,4),
(-0.05164332951996,1.05164332952),(-0.02,0.0125,0.045,0.0775,0.11,0.1425,
0.175,0.2075,0.24,0.2725,0.305,0.3375,0.37,0.4025,0.435,0.4675,0.5,0.5325,
0.565,0.5975,0.63,0.6625,0.695,0.7275,0.76,0.7925,0.825,0.8575,0.89,0.9225,
0.955,0.9875,1.02),.UNSPECIFIED.);
#374=B_SPLINE_SURFACE_WITH_KNOTS('',3,3,((#36047,#36048,#36049,#36050,#36051,
#36052,#36053,#36054,#36055,#36056,#36057,#36058,#36059,#36060,#36061,#36062,
#36063,#36064,#36065,#36066,#36067,#36068,#36069,#36070,#36071,#36072,#36073,
#36074,#36075,#36076,#36077,#36078,#36079,#36080,#36081),(#36082,#36083,
#36084,#36085,#36086,#36087,#36088,#36089,#36090,#36091,#36092,#36093,#36094,
#36095,#36096,#36097,#36098,#36099,#36100,#36101,#36102,#36103,#36104,#36105,
#36106,#36107,#36108,#36109,#36110,#36111,#36112,#36113,#36114,#36115,#36116),
(#36117,#36118,#36119,#36120,#36121,#36122,#36123,#36124,#36125,#36126,
#36127,#36128,#36129,#36130,#36131,#36132,#36133,#36134,#36135,#36136,#36137,
#36138,#36139,#36140,#36141,#36142,#36143,#36144,#36145,#36146,#36147,#36148,
#36149,#36150,#36151),(#36152,#36153,#36154,#36155,#36156,#36157,#36158,
#36159,#36160,#36161,#36162,#36163,#36164,#36165,#36166,#36167,#36168,#36169,
#36170,#36171,#36172,#36173,#36174,#36175,#36176,#36177,#36178,#36179,#36180,
#36181,#36182,#36183,#36184,#36185,#36186)),.UNSPECIFIED.,.F.,.F.,.F.,(4,
4),(4,1,1,1,1,1,1,1,1,1,1,1,1,1,1,1,1,1,1,1,1,1,1,1,1,1,1,1,1,1,1,1,4),
(-0.05164332951995,1.05164332952),(-0.02,0.0125,0.045,0.0775,0.11,0.1425,
0.175,0.2075,0.24,0.2725,0.305,0.3375,0.37,0.4025,0.435,0.4675,0.5,0.5325,
0.565,0.5975,0.63,0.6625,0.695,0.7275,0.76,0.7925,0.825,0.8575,0.89,0.9225,
0.955,0.9875,1.02),.UNSPECIFIED.);
#375=B_SPLINE_SURFACE_WITH_KNOTS('',3,3,((#36420,#36421,#36422,#36423,#36424,
#36425,#36426,#36427,#36428,#36429,#36430,#36431,#36432,#36433,#36434,#36435,
#36436,#36437,#36438,#36439,#36440,#36441,#36442,#36443,#36444,#36445,#36446,
#36447,#36448,#36449,#36450,#36451,#36452,#36453,#36454),(#36455,#36456,
#36457,#36458,#36459,#36460,#36461,#36462,#36463,#36464,#36465,#36466,#36467,
#36468,#36469,#36470,#36471,#36472,#36473,#36474,#36475,#36476,#36477,#36478,
#36479,#36480,#36481,#36482,#36483,#36484,#36485,#36486,#36487,#36488,#36489),
(#36490,#36491,#36492,#36493,#36494,#36495,#36496,#36497,#36498,#36499,
#36500,#36501,#36502,#36503,#36504,#36505,#36506,#36507,#36508,#36509,#36510,
#36511,#36512,#36513,#36514,#36515,#36516,#36517,#36518,#36519,#36520,#36521,
#36522,#36523,#36524),(#36525,#36526,#36527,#36528,#36529,#36530,#36531,
#36532,#36533,#36534,#36535,#36536,#36537,#36538,#36539,#36540,#36541,#36542,
#36543,#36544,#36545,#36546,#36547,#36548,#36549,#36550,#36551,#36552,#36553,
#36554,#36555,#36556,#36557,#36558,#36559)),.UNSPECIFIED.,.F.,.F.,.F.,(4,
4),(4,1,1,1,1,1,1,1,1,1,1,1,1,1,1,1,1,1,1,1,1,1,1,1,1,1,1,1,1,1,1,1,4),
(-0.05164332951996,1.05164332952),(-0.02,0.0125,0.045,0.0775,0.11,0.1425,
0.175,0.2075,0.24,0.2725,0.305,0.3375,0.37,0.4025,0.435,0.4675,0.5,0.5325,
0.565,0.5975,0.63,0.6625,0.695,0.7275,0.76,0.7925,0.825,0.8575,0.89,0.9225,
0.955,0.9875,1.02),.UNSPECIFIED.);
#376=B_SPLINE_SURFACE_WITH_KNOTS('',3,3,((#36721,#36722,#36723,#36724,#36725,
#36726,#36727,#36728,#36729,#36730,#36731,#36732,#36733,#36734,#36735,#36736,
#36737,#36738,#36739,#36740,#36741,#36742,#36743,#36744,#36745,#36746,#36747,
#36748,#36749,#36750,#36751,#36752,#36753,#36754,#36755),(#36756,#36757,
#36758,#36759,#36760,#36761,#36762,#36763,#36764,#36765,#36766,#36767,#36768,
#36769,#36770,#36771,#36772,#36773,#36774,#36775,#36776,#36777,#36778,#36779,
#36780,#36781,#36782,#36783,#36784,#36785,#36786,#36787,#36788,#36789,#36790),
(#36791,#36792,#36793,#36794,#36795,#36796,#36797,#36798,#36799,#36800,
#36801,#36802,#36803,#36804,#36805,#36806,#36807,#36808,#36809,#36810,#36811,
#36812,#36813,#36814,#36815,#36816,#36817,#36818,#36819,#36820,#36821,#36822,
#36823,#36824,#36825),(#36826,#36827,#36828,#36829,#36830,#36831,#36832,
#36833,#36834,#36835,#36836,#36837,#36838,#36839,#36840,#36841,#36842,#36843,
#36844,#36845,#36846,#36847,#36848,#36849,#36850,#36851,#36852,#36853,#36854,
#36855,#36856,#36857,#36858,#36859,#36860)),.UNSPECIFIED.,.F.,.F.,.F.,(4,
4),(4,1,1,1,1,1,1,1,1,1,1,1,1,1,1,1,1,1,1,1,1,1,1,1,1,1,1,1,1,1,1,1,4),
(-0.05164332951995,1.05164332952),(-0.02,0.0125,0.045,0.0775,0.11,0.1425,
0.175,0.2075,0.24,0.2725,0.305,0.3375,0.37,0.4025,0.435,0.4675,0.5,0.5325,
0.565,0.5975,0.63,0.6625,0.695,0.7275,0.76,0.7925,0.825,0.8575,0.89,0.9225,
0.955,0.9875,1.02),.UNSPECIFIED.);
#377=B_SPLINE_SURFACE_WITH_KNOTS('',3,3,((#37098,#37099,#37100,#37101,#37102,
#37103,#37104,#37105,#37106,#37107,#37108,#37109,#37110,#37111,#37112,#37113,
#37114,#37115,#37116,#37117,#37118,#37119,#37120,#37121,#37122,#37123,#37124,
#37125,#37126,#37127,#37128,#37129,#37130,#37131,#37132),(#37133,#37134,
#37135,#37136,#37137,#37138,#37139,#37140,#37141,#37142,#37143,#37144,#37145,
#37146,#37147,#37148,#37149,#37150,#37151,#37152,#37153,#37154,#37155,#37156,
#37157,#37158,#37159,#37160,#37161,#37162,#37163,#37164,#37165,#37166,#37167),
(#37168,#37169,#37170,#37171,#37172,#37173,#37174,#37175,#37176,#37177,
#37178,#37179,#37180,#37181,#37182,#37183,#37184,#37185,#37186,#37187,#37188,
#37189,#37190,#37191,#37192,#37193,#37194,#37195,#37196,#37197,#37198,#37199,
#37200,#37201,#37202),(#37203,#37204,#37205,#37206,#37207,#37208,#37209,
#37210,#37211,#37212,#37213,#37214,#37215,#37216,#37217,#37218,#37219,#37220,
#37221,#37222,#37223,#37224,#37225,#37226,#37227,#37228,#37229,#37230,#37231,
#37232,#37233,#37234,#37235,#37236,#37237)),.UNSPECIFIED.,.F.,.F.,.F.,(4,
4),(4,1,1,1,1,1,1,1,1,1,1,1,1,1,1,1,1,1,1,1,1,1,1,1,1,1,1,1,1,1,1,1,4),
(-0.05164332951996,1.05164332952),(-0.02,0.0125,0.045,0.0775,0.11,0.1425,
0.175,0.2075,0.24,0.2725,0.305,0.3375,0.37,0.4025,0.435,0.4675,0.5,0.5325,
0.565,0.5975,0.63,0.6625,0.695,0.7275,0.76,0.7925,0.825,0.8575,0.89,0.9225,
0.955,0.9875,1.02),.UNSPECIFIED.);
#378=B_SPLINE_SURFACE_WITH_KNOTS('',3,3,((#37401,#37402,#37403,#37404,#37405,
#37406,#37407,#37408,#37409,#37410,#37411,#37412,#37413,#37414,#37415,#37416,
#37417,#37418,#37419,#37420,#37421,#37422,#37423,#37424,#37425,#37426,#37427,
#37428,#37429,#37430,#37431,#37432,#37433,#37434,#37435),(#37436,#37437,
#37438,#37439,#37440,#37441,#37442,#37443,#37444,#37445,#37446,#37447,#37448,
#37449,#37450,#37451,#37452,#37453,#37454,#37455,#37456,#37457,#37458,#37459,
#37460,#37461,#37462,#37463,#37464,#37465,#37466,#37467,#37468,#37469,#37470),
(#37471,#37472,#37473,#37474,#37475,#37476,#37477,#37478,#37479,#37480,
#37481,#37482,#37483,#37484,#37485,#37486,#37487,#37488,#37489,#37490,#37491,
#37492,#37493,#37494,#37495,#37496,#37497,#37498,#37499,#37500,#37501,#37502,
#37503,#37504,#37505),(#37506,#37507,#37508,#37509,#37510,#37511,#37512,
#37513,#37514,#37515,#37516,#37517,#37518,#37519,#37520,#37521,#37522,#37523,
#37524,#37525,#37526,#37527,#37528,#37529,#37530,#37531,#37532,#37533,#37534,
#37535,#37536,#37537,#37538,#37539,#37540)),.UNSPECIFIED.,.F.,.F.,.F.,(4,
4),(4,1,1,1,1,1,1,1,1,1,1,1,1,1,1,1,1,1,1,1,1,1,1,1,1,1,1,1,1,1,1,1,4),
(-0.05164332951995,1.05164332952),(-0.02,0.0125,0.045,0.0775,0.11,0.1425,
0.175,0.2075,0.24,0.2725,0.305,0.3375,0.37,0.4025,0.435,0.4675,0.5,0.5325,
0.565,0.5975,0.63,0.6625,0.695,0.7275,0.76,0.7925,0.825,0.8575,0.89,0.9225,
0.955,0.9875,1.02),.UNSPECIFIED.);
#379=B_SPLINE_SURFACE_WITH_KNOTS('',3,3,((#37772,#37773,#37774,#37775,#37776,
#37777,#37778,#37779,#37780,#37781,#37782,#37783,#37784,#37785,#37786,#37787,
#37788,#37789,#37790,#37791,#37792,#37793,#37794,#37795,#37796,#37797,#37798,
#37799,#37800,#37801,#37802,#37803,#37804,#37805,#37806),(#37807,#37808,
#37809,#37810,#37811,#37812,#37813,#37814,#37815,#37816,#37817,#37818,#37819,
#37820,#37821,#37822,#37823,#37824,#37825,#37826,#37827,#37828,#37829,#37830,
#37831,#37832,#37833,#37834,#37835,#37836,#37837,#37838,#37839,#37840,#37841),
(#37842,#37843,#37844,#37845,#37846,#37847,#37848,#37849,#37850,#37851,
#37852,#37853,#37854,#37855,#37856,#37857,#37858,#37859,#37860,#37861,#37862,
#37863,#37864,#37865,#37866,#37867,#37868,#37869,#37870,#37871,#37872,#37873,
#37874,#37875,#37876),(#37877,#37878,#37879,#37880,#37881,#37882,#37883,
#37884,#37885,#37886,#37887,#37888,#37889,#37890,#37891,#37892,#37893,#37894,
#37895,#37896,#37897,#37898,#37899,#37900,#37901,#37902,#37903,#37904,#37905,
#37906,#37907,#37908,#37909,#37910,#37911)),.UNSPECIFIED.,.F.,.F.,.F.,(4,
4),(4,1,1,1,1,1,1,1,1,1,1,1,1,1,1,1,1,1,1,1,1,1,1,1,1,1,1,1,1,1,1,1,4),
(-0.05164332951996,1.05164332952),(-0.02,0.0125,0.045,0.0775,0.11,0.1425,
0.175,0.2075,0.24,0.2725,0.305,0.3375,0.37,0.4025,0.435,0.4675,0.5,0.5325,
0.565,0.5975,0.63,0.6625,0.695,0.7275,0.76,0.7925,0.825,0.8575,0.89,0.9225,
0.955,0.9875,1.02),.UNSPECIFIED.);
#380=B_SPLINE_SURFACE_WITH_KNOTS('',3,3,((#38073,#38074,#38075,#38076,#38077,
#38078,#38079,#38080,#38081,#38082,#38083,#38084,#38085,#38086,#38087,#38088,
#38089,#38090,#38091,#38092,#38093,#38094,#38095,#38096,#38097,#38098,#38099,
#38100,#38101,#38102,#38103,#38104,#38105,#38106,#38107),(#38108,#38109,
#38110,#38111,#38112,#38113,#38114,#38115,#38116,#38117,#38118,#38119,#38120,
#38121,#38122,#38123,#38124,#38125,#38126,#38127,#38128,#38129,#38130,#38131,
#38132,#38133,#38134,#38135,#38136,#38137,#38138,#38139,#38140,#38141,#38142),
(#38143,#38144,#38145,#38146,#38147,#38148,#38149,#38150,#38151,#38152,
#38153,#38154,#38155,#38156,#38157,#38158,#38159,#38160,#38161,#38162,#38163,
#38164,#38165,#38166,#38167,#38168,#38169,#38170,#38171,#38172,#38173,#38174,
#38175,#38176,#38177),(#38178,#38179,#38180,#38181,#38182,#38183,#38184,
#38185,#38186,#38187,#38188,#38189,#38190,#38191,#38192,#38193,#38194,#38195,
#38196,#38197,#38198,#38199,#38200,#38201,#38202,#38203,#38204,#38205,#38206,
#38207,#38208,#38209,#38210,#38211,#38212)),.UNSPECIFIED.,.F.,.F.,.F.,(4,
4),(4,1,1,1,1,1,1,1,1,1,1,1,1,1,1,1,1,1,1,1,1,1,1,1,1,1,1,1,1,1,1,1,4),
(-0.05164332951995,1.05164332952),(-0.02,0.0125,0.045,0.0775,0.11,0.1425,
0.175,0.2075,0.24,0.2725,0.305,0.3375,0.37,0.4025,0.435,0.4675,0.5,0.5325,
0.565,0.5975,0.63,0.6625,0.695,0.7275,0.76,0.7925,0.825,0.8575,0.89,0.9225,
0.955,0.9875,1.02),.UNSPECIFIED.);
#381=B_SPLINE_SURFACE_WITH_KNOTS('',3,3,((#38552,#38553,#38554,#38555,#38556,
#38557,#38558,#38559,#38560,#38561,#38562,#38563,#38564,#38565,#38566,#38567,
#38568,#38569,#38570,#38571,#38572,#38573,#38574,#38575,#38576,#38577,#38578,
#38579,#38580,#38581,#38582,#38583,#38584,#38585,#38586),(#38587,#38588,
#38589,#38590,#38591,#38592,#38593,#38594,#38595,#38596,#38597,#38598,#38599,
#38600,#38601,#38602,#38603,#38604,#38605,#38606,#38607,#38608,#38609,#38610,
#38611,#38612,#38613,#38614,#38615,#38616,#38617,#38618,#38619,#38620,#38621),
(#38622,#38623,#38624,#38625,#38626,#38627,#38628,#38629,#38630,#38631,
#38632,#38633,#38634,#38635,#38636,#38637,#38638,#38639,#38640,#38641,#38642,
#38643,#38644,#38645,#38646,#38647,#38648,#38649,#38650,#38651,#38652,#38653,
#38654,#38655,#38656),(#38657,#38658,#38659,#38660,#38661,#38662,#38663,
#38664,#38665,#38666,#38667,#38668,#38669,#38670,#38671,#38672,#38673,#38674,
#38675,#38676,#38677,#38678,#38679,#38680,#38681,#38682,#38683,#38684,#38685,
#38686,#38687,#38688,#38689,#38690,#38691)),.UNSPECIFIED.,.F.,.F.,.F.,(4,
4),(4,1,1,1,1,1,1,1,1,1,1,1,1,1,1,1,1,1,1,1,1,1,1,1,1,1,1,1,1,1,1,1,4),
(-0.05164332951995,1.05164332952),(0.1685302411052,0.1950231500896,0.221516059074,
0.2480089680584,0.2745018770427,0.3009947860271,0.3274876950115,0.3539806039959,
0.3804735129803,0.4069664219647,0.4334593309491,0.4599522399335,0.4864451489179,
0.5129380579023,0.5394309668867,0.5659238758711,0.5924167848555,0.6189096938399,
0.6454026028243,0.6718955118087,0.6983884207931,0.7248813297774,0.7513742387618,
0.7778671477462,0.8043600567306,0.830852965715,0.8573458746994,0.8838387836838,
0.9103316926682,0.9368246016526,0.963317510637,0.9898104196214,1.016303328606),
 .UNSPECIFIED.);
#382=B_SPLINE_SURFACE_WITH_KNOTS('',3,3,((#38949,#38950,#38951,#38952,#38953,
#38954,#38955,#38956,#38957,#38958,#38959,#38960,#38961,#38962,#38963,#38964,
#38965,#38966,#38967,#38968,#38969,#38970,#38971,#38972,#38973,#38974,#38975,
#38976,#38977,#38978,#38979,#38980,#38981,#38982,#38983),(#38984,#38985,
#38986,#38987,#38988,#38989,#38990,#38991,#38992,#38993,#38994,#38995,#38996,
#38997,#38998,#38999,#39000,#39001,#39002,#39003,#39004,#39005,#39006,#39007,
#39008,#39009,#39010,#39011,#39012,#39013,#39014,#39015,#39016,#39017,#39018),
(#39019,#39020,#39021,#39022,#39023,#39024,#39025,#39026,#39027,#39028,
#39029,#39030,#39031,#39032,#39033,#39034,#39035,#39036,#39037,#39038,#39039,
#39040,#39041,#39042,#39043,#39044,#39045,#39046,#39047,#39048,#39049,#39050,
#39051,#39052,#39053),(#39054,#39055,#39056,#39057,#39058,#39059,#39060,
#39061,#39062,#39063,#39064,#39065,#39066,#39067,#39068,#39069,#39070,#39071,
#39072,#39073,#39074,#39075,#39076,#39077,#39078,#39079,#39080,#39081,#39082,
#39083,#39084,#39085,#39086,#39087,#39088)),.UNSPECIFIED.,.F.,.F.,.F.,(4,
4),(4,1,1,1,1,1,1,1,1,1,1,1,1,1,1,1,1,1,1,1,1,1,1,1,1,1,1,1,1,1,1,1,4),
(-0.1318015091147,1.131801509115),(0.08569894047188,0.1148310820745,0.1439632236771,
0.1730953652797,0.2022275068823,0.2313596484849,0.2604917900876,0.2896239316902,
0.3187560732928,0.3478882148954,0.377020356498,0.4061524981006,0.4352846397032,
0.4644167813058,0.4935489229084,0.5226810645111,0.5518132061137,0.5809453477163,
0.6100774893189,0.6392096309215,0.6683417725241,0.6974739141267,0.7266060557293,
0.7557381973319,0.7848703389346,0.8140024805372,0.8431346221398,0.8722667637424,
0.901398905345,0.9305310469476,0.9596631885502,0.9887953301528,1.017927471755),
 .UNSPECIFIED.);
#383=B_SPLINE_SURFACE_WITH_KNOTS('',3,3,((#39090,#39091,#39092,#39093,#39094,
#39095,#39096,#39097,#39098,#39099,#39100,#39101,#39102,#39103,#39104,#39105,
#39106,#39107,#39108,#39109,#39110,#39111,#39112,#39113,#39114,#39115,#39116,
#39117,#39118,#39119,#39120,#39121,#39122,#39123,#39124),(#39125,#39126,
#39127,#39128,#39129,#39130,#39131,#39132,#39133,#39134,#39135,#39136,#39137,
#39138,#39139,#39140,#39141,#39142,#39143,#39144,#39145,#39146,#39147,#39148,
#39149,#39150,#39151,#39152,#39153,#39154,#39155,#39156,#39157,#39158,#39159),
(#39160,#39161,#39162,#39163,#39164,#39165,#39166,#39167,#39168,#39169,
#39170,#39171,#39172,#39173,#39174,#39175,#39176,#39177,#39178,#39179,#39180,
#39181,#39182,#39183,#39184,#39185,#39186,#39187,#39188,#39189,#39190,#39191,
#39192,#39193,#39194),(#39195,#39196,#39197,#39198,#39199,#39200,#39201,
#39202,#39203,#39204,#39205,#39206,#39207,#39208,#39209,#39210,#39211,#39212,
#39213,#39214,#39215,#39216,#39217,#39218,#39219,#39220,#39221,#39222,#39223,
#39224,#39225,#39226,#39227,#39228,#39229)),.UNSPECIFIED.,.F.,.F.,.F.,(4,
4),(4,1,1,1,1,1,1,1,1,1,1,1,1,1,1,1,1,1,1,1,1,1,1,1,1,1,1,1,1,1,1,1,4),
(-0.1318015091147,1.131801509115),(-0.02,0.0125,0.045,0.0775,0.11,0.1425,
0.175,0.2075,0.24,0.2725,0.305,0.3375,0.37,0.4025,0.435,0.4675,0.5,0.5325,
0.565,0.5975,0.63,0.6625,0.695,0.7275,0.76,0.7925,0.825,0.8575,0.89,0.9225,
0.955,0.9875,1.02),.UNSPECIFIED.);
#384=B_SPLINE_SURFACE_WITH_KNOTS('',3,3,((#39231,#39232,#39233,#39234,#39235,
#39236,#39237,#39238,#39239,#39240,#39241,#39242,#39243,#39244,#39245,#39246,
#39247,#39248,#39249,#39250,#39251,#39252,#39253,#39254,#39255,#39256,#39257,
#39258,#39259,#39260,#39261,#39262,#39263,#39264,#39265),(#39266,#39267,
#39268,#39269,#39270,#39271,#39272,#39273,#39274,#39275,#39276,#39277,#39278,
#39279,#39280,#39281,#39282,#39283,#39284,#39285,#39286,#39287,#39288,#39289,
#39290,#39291,#39292,#39293,#39294,#39295,#39296,#39297,#39298,#39299,#39300),
(#39301,#39302,#39303,#39304,#39305,#39306,#39307,#39308,#39309,#39310,
#39311,#39312,#39313,#39314,#39315,#39316,#39317,#39318,#39319,#39320,#39321,
#39322,#39323,#39324,#39325,#39326,#39327,#39328,#39329,#39330,#39331,#39332,
#39333,#39334,#39335),(#39336,#39337,#39338,#39339,#39340,#39341,#39342,
#39343,#39344,#39345,#39346,#39347,#39348,#39349,#39350,#39351,#39352,#39353,
#39354,#39355,#39356,#39357,#39358,#39359,#39360,#39361,#39362,#39363,#39364,
#39365,#39366,#39367,#39368,#39369,#39370)),.UNSPECIFIED.,.F.,.F.,.F.,(4,
4),(4,1,1,1,1,1,1,1,1,1,1,1,1,1,1,1,1,1,1,1,1,1,1,1,1,1,1,1,1,1,1,1,4),
(-0.1318015091147,1.131801509115),(-0.02,0.0125,0.045,0.0775,0.11,0.1425,
0.175,0.2075,0.24,0.2725,0.305,0.3375,0.37,0.4025,0.435,0.4675,0.5,0.5325,
0.565,0.5975,0.63,0.6625,0.695,0.7275,0.76,0.7925,0.825,0.8575,0.89,0.9225,
0.955,0.9875,1.02),.UNSPECIFIED.);
#385=B_SPLINE_SURFACE_WITH_KNOTS('',3,3,((#39372,#39373,#39374,#39375,#39376,
#39377,#39378,#39379,#39380,#39381,#39382,#39383,#39384,#39385,#39386,#39387,
#39388,#39389,#39390,#39391,#39392,#39393,#39394,#39395,#39396,#39397,#39398,
#39399,#39400,#39401,#39402,#39403,#39404,#39405,#39406),(#39407,#39408,
#39409,#39410,#39411,#39412,#39413,#39414,#39415,#39416,#39417,#39418,#39419,
#39420,#39421,#39422,#39423,#39424,#39425,#39426,#39427,#39428,#39429,#39430,
#39431,#39432,#39433,#39434,#39435,#39436,#39437,#39438,#39439,#39440,#39441),
(#39442,#39443,#39444,#39445,#39446,#39447,#39448,#39449,#39450,#39451,
#39452,#39453,#39454,#39455,#39456,#39457,#39458,#39459,#39460,#39461,#39462,
#39463,#39464,#39465,#39466,#39467,#39468,#39469,#39470,#39471,#39472,#39473,
#39474,#39475,#39476),(#39477,#39478,#39479,#39480,#39481,#39482,#39483,
#39484,#39485,#39486,#39487,#39488,#39489,#39490,#39491,#39492,#39493,#39494,
#39495,#39496,#39497,#39498,#39499,#39500,#39501,#39502,#39503,#39504,#39505,
#39506,#39507,#39508,#39509,#39510,#39511)),.UNSPECIFIED.,.F.,.F.,.F.,(4,
4),(4,1,1,1,1,1,1,1,1,1,1,1,1,1,1,1,1,1,1,1,1,1,1,1,1,1,1,1,1,1,1,1,4),
(-0.1318015091147,1.131801509115),(-0.02,0.0125,0.045,0.0775,0.11,0.1425,
0.175,0.2075,0.24,0.2725,0.305,0.3375,0.37,0.4025,0.435,0.4675,0.5,0.5325,
0.565,0.5975,0.63,0.6625,0.695,0.7275,0.76,0.7925,0.825,0.8575,0.89,0.9225,
0.955,0.9875,1.02),.UNSPECIFIED.);
#386=B_SPLINE_SURFACE_WITH_KNOTS('',3,3,((#39513,#39514,#39515,#39516,#39517,
#39518,#39519,#39520,#39521,#39522,#39523,#39524,#39525,#39526,#39527,#39528,
#39529,#39530,#39531,#39532,#39533,#39534,#39535,#39536,#39537,#39538,#39539,
#39540,#39541,#39542,#39543,#39544,#39545,#39546,#39547),(#39548,#39549,
#39550,#39551,#39552,#39553,#39554,#39555,#39556,#39557,#39558,#39559,#39560,
#39561,#39562,#39563,#39564,#39565,#39566,#39567,#39568,#39569,#39570,#39571,
#39572,#39573,#39574,#39575,#39576,#39577,#39578,#39579,#39580,#39581,#39582),
(#39583,#39584,#39585,#39586,#39587,#39588,#39589,#39590,#39591,#39592,
#39593,#39594,#39595,#39596,#39597,#39598,#39599,#39600,#39601,#39602,#39603,
#39604,#39605,#39606,#39607,#39608,#39609,#39610,#39611,#39612,#39613,#39614,
#39615,#39616,#39617),(#39618,#39619,#39620,#39621,#39622,#39623,#39624,
#39625,#39626,#39627,#39628,#39629,#39630,#39631,#39632,#39633,#39634,#39635,
#39636,#39637,#39638,#39639,#39640,#39641,#39642,#39643,#39644,#39645,#39646,
#39647,#39648,#39649,#39650,#39651,#39652)),.UNSPECIFIED.,.F.,.F.,.F.,(4,
4),(4,1,1,1,1,1,1,1,1,1,1,1,1,1,1,1,1,1,1,1,1,1,1,1,1,1,1,1,1,1,1,1,4),
(-0.1318015091147,1.131801509115),(-0.02,0.0125,0.045,0.0775,0.11,0.1425,
0.175,0.2075,0.24,0.2725,0.305,0.3375,0.37,0.4025,0.435,0.4675,0.5,0.5325,
0.565,0.5975,0.63,0.6625,0.695,0.7275,0.76,0.7925,0.825,0.8575,0.89,0.9225,
0.955,0.9875,1.02),.UNSPECIFIED.);
#387=B_SPLINE_SURFACE_WITH_KNOTS('',3,3,((#39654,#39655,#39656,#39657,#39658,
#39659,#39660,#39661,#39662,#39663,#39664,#39665,#39666,#39667,#39668,#39669,
#39670,#39671,#39672,#39673,#39674,#39675,#39676,#39677,#39678,#39679,#39680,
#39681,#39682,#39683,#39684,#39685,#39686,#39687,#39688),(#39689,#39690,
#39691,#39692,#39693,#39694,#39695,#39696,#39697,#39698,#39699,#39700,#39701,
#39702,#39703,#39704,#39705,#39706,#39707,#39708,#39709,#39710,#39711,#39712,
#39713,#39714,#39715,#39716,#39717,#39718,#39719,#39720,#39721,#39722,#39723),
(#39724,#39725,#39726,#39727,#39728,#39729,#39730,#39731,#39732,#39733,
#39734,#39735,#39736,#39737,#39738,#39739,#39740,#39741,#39742,#39743,#39744,
#39745,#39746,#39747,#39748,#39749,#39750,#39751,#39752,#39753,#39754,#39755,
#39756,#39757,#39758),(#39759,#39760,#39761,#39762,#39763,#39764,#39765,
#39766,#39767,#39768,#39769,#39770,#39771,#39772,#39773,#39774,#39775,#39776,
#39777,#39778,#39779,#39780,#39781,#39782,#39783,#39784,#39785,#39786,#39787,
#39788,#39789,#39790,#39791,#39792,#39793)),.UNSPECIFIED.,.F.,.F.,.F.,(4,
4),(4,1,1,1,1,1,1,1,1,1,1,1,1,1,1,1,1,1,1,1,1,1,1,1,1,1,1,1,1,1,1,1,4),
(-0.1318015091147,1.131801509115),(-0.02,0.0125,0.045,0.0775,0.11,0.1425,
0.175,0.2075,0.24,0.2725,0.305,0.3375,0.37,0.4025,0.435,0.4675,0.5,0.5325,
0.565,0.5975,0.63,0.6625,0.695,0.7275,0.76,0.7925,0.825,0.8575,0.89,0.9225,
0.955,0.9875,1.02),.UNSPECIFIED.);
#388=B_SPLINE_SURFACE_WITH_KNOTS('',3,3,((#40199,#40200,#40201,#40202,#40203,
#40204,#40205,#40206,#40207,#40208,#40209,#40210,#40211,#40212,#40213,#40214,
#40215,#40216,#40217),(#40218,#40219,#40220,#40221,#40222,#40223,#40224,
#40225,#40226,#40227,#40228,#40229,#40230,#40231,#40232,#40233,#40234,#40235,
#40236),(#40237,#40238,#40239,#40240,#40241,#40242,#40243,#40244,#40245,
#40246,#40247,#40248,#40249,#40250,#40251,#40252,#40253,#40254,#40255),
(#40256,#40257,#40258,#40259,#40260,#40261,#40262,#40263,#40264,#40265,
#40266,#40267,#40268,#40269,#40270,#40271,#40272,#40273,#40274)),
 .UNSPECIFIED.,.F.,.F.,.F.,(4,4),(4,1,1,1,1,1,1,1,1,1,1,1,1,1,1,1,4),(-0.1077744783079,
1.107774478308),(0.7017764360683,0.7207808788678,0.7397853216674,0.758789764467,
0.7777942072665,0.7967986500661,0.8158030928657,0.8348075356653,0.8538119784648,
0.8728164212644,0.891820864064,0.9108253068635,0.9298297496631,0.9488341924627,
0.9678386352623,0.9868430780618,1.005847520861),.UNSPECIFIED.);
#389=B_SPLINE_SURFACE_WITH_KNOTS('',3,3,((#40368,#40369,#40370,#40371,#40372,
#40373,#40374,#40375,#40376,#40377,#40378,#40379,#40380,#40381,#40382,#40383,
#40384,#40385,#40386),(#40387,#40388,#40389,#40390,#40391,#40392,#40393,
#40394,#40395,#40396,#40397,#40398,#40399,#40400,#40401,#40402,#40403,#40404,
#40405),(#40406,#40407,#40408,#40409,#40410,#40411,#40412,#40413,#40414,
#40415,#40416,#40417,#40418,#40419,#40420,#40421,#40422,#40423,#40424),
(#40425,#40426,#40427,#40428,#40429,#40430,#40431,#40432,#40433,#40434,
#40435,#40436,#40437,#40438,#40439,#40440,#40441,#40442,#40443)),
 .UNSPECIFIED.,.F.,.F.,.F.,(4,4),(4,1,1,1,1,1,1,1,1,1,1,1,1,1,1,1,4),(-0.1077744783079,
1.107774478308),(0.49,0.5225,0.555,0.5875,0.62,0.6525,0.685,0.7175,0.75,
0.7825,0.815,0.8475,0.88,0.9125,0.945,0.9775,1.01),.UNSPECIFIED.);
#390=B_SPLINE_SURFACE_WITH_KNOTS('',3,3,((#40584,#40585,#40586,#40587,#40588,
#40589,#40590,#40591,#40592,#40593,#40594,#40595,#40596,#40597,#40598,#40599,
#40600,#40601,#40602),(#40603,#40604,#40605,#40606,#40607,#40608,#40609,
#40610,#40611,#40612,#40613,#40614,#40615,#40616,#40617,#40618,#40619,#40620,
#40621),(#40622,#40623,#40624,#40625,#40626,#40627,#40628,#40629,#40630,
#40631,#40632,#40633,#40634,#40635,#40636,#40637,#40638,#40639,#40640),
(#40641,#40642,#40643,#40644,#40645,#40646,#40647,#40648,#40649,#40650,
#40651,#40652,#40653,#40654,#40655,#40656,#40657,#40658,#40659)),
 .UNSPECIFIED.,.F.,.F.,.F.,(4,4),(4,1,1,1,1,1,1,1,1,1,1,1,1,1,1,1,4),(-0.1727715412221,
1.172771541222),(0.5842235639317,0.6107191211322,0.6372146783326,0.663710235533,
0.6902057927335,0.7167013499339,0.7431969071343,0.7696924643347,0.7961880215352,
0.8226835787356,0.849179135936,0.8756746931365,0.9021702503369,0.9286658075373,
0.9551613647377,0.9816569219382,1.008152479139),.UNSPECIFIED.);
#391=B_SPLINE_SURFACE_WITH_KNOTS('',3,3,((#40661,#40662,#40663,#40664,#40665,
#40666,#40667,#40668,#40669,#40670,#40671,#40672,#40673,#40674,#40675,#40676,
#40677,#40678,#40679,#40680,#40681,#40682,#40683,#40684,#40685,#40686,#40687,
#40688,#40689,#40690,#40691,#40692,#40693,#40694,#40695),(#40696,#40697,
#40698,#40699,#40700,#40701,#40702,#40703,#40704,#40705,#40706,#40707,#40708,
#40709,#40710,#40711,#40712,#40713,#40714,#40715,#40716,#40717,#40718,#40719,
#40720,#40721,#40722,#40723,#40724,#40725,#40726,#40727,#40728,#40729,#40730),
(#40731,#40732,#40733,#40734,#40735,#40736,#40737,#40738,#40739,#40740,
#40741,#40742,#40743,#40744,#40745,#40746,#40747,#40748,#40749,#40750,#40751,
#40752,#40753,#40754,#40755,#40756,#40757,#40758,#40759,#40760,#40761,#40762,
#40763,#40764,#40765),(#40766,#40767,#40768,#40769,#40770,#40771,#40772,
#40773,#40774,#40775,#40776,#40777,#40778,#40779,#40780,#40781,#40782,#40783,
#40784,#40785,#40786,#40787,#40788,#40789,#40790,#40791,#40792,#40793,#40794,
#40795,#40796,#40797,#40798,#40799,#40800)),.UNSPECIFIED.,.F.,.F.,.F.,(4,
4),(4,1,1,1,1,1,1,1,1,1,1,1,1,1,1,1,1,1,1,1,1,1,1,1,1,1,1,1,1,1,1,1,4),
(-0.1727715412221,1.172771541222),(-0.02,0.0125,0.045,0.0775,0.11,0.1425,
0.175,0.2075,0.24,0.2725,0.305,0.3375,0.37,0.4025,0.435,0.4675,0.5,0.5325,
0.565,0.5975,0.63,0.6625,0.695,0.7275,0.76,0.7925,0.825,0.8575,0.89,0.9225,
0.955,0.9875,1.02),.UNSPECIFIED.);
#392=B_SPLINE_SURFACE_WITH_KNOTS('',3,3,((#41024,#41025,#41026,#41027,#41028,
#41029,#41030,#41031,#41032,#41033,#41034,#41035,#41036,#41037,#41038,#41039,
#41040,#41041,#41042,#41043,#41044,#41045,#41046,#41047,#41048,#41049,#41050,
#41051,#41052,#41053,#41054,#41055,#41056,#41057,#41058),(#41059,#41060,
#41061,#41062,#41063,#41064,#41065,#41066,#41067,#41068,#41069,#41070,#41071,
#41072,#41073,#41074,#41075,#41076,#41077,#41078,#41079,#41080,#41081,#41082,
#41083,#41084,#41085,#41086,#41087,#41088,#41089,#41090,#41091,#41092,#41093),
(#41094,#41095,#41096,#41097,#41098,#41099,#41100,#41101,#41102,#41103,
#41104,#41105,#41106,#41107,#41108,#41109,#41110,#41111,#41112,#41113,#41114,
#41115,#41116,#41117,#41118,#41119,#41120,#41121,#41122,#41123,#41124,#41125,
#41126,#41127,#41128),(#41129,#41130,#41131,#41132,#41133,#41134,#41135,
#41136,#41137,#41138,#41139,#41140,#41141,#41142,#41143,#41144,#41145,#41146,
#41147,#41148,#41149,#41150,#41151,#41152,#41153,#41154,#41155,#41156,#41157,
#41158,#41159,#41160,#41161,#41162,#41163)),.UNSPECIFIED.,.F.,.F.,.F.,(4,
4),(4,1,1,1,1,1,1,1,1,1,1,1,1,1,1,1,1,1,1,1,1,1,1,1,1,1,1,1,1,1,1,1,4),
(-0.1077744783079,1.107774478308),(-0.02,0.0125,0.045,0.0775,0.11,0.1425,
0.175,0.2075,0.24,0.2725,0.305,0.3375,0.37,0.4025,0.435,0.4675,0.5,0.5325,
0.565,0.5975,0.63,0.6625,0.695,0.7275,0.76,0.7925,0.825,0.8575,0.89,0.9225,
0.955,0.9875,1.02),.UNSPECIFIED.);
#393=B_SPLINE_SURFACE_WITH_KNOTS('',3,3,((#41346,#41347,#41348,#41349,#41350,
#41351,#41352,#41353,#41354,#41355,#41356,#41357,#41358,#41359,#41360,#41361,
#41362,#41363,#41364,#41365,#41366,#41367,#41368,#41369,#41370,#41371,#41372,
#41373,#41374,#41375,#41376,#41377,#41378,#41379,#41380),(#41381,#41382,
#41383,#41384,#41385,#41386,#41387,#41388,#41389,#41390,#41391,#41392,#41393,
#41394,#41395,#41396,#41397,#41398,#41399,#41400,#41401,#41402,#41403,#41404,
#41405,#41406,#41407,#41408,#41409,#41410,#41411,#41412,#41413,#41414,#41415),
(#41416,#41417,#41418,#41419,#41420,#41421,#41422,#41423,#41424,#41425,
#41426,#41427,#41428,#41429,#41430,#41431,#41432,#41433,#41434,#41435,#41436,
#41437,#41438,#41439,#41440,#41441,#41442,#41443,#41444,#41445,#41446,#41447,
#41448,#41449,#41450),(#41451,#41452,#41453,#41454,#41455,#41456,#41457,
#41458,#41459,#41460,#41461,#41462,#41463,#41464,#41465,#41466,#41467,#41468,
#41469,#41470,#41471,#41472,#41473,#41474,#41475,#41476,#41477,#41478,#41479,
#41480,#41481,#41482,#41483,#41484,#41485)),.UNSPECIFIED.,.F.,.F.,.F.,(4,
4),(4,1,1,1,1,1,1,1,1,1,1,1,1,1,1,1,1,1,1,1,1,1,1,1,1,1,1,1,1,1,1,1,4),
(-0.1077744783079,1.107774478308),(-0.02,0.0125,0.045,0.0775,0.11,0.1425,
0.175,0.2075,0.24,0.2725,0.305,0.3375,0.37,0.4025,0.435,0.4675,0.5,0.5325,
0.565,0.5975,0.63,0.6625,0.695,0.7275,0.76,0.7925,0.825,0.8575,0.89,0.9225,
0.955,0.9875,1.02),.UNSPECIFIED.);
#394=B_SPLINE_SURFACE_WITH_KNOTS('',3,3,((#41598,#41599,#41600,#41601,#41602,
#41603,#41604,#41605,#41606,#41607,#41608,#41609,#41610,#41611,#41612,#41613,
#41614,#41615,#41616,#41617,#41618,#41619,#41620,#41621,#41622,#41623,#41624,
#41625,#41626,#41627,#41628,#41629,#41630,#41631,#41632),(#41633,#41634,
#41635,#41636,#41637,#41638,#41639,#41640,#41641,#41642,#41643,#41644,#41645,
#41646,#41647,#41648,#41649,#41650,#41651,#41652,#41653,#41654,#41655,#41656,
#41657,#41658,#41659,#41660,#41661,#41662,#41663,#41664,#41665,#41666,#41667),
(#41668,#41669,#41670,#41671,#41672,#41673,#41674,#41675,#41676,#41677,
#41678,#41679,#41680,#41681,#41682,#41683,#41684,#41685,#41686,#41687,#41688,
#41689,#41690,#41691,#41692,#41693,#41694,#41695,#41696,#41697,#41698,#41699,
#41700,#41701,#41702),(#41703,#41704,#41705,#41706,#41707,#41708,#41709,
#41710,#41711,#41712,#41713,#41714,#41715,#41716,#41717,#41718,#41719,#41720,
#41721,#41722,#41723,#41724,#41725,#41726,#41727,#41728,#41729,#41730,#41731,
#41732,#41733,#41734,#41735,#41736,#41737)),.UNSPECIFIED.,.F.,.F.,.F.,(4,
4),(4,1,1,1,1,1,1,1,1,1,1,1,1,1,1,1,1,1,1,1,1,1,1,1,1,1,1,1,1,1,1,1,4),
(-0.1077744783079,1.107774478308),(-0.02,0.0125,0.045,0.0775,0.11,0.1425,
0.175,0.2075,0.24,0.2725,0.305,0.3375,0.37,0.4025,0.435,0.4675,0.5,0.5325,
0.565,0.5975,0.63,0.6625,0.695,0.7275,0.76,0.7925,0.825,0.8575,0.89,0.9225,
0.955,0.9875,1.02),.UNSPECIFIED.);
#395=B_SPLINE_SURFACE_WITH_KNOTS('',3,3,((#42140,#42141,#42142,#42143,#42144,
#42145,#42146,#42147,#42148,#42149,#42150,#42151,#42152,#42153,#42154,#42155,
#42156,#42157,#42158,#42159,#42160,#42161,#42162,#42163,#42164,#42165,#42166,
#42167,#42168,#42169,#42170,#42171,#42172,#42173,#42174),(#42175,#42176,
#42177,#42178,#42179,#42180,#42181,#42182,#42183,#42184,#42185,#42186,#42187,
#42188,#42189,#42190,#42191,#42192,#42193,#42194,#42195,#42196,#42197,#42198,
#42199,#42200,#42201,#42202,#42203,#42204,#42205,#42206,#42207,#42208,#42209),
(#42210,#42211,#42212,#42213,#42214,#42215,#42216,#42217,#42218,#42219,
#42220,#42221,#42222,#42223,#42224,#42225,#42226,#42227,#42228,#42229,#42230,
#42231,#42232,#42233,#42234,#42235,#42236,#42237,#42238,#42239,#42240,#42241,
#42242,#42243,#42244),(#42245,#42246,#42247,#42248,#42249,#42250,#42251,
#42252,#42253,#42254,#42255,#42256,#42257,#42258,#42259,#42260,#42261,#42262,
#42263,#42264,#42265,#42266,#42267,#42268,#42269,#42270,#42271,#42272,#42273,
#42274,#42275,#42276,#42277,#42278,#42279)),.UNSPECIFIED.,.F.,.F.,.F.,(4,
4),(4,1,1,1,1,1,1,1,1,1,1,1,1,1,1,1,1,1,1,1,1,1,1,1,1,1,1,1,1,1,1,1,4),
(-0.1077744783079,1.107774478308),(-0.02,0.0125,0.045,0.0775,0.11,0.1425,
0.175,0.2075,0.24,0.2725,0.305,0.3375,0.37,0.4025,0.435,0.4675,0.5,0.5325,
0.565,0.5975,0.63,0.6625,0.695,0.7275,0.76,0.7925,0.825,0.8575,0.89,0.9225,
0.955,0.9875,1.02),.UNSPECIFIED.);
#396=B_SPLINE_SURFACE_WITH_KNOTS('',3,3,((#42392,#42393,#42394,#42395,#42396,
#42397,#42398,#42399,#42400,#42401,#42402,#42403,#42404,#42405,#42406,#42407,
#42408,#42409,#42410,#42411,#42412,#42413,#42414,#42415,#42416,#42417,#42418,
#42419,#42420,#42421,#42422,#42423,#42424,#42425,#42426),(#42427,#42428,
#42429,#42430,#42431,#42432,#42433,#42434,#42435,#42436,#42437,#42438,#42439,
#42440,#42441,#42442,#42443,#42444,#42445,#42446,#42447,#42448,#42449,#42450,
#42451,#42452,#42453,#42454,#42455,#42456,#42457,#42458,#42459,#42460,#42461),
(#42462,#42463,#42464,#42465,#42466,#42467,#42468,#42469,#42470,#42471,
#42472,#42473,#42474,#42475,#42476,#42477,#42478,#42479,#42480,#42481,#42482,
#42483,#42484,#42485,#42486,#42487,#42488,#42489,#42490,#42491,#42492,#42493,
#42494,#42495,#42496),(#42497,#42498,#42499,#42500,#42501,#42502,#42503,
#42504,#42505,#42506,#42507,#42508,#42509,#42510,#42511,#42512,#42513,#42514,
#42515,#42516,#42517,#42518,#42519,#42520,#42521,#42522,#42523,#42524,#42525,
#42526,#42527,#42528,#42529,#42530,#42531)),.UNSPECIFIED.,.F.,.F.,.F.,(4,
4),(4,1,1,1,1,1,1,1,1,1,1,1,1,1,1,1,1,1,1,1,1,1,1,1,1,1,1,1,1,1,1,1,4),
(-0.1077744783079,1.107774478308),(-0.02,0.0125,0.045,0.0775,0.11,0.1425,
0.175,0.2075,0.24,0.2725,0.305,0.3375,0.37,0.4025,0.435,0.4675,0.5,0.5325,
0.565,0.5975,0.63,0.6625,0.695,0.7275,0.76,0.7925,0.825,0.8575,0.89,0.9225,
0.955,0.9875,1.02),.UNSPECIFIED.);
#397=B_SPLINE_SURFACE_WITH_KNOTS('',3,3,((#42827,#42828,#42829,#42830,#42831,
#42832,#42833,#42834,#42835,#42836,#42837,#42838,#42839,#42840,#42841,#42842,
#42843,#42844,#42845,#42846,#42847,#42848,#42849,#42850,#42851,#42852,#42853,
#42854,#42855,#42856,#42857,#42858,#42859,#42860,#42861),(#42862,#42863,
#42864,#42865,#42866,#42867,#42868,#42869,#42870,#42871,#42872,#42873,#42874,
#42875,#42876,#42877,#42878,#42879,#42880,#42881,#42882,#42883,#42884,#42885,
#42886,#42887,#42888,#42889,#42890,#42891,#42892,#42893,#42894,#42895,#42896),
(#42897,#42898,#42899,#42900,#42901,#42902,#42903,#42904,#42905,#42906,
#42907,#42908,#42909,#42910,#42911,#42912,#42913,#42914,#42915,#42916,#42917,
#42918,#42919,#42920,#42921,#42922,#42923,#42924,#42925,#42926,#42927,#42928,
#42929,#42930,#42931),(#42932,#42933,#42934,#42935,#42936,#42937,#42938,
#42939,#42940,#42941,#42942,#42943,#42944,#42945,#42946,#42947,#42948,#42949,
#42950,#42951,#42952,#42953,#42954,#42955,#42956,#42957,#42958,#42959,#42960,
#42961,#42962,#42963,#42964,#42965,#42966)),.UNSPECIFIED.,.F.,.F.,.F.,(4,
4),(4,1,1,1,1,1,1,1,1,1,1,1,1,1,1,1,1,1,1,1,1,1,1,1,1,1,1,1,1,1,1,1,4),
(-0.1077744783079,1.107774478308),(-0.02,0.0125,0.045,0.0775,0.11,0.1425,
0.175,0.2075,0.24,0.2725,0.305,0.3375,0.37,0.4025,0.435,0.4675,0.5,0.5325,
0.565,0.5975,0.63,0.6625,0.695,0.7275,0.76,0.7925,0.825,0.8575,0.89,0.9225,
0.955,0.9875,1.02),.UNSPECIFIED.);
#398=B_SPLINE_SURFACE_WITH_KNOTS('',3,3,((#43084,#43085,#43086,#43087,#43088,
#43089,#43090,#43091,#43092,#43093,#43094,#43095,#43096,#43097,#43098,#43099,
#43100,#43101,#43102,#43103,#43104,#43105,#43106,#43107,#43108,#43109,#43110,
#43111,#43112,#43113,#43114,#43115,#43116,#43117,#43118),(#43119,#43120,
#43121,#43122,#43123,#43124,#43125,#43126,#43127,#43128,#43129,#43130,#43131,
#43132,#43133,#43134,#43135,#43136,#43137,#43138,#43139,#43140,#43141,#43142,
#43143,#43144,#43145,#43146,#43147,#43148,#43149,#43150,#43151,#43152,#43153),
(#43154,#43155,#43156,#43157,#43158,#43159,#43160,#43161,#43162,#43163,
#43164,#43165,#43166,#43167,#43168,#43169,#43170,#43171,#43172,#43173,#43174,
#43175,#43176,#43177,#43178,#43179,#43180,#43181,#43182,#43183,#43184,#43185,
#43186,#43187,#43188),(#43189,#43190,#43191,#43192,#43193,#43194,#43195,
#43196,#43197,#43198,#43199,#43200,#43201,#43202,#43203,#43204,#43205,#43206,
#43207,#43208,#43209,#43210,#43211,#43212,#43213,#43214,#43215,#43216,#43217,
#43218,#43219,#43220,#43221,#43222,#43223)),.UNSPECIFIED.,.F.,.F.,.F.,(4,
4),(4,1,1,1,1,1,1,1,1,1,1,1,1,1,1,1,1,1,1,1,1,1,1,1,1,1,1,1,1,1,1,1,4),
(-0.1727715412221,1.172771541222),(-0.02,0.0125,0.045,0.0775,0.11,0.1425,
0.175,0.2075,0.24,0.2725,0.305,0.3375,0.37,0.4025,0.435,0.4675,0.5,0.5325,
0.565,0.5975,0.63,0.6625,0.695,0.7275,0.76,0.7925,0.825,0.8575,0.89,0.9225,
0.955,0.9875,1.02),.UNSPECIFIED.);
#399=B_SPLINE_SURFACE_WITH_KNOTS('',3,3,((#43231,#43232,#43233,#43234,#43235,
#43236,#43237,#43238,#43239,#43240,#43241,#43242,#43243,#43244,#43245,#43246,
#43247,#43248,#43249,#43250,#43251,#43252,#43253,#43254,#43255,#43256,#43257,
#43258,#43259,#43260,#43261,#43262,#43263,#43264,#43265),(#43266,#43267,
#43268,#43269,#43270,#43271,#43272,#43273,#43274,#43275,#43276,#43277,#43278,
#43279,#43280,#43281,#43282,#43283,#43284,#43285,#43286,#43287,#43288,#43289,
#43290,#43291,#43292,#43293,#43294,#43295,#43296,#43297,#43298,#43299,#43300),
(#43301,#43302,#43303,#43304,#43305,#43306,#43307,#43308,#43309,#43310,
#43311,#43312,#43313,#43314,#43315,#43316,#43317,#43318,#43319,#43320,#43321,
#43322,#43323,#43324,#43325,#43326,#43327,#43328,#43329,#43330,#43331,#43332,
#43333,#43334,#43335),(#43336,#43337,#43338,#43339,#43340,#43341,#43342,
#43343,#43344,#43345,#43346,#43347,#43348,#43349,#43350,#43351,#43352,#43353,
#43354,#43355,#43356,#43357,#43358,#43359,#43360,#43361,#43362,#43363,#43364,
#43365,#43366,#43367,#43368,#43369,#43370)),.UNSPECIFIED.,.F.,.F.,.F.,(4,
4),(4,1,1,1,1,1,1,1,1,1,1,1,1,1,1,1,1,1,1,1,1,1,1,1,1,1,1,1,1,1,1,1,4),
(-0.1727715412221,1.172771541222),(-0.02,0.0125,0.045,0.0775,0.11,0.1425,
0.175,0.2075,0.24,0.2725,0.305,0.3375,0.37,0.4025,0.435,0.4675,0.5,0.5325,
0.565,0.5975,0.63,0.6625,0.695,0.7275,0.76,0.7925,0.825,0.8575,0.89,0.9225,
0.955,0.9875,1.02),.UNSPECIFIED.);
#400=B_SPLINE_SURFACE_WITH_KNOTS('',3,3,((#46509,#46510,#46511,#46512,#46513,
#46514,#46515,#46516,#46517,#46518,#46519,#46520,#46521,#46522,#46523,#46524,
#46525,#46526,#46527,#46528,#46529,#46530,#46531,#46532,#46533,#46534,#46535,
#46536,#46537,#46538,#46539,#46540,#46541,#46542,#46543,#46544,#46545,#46546,
#46547,#46548,#46549,#46550,#46551,#46552,#46553,#46554,#46555,#46556,#46557,
#46558,#46559,#46560,#46561,#46562,#46563,#46564,#46565,#46566,#46567,#46568,
#46569,#46570,#46571,#46572,#46573,#46574,#46575),(#46576,#46577,#46578,
#46579,#46580,#46581,#46582,#46583,#46584,#46585,#46586,#46587,#46588,#46589,
#46590,#46591,#46592,#46593,#46594,#46595,#46596,#46597,#46598,#46599,#46600,
#46601,#46602,#46603,#46604,#46605,#46606,#46607,#46608,#46609,#46610,#46611,
#46612,#46613,#46614,#46615,#46616,#46617,#46618,#46619,#46620,#46621,#46622,
#46623,#46624,#46625,#46626,#46627,#46628,#46629,#46630,#46631,#46632,#46633,
#46634,#46635,#46636,#46637,#46638,#46639,#46640,#46641,#46642),(#46643,
#46644,#46645,#46646,#46647,#46648,#46649,#46650,#46651,#46652,#46653,#46654,
#46655,#46656,#46657,#46658,#46659,#46660,#46661,#46662,#46663,#46664,#46665,
#46666,#46667,#46668,#46669,#46670,#46671,#46672,#46673,#46674,#46675,#46676,
#46677,#46678,#46679,#46680,#46681,#46682,#46683,#46684,#46685,#46686,#46687,
#46688,#46689,#46690,#46691,#46692,#46693,#46694,#46695,#46696,#46697,#46698,
#46699,#46700,#46701,#46702,#46703,#46704,#46705,#46706,#46707,#46708,#46709),
(#46710,#46711,#46712,#46713,#46714,#46715,#46716,#46717,#46718,#46719,
#46720,#46721,#46722,#46723,#46724,#46725,#46726,#46727,#46728,#46729,#46730,
#46731,#46732,#46733,#46734,#46735,#46736,#46737,#46738,#46739,#46740,#46741,
#46742,#46743,#46744,#46745,#46746,#46747,#46748,#46749,#46750,#46751,#46752,
#46753,#46754,#46755,#46756,#46757,#46758,#46759,#46760,#46761,#46762,#46763,
#46764,#46765,#46766,#46767,#46768,#46769,#46770,#46771,#46772,#46773,#46774,
#46775,#46776)),.UNSPECIFIED.,.F.,.F.,.F.,(4,4),(4,1,1,1,1,1,1,1,1,1,1,
1,1,1,1,1,1,1,1,1,1,1,1,1,1,1,1,1,1,1,1,1,1,1,1,1,1,1,1,1,1,1,1,1,1,1,1,
1,1,1,1,1,1,1,1,1,1,1,1,1,1,1,1,1,4),(-0.04605142190376,1.046051421904),
(-0.02,-0.00375,0.0125,0.02875,0.045,0.06125,0.0775,0.09375,0.11,0.12625,
0.1425,0.15875,0.175,0.19125,0.2075,0.22375,0.24,0.25625,0.2725,0.28875,
0.305,0.32125,0.3375,0.35375,0.37,0.38625,0.4025,0.41875,0.435,0.45125,
0.4675,0.48375,0.5,0.51625,0.5325,0.54875,0.565,0.58125,0.5975,0.61375,
0.63,0.64625,0.6625,0.67875,0.695,0.71125,0.7275,0.74375,0.76,0.77625,0.7925,
0.80875,0.825,0.84125,0.8575,0.87375,0.89,0.90625,0.9225,0.93875,0.955,
0.97125,0.9875,1.00375,1.02),.UNSPECIFIED.);
#401=B_SPLINE_SURFACE_WITH_KNOTS('',3,3,((#47626,#47627,#47628,#47629,#47630,
#47631,#47632,#47633,#47634,#47635,#47636,#47637,#47638,#47639,#47640,#47641,
#47642,#47643,#47644,#47645,#47646,#47647,#47648,#47649,#47650,#47651,#47652,
#47653,#47654,#47655,#47656,#47657,#47658,#47659,#47660,#47661,#47662,#47663,
#47664,#47665,#47666,#47667,#47668,#47669,#47670,#47671,#47672,#47673,#47674,
#47675,#47676,#47677,#47678,#47679,#47680,#47681,#47682,#47683,#47684,#47685,
#47686,#47687,#47688,#47689,#47690,#47691,#47692),(#47693,#47694,#47695,
#47696,#47697,#47698,#47699,#47700,#47701,#47702,#47703,#47704,#47705,#47706,
#47707,#47708,#47709,#47710,#47711,#47712,#47713,#47714,#47715,#47716,#47717,
#47718,#47719,#47720,#47721,#47722,#47723,#47724,#47725,#47726,#47727,#47728,
#47729,#47730,#47731,#47732,#47733,#47734,#47735,#47736,#47737,#47738,#47739,
#47740,#47741,#47742,#47743,#47744,#47745,#47746,#47747,#47748,#47749,#47750,
#47751,#47752,#47753,#47754,#47755,#47756,#47757,#47758,#47759),(#47760,
#47761,#47762,#47763,#47764,#47765,#47766,#47767,#47768,#47769,#47770,#47771,
#47772,#47773,#47774,#47775,#47776,#47777,#47778,#47779,#47780,#47781,#47782,
#47783,#47784,#47785,#47786,#47787,#47788,#47789,#47790,#47791,#47792,#47793,
#47794,#47795,#47796,#47797,#47798,#47799,#47800,#47801,#47802,#47803,#47804,
#47805,#47806,#47807,#47808,#47809,#47810,#47811,#47812,#47813,#47814,#47815,
#47816,#47817,#47818,#47819,#47820,#47821,#47822,#47823,#47824,#47825,#47826),
(#47827,#47828,#47829,#47830,#47831,#47832,#47833,#47834,#47835,#47836,
#47837,#47838,#47839,#47840,#47841,#47842,#47843,#47844,#47845,#47846,#47847,
#47848,#47849,#47850,#47851,#47852,#47853,#47854,#47855,#47856,#47857,#47858,
#47859,#47860,#47861,#47862,#47863,#47864,#47865,#47866,#47867,#47868,#47869,
#47870,#47871,#47872,#47873,#47874,#47875,#47876,#47877,#47878,#47879,#47880,
#47881,#47882,#47883,#47884,#47885,#47886,#47887,#47888,#47889,#47890,#47891,
#47892,#47893)),.UNSPECIFIED.,.F.,.F.,.F.,(4,4),(4,1,1,1,1,1,1,1,1,1,1,
1,1,1,1,1,1,1,1,1,1,1,1,1,1,1,1,1,1,1,1,1,1,1,1,1,1,1,1,1,1,1,1,1,1,1,1,
1,1,1,1,1,1,1,1,1,1,1,1,1,1,1,1,1,4),(-0.04605142190375,1.046051421904),
(-0.02,-0.00375,0.0125,0.02875,0.045,0.06125,0.0775,0.09375,0.11,0.12625,
0.1425,0.15875,0.175,0.19125,0.2075,0.22375,0.24,0.25625,0.2725,0.28875,
0.305,0.32125,0.3375,0.35375,0.37,0.38625,0.4025,0.41875,0.435,0.45125,
0.4675,0.48375,0.5,0.51625,0.5325,0.54875,0.565,0.58125,0.5975,0.61375,
0.63,0.64625,0.6625,0.67875,0.695,0.71125,0.7275,0.74375,0.76,0.77625,0.7925,
0.80875,0.825,0.84125,0.8575,0.87375,0.89,0.90625,0.9225,0.93875,0.955,
0.97125,0.9875,1.00375,1.02),.UNSPECIFIED.);
#402=B_SPLINE_SURFACE_WITH_KNOTS('',3,3,((#48678,#48679,#48680,#48681,#48682,
#48683,#48684,#48685,#48686,#48687,#48688,#48689,#48690,#48691,#48692,#48693,
#48694,#48695,#48696,#48697,#48698,#48699,#48700,#48701,#48702,#48703,#48704,
#48705,#48706,#48707,#48708,#48709,#48710,#48711,#48712,#48713,#48714,#48715,
#48716,#48717,#48718,#48719,#48720,#48721,#48722,#48723,#48724,#48725,#48726,
#48727,#48728,#48729,#48730,#48731,#48732,#48733,#48734,#48735,#48736,#48737,
#48738,#48739,#48740,#48741,#48742,#48743,#48744),(#48745,#48746,#48747,
#48748,#48749,#48750,#48751,#48752,#48753,#48754,#48755,#48756,#48757,#48758,
#48759,#48760,#48761,#48762,#48763,#48764,#48765,#48766,#48767,#48768,#48769,
#48770,#48771,#48772,#48773,#48774,#48775,#48776,#48777,#48778,#48779,#48780,
#48781,#48782,#48783,#48784,#48785,#48786,#48787,#48788,#48789,#48790,#48791,
#48792,#48793,#48794,#48795,#48796,#48797,#48798,#48799,#48800,#48801,#48802,
#48803,#48804,#48805,#48806,#48807,#48808,#48809,#48810,#48811),(#48812,
#48813,#48814,#48815,#48816,#48817,#48818,#48819,#48820,#48821,#48822,#48823,
#48824,#48825,#48826,#48827,#48828,#48829,#48830,#48831,#48832,#48833,#48834,
#48835,#48836,#48837,#48838,#48839,#48840,#48841,#48842,#48843,#48844,#48845,
#48846,#48847,#48848,#48849,#48850,#48851,#48852,#48853,#48854,#48855,#48856,
#48857,#48858,#48859,#48860,#48861,#48862,#48863,#48864,#48865,#48866,#48867,
#48868,#48869,#48870,#48871,#48872,#48873,#48874,#48875,#48876,#48877,#48878),
(#48879,#48880,#48881,#48882,#48883,#48884,#48885,#48886,#48887,#48888,
#48889,#48890,#48891,#48892,#48893,#48894,#48895,#48896,#48897,#48898,#48899,
#48900,#48901,#48902,#48903,#48904,#48905,#48906,#48907,#48908,#48909,#48910,
#48911,#48912,#48913,#48914,#48915,#48916,#48917,#48918,#48919,#48920,#48921,
#48922,#48923,#48924,#48925,#48926,#48927,#48928,#48929,#48930,#48931,#48932,
#48933,#48934,#48935,#48936,#48937,#48938,#48939,#48940,#48941,#48942,#48943,
#48944,#48945)),.UNSPECIFIED.,.F.,.F.,.F.,(4,4),(4,1,1,1,1,1,1,1,1,1,1,
1,1,1,1,1,1,1,1,1,1,1,1,1,1,1,1,1,1,1,1,1,1,1,1,1,1,1,1,1,1,1,1,1,1,1,1,
1,1,1,1,1,1,1,1,1,1,1,1,1,1,1,1,1,4),(-0.04605142190375,1.046051421904),
(-0.02,-0.00375,0.0125,0.02875,0.045,0.06125,0.0775,0.09375,0.11,0.12625,
0.1425,0.15875,0.175,0.19125,0.2075,0.22375,0.24,0.25625,0.2725,0.28875,
0.305,0.32125,0.3375,0.35375,0.37,0.38625,0.4025,0.41875,0.435,0.45125,
0.4675,0.48375,0.5,0.51625,0.5325,0.54875,0.565,0.58125,0.5975,0.61375,
0.63,0.64625,0.6625,0.67875,0.695,0.71125,0.7275,0.74375,0.76,0.77625,0.7925,
0.80875,0.825,0.84125,0.8575,0.87375,0.89,0.90625,0.9225,0.93875,0.955,
0.97125,0.9875,1.00375,1.02),.UNSPECIFIED.);
#403=B_SPLINE_SURFACE_WITH_KNOTS('',3,3,((#49626,#49627,#49628,#49629,#49630,
#49631,#49632,#49633,#49634,#49635,#49636,#49637,#49638,#49639,#49640,#49641,
#49642,#49643,#49644,#49645,#49646,#49647,#49648,#49649,#49650,#49651,#49652,
#49653,#49654,#49655,#49656,#49657,#49658,#49659,#49660,#49661,#49662,#49663,
#49664,#49665,#49666,#49667,#49668,#49669,#49670,#49671,#49672,#49673,#49674,
#49675,#49676,#49677,#49678,#49679,#49680,#49681,#49682,#49683,#49684,#49685,
#49686,#49687,#49688,#49689,#49690,#49691,#49692),(#49693,#49694,#49695,
#49696,#49697,#49698,#49699,#49700,#49701,#49702,#49703,#49704,#49705,#49706,
#49707,#49708,#49709,#49710,#49711,#49712,#49713,#49714,#49715,#49716,#49717,
#49718,#49719,#49720,#49721,#49722,#49723,#49724,#49725,#49726,#49727,#49728,
#49729,#49730,#49731,#49732,#49733,#49734,#49735,#49736,#49737,#49738,#49739,
#49740,#49741,#49742,#49743,#49744,#49745,#49746,#49747,#49748,#49749,#49750,
#49751,#49752,#49753,#49754,#49755,#49756,#49757,#49758,#49759),(#49760,
#49761,#49762,#49763,#49764,#49765,#49766,#49767,#49768,#49769,#49770,#49771,
#49772,#49773,#49774,#49775,#49776,#49777,#49778,#49779,#49780,#49781,#49782,
#49783,#49784,#49785,#49786,#49787,#49788,#49789,#49790,#49791,#49792,#49793,
#49794,#49795,#49796,#49797,#49798,#49799,#49800,#49801,#49802,#49803,#49804,
#49805,#49806,#49807,#49808,#49809,#49810,#49811,#49812,#49813,#49814,#49815,
#49816,#49817,#49818,#49819,#49820,#49821,#49822,#49823,#49824,#49825,#49826),
(#49827,#49828,#49829,#49830,#49831,#49832,#49833,#49834,#49835,#49836,
#49837,#49838,#49839,#49840,#49841,#49842,#49843,#49844,#49845,#49846,#49847,
#49848,#49849,#49850,#49851,#49852,#49853,#49854,#49855,#49856,#49857,#49858,
#49859,#49860,#49861,#49862,#49863,#49864,#49865,#49866,#49867,#49868,#49869,
#49870,#49871,#49872,#49873,#49874,#49875,#49876,#49877,#49878,#49879,#49880,
#49881,#49882,#49883,#49884,#49885,#49886,#49887,#49888,#49889,#49890,#49891,
#49892,#49893)),.UNSPECIFIED.,.F.,.F.,.F.,(4,4),(4,1,1,1,1,1,1,1,1,1,1,
1,1,1,1,1,1,1,1,1,1,1,1,1,1,1,1,1,1,1,1,1,1,1,1,1,1,1,1,1,1,1,1,1,1,1,1,
1,1,1,1,1,1,1,1,1,1,1,1,1,1,1,1,1,4),(-0.04605142190375,1.046051421904),
(0.151,0.1645257352941,0.1780514705882,0.1915772058824,0.2051029411765,
0.2186286764706,0.2321544117647,0.2456801470588,0.2592058823529,0.2727316176471,
0.2862573529412,0.2997830882353,0.3133088235294,0.3268345588235,0.3403602941176,
0.3538860294118,0.3674117647059,0.3809375,0.3944632352941,0.4079889705882,
0.4215147058824,0.4350404411765,0.4485661764706,0.4620919117647,0.4756176470588,
0.4891433823529,0.5026691176471,0.5161948529412,0.5297205882353,0.5432463235294,
0.5567720588235,0.5702977941176,0.5838235294118,0.5973492647059,0.610875,
0.6244007352941,0.6379264705882,0.6514522058824,0.6649779411765,0.6785036764706,
0.6920294117647,0.7055551470588,0.7190808823529,0.7326066176471,0.7461323529412,
0.7596580882353,0.7731838235294,0.7867095588235,0.8002352941176,0.8137610294118,
0.8272867647059,0.8408125,0.8543382352941,0.8678639705882,0.8813897058824,
0.8949154411765,0.9084411764706,0.9219669117647,0.9354926470588,0.9490183823529,
0.9625441176471,0.9760698529412,0.9895955882353,1.003121323529,1.016647058824),
 .UNSPECIFIED.);
#404=B_SPLINE_SURFACE_WITH_KNOTS('',3,3,((#50188,#50189,#50190,#50191,#50192,
#50193,#50194,#50195,#50196,#50197,#50198,#50199,#50200,#50201,#50202,#50203,
#50204,#50205,#50206,#50207,#50208,#50209,#50210,#50211,#50212,#50213,#50214,
#50215,#50216,#50217,#50218,#50219,#50220,#50221,#50222),(#50223,#50224,
#50225,#50226,#50227,#50228,#50229,#50230,#50231,#50232,#50233,#50234,#50235,
#50236,#50237,#50238,#50239,#50240,#50241,#50242,#50243,#50244,#50245,#50246,
#50247,#50248,#50249,#50250,#50251,#50252,#50253,#50254,#50255,#50256,#50257),
(#50258,#50259,#50260,#50261,#50262,#50263,#50264,#50265,#50266,#50267,
#50268,#50269,#50270,#50271,#50272,#50273,#50274,#50275,#50276,#50277,#50278,
#50279,#50280,#50281,#50282,#50283,#50284,#50285,#50286,#50287,#50288,#50289,
#50290,#50291,#50292),(#50293,#50294,#50295,#50296,#50297,#50298,#50299,
#50300,#50301,#50302,#50303,#50304,#50305,#50306,#50307,#50308,#50309,#50310,
#50311,#50312,#50313,#50314,#50315,#50316,#50317,#50318,#50319,#50320,#50321,
#50322,#50323,#50324,#50325,#50326,#50327)),.UNSPECIFIED.,.F.,.F.,.F.,(4,
4),(4,1,1,1,1,1,1,1,1,1,1,1,1,1,1,1,1,1,1,1,1,1,1,1,1,1,1,1,1,1,1,1,4),
(-0.04605142190375,1.046051421904),(0.3253907954222,0.3468856965485,0.3683805976747,
0.389875498801,0.4113703999272,0.4328653010535,0.4543602021797,0.475855103306,
0.4973500044322,0.5188449055585,0.5403398066847,0.561834707811,0.5833296089372,
0.6048245100635,0.6263194111897,0.647814312316,0.6693092134423,0.6908041145685,
0.7122990156948,0.733793916821,0.7552888179473,0.7767837190735,0.7982786201998,
0.819773521326,0.8412684224523,0.8627633235785,0.8842582247048,0.905753125831,
0.9272480269573,0.9487429280835,0.9702378292098,0.9917327303361,1.013227631462),
 .UNSPECIFIED.);
#405=B_SPLINE_SURFACE_WITH_KNOTS('',3,3,((#50500,#50501,#50502,#50503,#50504,
#50505,#50506,#50507,#50508,#50509,#50510,#50511,#50512,#50513,#50514,#50515,
#50516,#50517,#50518,#50519,#50520,#50521,#50522,#50523,#50524,#50525,#50526,
#50527,#50528,#50529,#50530,#50531,#50532,#50533,#50534),(#50535,#50536,
#50537,#50538,#50539,#50540,#50541,#50542,#50543,#50544,#50545,#50546,#50547,
#50548,#50549,#50550,#50551,#50552,#50553,#50554,#50555,#50556,#50557,#50558,
#50559,#50560,#50561,#50562,#50563,#50564,#50565,#50566,#50567,#50568,#50569),
(#50570,#50571,#50572,#50573,#50574,#50575,#50576,#50577,#50578,#50579,
#50580,#50581,#50582,#50583,#50584,#50585,#50586,#50587,#50588,#50589,#50590,
#50591,#50592,#50593,#50594,#50595,#50596,#50597,#50598,#50599,#50600,#50601,
#50602,#50603,#50604),(#50605,#50606,#50607,#50608,#50609,#50610,#50611,
#50612,#50613,#50614,#50615,#50616,#50617,#50618,#50619,#50620,#50621,#50622,
#50623,#50624,#50625,#50626,#50627,#50628,#50629,#50630,#50631,#50632,#50633,
#50634,#50635,#50636,#50637,#50638,#50639)),.UNSPECIFIED.,.F.,.F.,.F.,(4,
4),(4,1,1,1,1,1,1,1,1,1,1,1,1,1,1,1,1,1,1,1,1,1,1,1,1,1,1,1,1,1,1,1,4),
(-0.1117758545036,1.111775854504),(0.2466092045778,0.2706143034515,0.2946194023253,
0.318624501199,0.3426296000728,0.3666346989465,0.3906397978203,0.414644896694,
0.4386499955678,0.4626550944415,0.4866601933153,0.510665292189,0.5346703910628,
0.5586754899365,0.5826805888103,0.606685687684,0.6306907865577,0.6546958854315,
0.6787009843052,0.702706083179,0.7267111820527,0.7507162809265,0.7747213798002,
0.798726478674,0.8227315775477,0.8467366764215,0.8707417752952,0.894746874169,
0.9187519730427,0.9427570719165,0.9667621707902,0.9907672696639,1.014772368538),
 .UNSPECIFIED.);
#406=B_SPLINE_SURFACE_WITH_KNOTS('',3,3,((#50641,#50642,#50643,#50644,#50645,
#50646,#50647,#50648,#50649,#50650,#50651,#50652,#50653,#50654,#50655,#50656,
#50657,#50658,#50659,#50660,#50661,#50662,#50663,#50664,#50665,#50666,#50667,
#50668,#50669,#50670,#50671,#50672,#50673,#50674,#50675,#50676,#50677,#50678,
#50679,#50680,#50681,#50682,#50683,#50684,#50685,#50686,#50687,#50688,#50689,
#50690,#50691,#50692,#50693,#50694,#50695,#50696,#50697,#50698,#50699,#50700,
#50701,#50702,#50703,#50704,#50705,#50706,#50707),(#50708,#50709,#50710,
#50711,#50712,#50713,#50714,#50715,#50716,#50717,#50718,#50719,#50720,#50721,
#50722,#50723,#50724,#50725,#50726,#50727,#50728,#50729,#50730,#50731,#50732,
#50733,#50734,#50735,#50736,#50737,#50738,#50739,#50740,#50741,#50742,#50743,
#50744,#50745,#50746,#50747,#50748,#50749,#50750,#50751,#50752,#50753,#50754,
#50755,#50756,#50757,#50758,#50759,#50760,#50761,#50762,#50763,#50764,#50765,
#50766,#50767,#50768,#50769,#50770,#50771,#50772,#50773,#50774),(#50775,
#50776,#50777,#50778,#50779,#50780,#50781,#50782,#50783,#50784,#50785,#50786,
#50787,#50788,#50789,#50790,#50791,#50792,#50793,#50794,#50795,#50796,#50797,
#50798,#50799,#50800,#50801,#50802,#50803,#50804,#50805,#50806,#50807,#50808,
#50809,#50810,#50811,#50812,#50813,#50814,#50815,#50816,#50817,#50818,#50819,
#50820,#50821,#50822,#50823,#50824,#50825,#50826,#50827,#50828,#50829,#50830,
#50831,#50832,#50833,#50834,#50835,#50836,#50837,#50838,#50839,#50840,#50841),
(#50842,#50843,#50844,#50845,#50846,#50847,#50848,#50849,#50850,#50851,
#50852,#50853,#50854,#50855,#50856,#50857,#50858,#50859,#50860,#50861,#50862,
#50863,#50864,#50865,#50866,#50867,#50868,#50869,#50870,#50871,#50872,#50873,
#50874,#50875,#50876,#50877,#50878,#50879,#50880,#50881,#50882,#50883,#50884,
#50885,#50886,#50887,#50888,#50889,#50890,#50891,#50892,#50893,#50894,#50895,
#50896,#50897,#50898,#50899,#50900,#50901,#50902,#50903,#50904,#50905,#50906,
#50907,#50908)),.UNSPECIFIED.,.F.,.F.,.F.,(4,4),(4,1,1,1,1,1,1,1,1,1,1,
1,1,1,1,1,1,1,1,1,1,1,1,1,1,1,1,1,1,1,1,1,1,1,1,1,1,1,1,1,1,1,1,1,1,1,1,
1,1,1,1,1,1,1,1,1,1,1,1,1,1,1,1,1,4),(-0.1117758545036,1.111775854504),
(-0.02,-0.00375,0.0125,0.02875,0.045,0.06125,0.0775,0.09375,0.11,0.12625,
0.1425,0.15875,0.175,0.19125,0.2075,0.22375,0.24,0.25625,0.2725,0.28875,
0.305,0.32125,0.3375,0.35375,0.37,0.38625,0.4025,0.41875,0.435,0.45125,
0.4675,0.48375,0.5,0.51625,0.5325,0.54875,0.565,0.58125,0.5975,0.61375,
0.63,0.64625,0.6625,0.67875,0.695,0.71125,0.7275,0.74375,0.76,0.77625,0.7925,
0.80875,0.825,0.84125,0.8575,0.87375,0.89,0.90625,0.9225,0.93875,0.955,
0.97125,0.9875,1.00375,1.02),.UNSPECIFIED.);
#407=B_SPLINE_SURFACE_WITH_KNOTS('',3,3,((#50910,#50911,#50912,#50913,#50914,
#50915,#50916,#50917,#50918,#50919,#50920,#50921,#50922,#50923,#50924,#50925,
#50926,#50927,#50928,#50929,#50930,#50931,#50932,#50933,#50934,#50935,#50936,
#50937,#50938,#50939,#50940,#50941,#50942,#50943,#50944,#50945,#50946,#50947,
#50948,#50949,#50950,#50951,#50952,#50953,#50954,#50955,#50956,#50957,#50958,
#50959,#50960,#50961,#50962,#50963,#50964,#50965,#50966,#50967,#50968,#50969,
#50970,#50971,#50972,#50973,#50974,#50975,#50976),(#50977,#50978,#50979,
#50980,#50981,#50982,#50983,#50984,#50985,#50986,#50987,#50988,#50989,#50990,
#50991,#50992,#50993,#50994,#50995,#50996,#50997,#50998,#50999,#51000,#51001,
#51002,#51003,#51004,#51005,#51006,#51007,#51008,#51009,#51010,#51011,#51012,
#51013,#51014,#51015,#51016,#51017,#51018,#51019,#51020,#51021,#51022,#51023,
#51024,#51025,#51026,#51027,#51028,#51029,#51030,#51031,#51032,#51033,#51034,
#51035,#51036,#51037,#51038,#51039,#51040,#51041,#51042,#51043),(#51044,
#51045,#51046,#51047,#51048,#51049,#51050,#51051,#51052,#51053,#51054,#51055,
#51056,#51057,#51058,#51059,#51060,#51061,#51062,#51063,#51064,#51065,#51066,
#51067,#51068,#51069,#51070,#51071,#51072,#51073,#51074,#51075,#51076,#51077,
#51078,#51079,#51080,#51081,#51082,#51083,#51084,#51085,#51086,#51087,#51088,
#51089,#51090,#51091,#51092,#51093,#51094,#51095,#51096,#51097,#51098,#51099,
#51100,#51101,#51102,#51103,#51104,#51105,#51106,#51107,#51108,#51109,#51110),
(#51111,#51112,#51113,#51114,#51115,#51116,#51117,#51118,#51119,#51120,
#51121,#51122,#51123,#51124,#51125,#51126,#51127,#51128,#51129,#51130,#51131,
#51132,#51133,#51134,#51135,#51136,#51137,#51138,#51139,#51140,#51141,#51142,
#51143,#51144,#51145,#51146,#51147,#51148,#51149,#51150,#51151,#51152,#51153,
#51154,#51155,#51156,#51157,#51158,#51159,#51160,#51161,#51162,#51163,#51164,
#51165,#51166,#51167,#51168,#51169,#51170,#51171,#51172,#51173,#51174,#51175,
#51176,#51177)),.UNSPECIFIED.,.F.,.F.,.F.,(4,4),(4,1,1,1,1,1,1,1,1,1,1,
1,1,1,1,1,1,1,1,1,1,1,1,1,1,1,1,1,1,1,1,1,1,1,1,1,1,1,1,1,1,1,1,1,1,1,1,
1,1,1,1,1,1,1,1,1,1,1,1,1,1,1,1,1,4),(-0.1117758545037,1.111775854504),
(-0.02,-0.00375,0.0125,0.02875,0.045,0.06125,0.0775,0.09375,0.11,0.12625,
0.1425,0.15875,0.175,0.19125,0.2075,0.22375,0.24,0.25625,0.2725,0.28875,
0.305,0.32125,0.3375,0.35375,0.37,0.38625,0.4025,0.41875,0.435,0.45125,
0.4675,0.48375,0.5,0.51625,0.5325,0.54875,0.565,0.58125,0.5975,0.61375,
0.63,0.64625,0.6625,0.67875,0.695,0.71125,0.7275,0.74375,0.76,0.77625,0.7925,
0.80875,0.825,0.84125,0.8575,0.87375,0.89,0.90625,0.9225,0.93875,0.955,
0.97125,0.9875,1.00375,1.02),.UNSPECIFIED.);
#408=B_SPLINE_SURFACE_WITH_KNOTS('',3,3,((#51791,#51792,#51793,#51794,#51795,
#51796,#51797,#51798,#51799,#51800,#51801,#51802,#51803,#51804,#51805,#51806,
#51807,#51808,#51809,#51810,#51811,#51812,#51813,#51814,#51815,#51816,#51817,
#51818,#51819,#51820,#51821,#51822,#51823,#51824,#51825,#51826,#51827,#51828,
#51829,#51830,#51831,#51832,#51833,#51834,#51835,#51836,#51837,#51838,#51839,
#51840,#51841,#51842,#51843,#51844,#51845,#51846,#51847,#51848,#51849,#51850,
#51851,#51852,#51853,#51854,#51855,#51856,#51857),(#51858,#51859,#51860,
#51861,#51862,#51863,#51864,#51865,#51866,#51867,#51868,#51869,#51870,#51871,
#51872,#51873,#51874,#51875,#51876,#51877,#51878,#51879,#51880,#51881,#51882,
#51883,#51884,#51885,#51886,#51887,#51888,#51889,#51890,#51891,#51892,#51893,
#51894,#51895,#51896,#51897,#51898,#51899,#51900,#51901,#51902,#51903,#51904,
#51905,#51906,#51907,#51908,#51909,#51910,#51911,#51912,#51913,#51914,#51915,
#51916,#51917,#51918,#51919,#51920,#51921,#51922,#51923,#51924),(#51925,
#51926,#51927,#51928,#51929,#51930,#51931,#51932,#51933,#51934,#51935,#51936,
#51937,#51938,#51939,#51940,#51941,#51942,#51943,#51944,#51945,#51946,#51947,
#51948,#51949,#51950,#51951,#51952,#51953,#51954,#51955,#51956,#51957,#51958,
#51959,#51960,#51961,#51962,#51963,#51964,#51965,#51966,#51967,#51968,#51969,
#51970,#51971,#51972,#51973,#51974,#51975,#51976,#51977,#51978,#51979,#51980,
#51981,#51982,#51983,#51984,#51985,#51986,#51987,#51988,#51989,#51990,#51991),
(#51992,#51993,#51994,#51995,#51996,#51997,#51998,#51999,#52000,#52001,
#52002,#52003,#52004,#52005,#52006,#52007,#52008,#52009,#52010,#52011,#52012,
#52013,#52014,#52015,#52016,#52017,#52018,#52019,#52020,#52021,#52022,#52023,
#52024,#52025,#52026,#52027,#52028,#52029,#52030,#52031,#52032,#52033,#52034,
#52035,#52036,#52037,#52038,#52039,#52040,#52041,#52042,#52043,#52044,#52045,
#52046,#52047,#52048,#52049,#52050,#52051,#52052,#52053,#52054,#52055,#52056,
#52057,#52058)),.UNSPECIFIED.,.F.,.F.,.F.,(4,4),(4,1,1,1,1,1,1,1,1,1,1,
1,1,1,1,1,1,1,1,1,1,1,1,1,1,1,1,1,1,1,1,1,1,1,1,1,1,1,1,1,1,1,1,1,1,1,1,
1,1,1,1,1,1,1,1,1,1,1,1,1,1,1,1,1,4),(-0.04605142190376,1.046051421904),
(-0.02,-0.00375,0.0125,0.02875,0.045,0.06125,0.0775,0.09375,0.11,0.12625,
0.1425,0.15875,0.175,0.19125,0.2075,0.22375,0.24,0.25625,0.2725,0.28875,
0.305,0.32125,0.3375,0.35375,0.37,0.38625,0.4025,0.41875,0.435,0.45125,
0.4675,0.48375,0.5,0.51625,0.5325,0.54875,0.565,0.58125,0.5975,0.61375,
0.63,0.64625,0.6625,0.67875,0.695,0.71125,0.7275,0.74375,0.76,0.77625,0.7925,
0.80875,0.825,0.84125,0.8575,0.87375,0.89,0.90625,0.9225,0.93875,0.955,
0.97125,0.9875,1.00375,1.02),.UNSPECIFIED.);
#409=PLANE('',#9283);
#410=PLANE('',#9286);
#411=PLANE('',#9287);
#412=PLANE('',#9290);
#413=PLANE('',#9291);
#414=PLANE('',#9293);
#415=PLANE('',#9295);
#416=PLANE('',#9303);
#417=PLANE('',#9400);
#418=PLANE('',#9401);
#419=PLANE('',#9402);
#420=PLANE('',#9403);
#421=PLANE('',#9404);
#422=PLANE('',#9405);
#423=PLANE('',#9406);
#424=PLANE('',#9410);
#425=PLANE('',#9668);
#426=PLANE('',#9680);
#427=PLANE('',#9681);
#428=PLANE('',#9682);
#429=PLANE('',#9683);
#430=PLANE('',#9684);
#431=PLANE('',#9685);
#432=PLANE('',#9686);
#433=PLANE('',#9689);
#434=PLANE('',#9690);
#435=PLANE('',#9693);
#436=PLANE('',#9695);
#437=PLANE('',#9700);
#438=PLANE('',#9707);
#439=PLANE('',#9718);
#440=PLANE('',#9719);
#441=PLANE('',#9731);
#442=PLANE('',#9734);
#443=PLANE('',#9746);
#444=PLANE('',#9747);
#445=PLANE('',#9749);
#446=PLANE('',#9751);
#447=PLANE('',#9753);
#448=PLANE('',#9755);
#449=PLANE('',#9757);
#450=PLANE('',#9759);
#451=PLANE('',#9761);
#452=PLANE('',#9764);
#453=PLANE('',#9766);
#454=PLANE('',#9768);
#455=PLANE('',#9770);
#456=PLANE('',#9772);
#457=PLANE('',#9774);
#458=PLANE('',#9777);
#459=PLANE('',#9783);
#460=PLANE('',#9786);
#461=PLANE('',#9789);
#462=PLANE('',#9792);
#463=PLANE('',#9812);
#464=PLANE('',#9884);
#465=PLANE('',#9892);
#466=PLANE('',#9909);
#467=PLANE('',#9913);
#468=PLANE('',#9922);
#469=PLANE('',#9948);
#470=PLANE('',#9949);
#471=PLANE('',#9952);
#472=PLANE('',#9953);
#473=PLANE('',#9965);
#474=PLANE('',#9967);
#475=PLANE('',#9969);
#476=PLANE('',#9971);
#477=PLANE('',#9973);
#478=PLANE('',#9975);
#479=PLANE('',#9977);
#480=PLANE('',#9979);
#481=PLANE('',#9981);
#482=PLANE('',#9984);
#483=PLANE('',#9986);
#484=PLANE('',#9988);
#485=PLANE('',#9997);
#486=PLANE('',#10004);
#487=PLANE('',#10005);
#488=PLANE('',#10006);
#489=PLANE('',#10010);
#490=PLANE('',#10014);
#491=PLANE('',#10023);
#492=PLANE('',#10041);
#493=PLANE('',#10052);
#494=PLANE('',#10067);
#495=PLANE('',#10086);
#496=PLANE('',#10091);
#497=PLANE('',#10095);
#498=PLANE('',#10100);
#499=PLANE('',#10101);
#500=PLANE('',#10107);
#501=PLANE('',#10114);
#502=PLANE('',#10118);
#503=PLANE('',#10133);
#504=PLANE('',#10138);
#505=PLANE('',#10143);
#506=PLANE('',#10147);
#507=PLANE('',#10151);
#508=PLANE('',#10159);
#509=PLANE('',#10160);
#510=PLANE('',#10162);
#511=PLANE('',#10164);
#512=PLANE('',#10166);
#513=PLANE('',#10168);
#514=PLANE('',#10170);
#515=PLANE('',#10176);
#516=PLANE('',#10181);
#517=PLANE('',#10185);
#518=FACE_OUTER_BOUND('',#1055,.T.);
#519=FACE_OUTER_BOUND('',#1056,.T.);
#520=FACE_OUTER_BOUND('',#1057,.T.);
#521=FACE_OUTER_BOUND('',#1058,.T.);
#522=FACE_OUTER_BOUND('',#1059,.T.);
#523=FACE_OUTER_BOUND('',#1060,.T.);
#524=FACE_OUTER_BOUND('',#1061,.T.);
#525=FACE_OUTER_BOUND('',#1062,.T.);
#526=FACE_OUTER_BOUND('',#1063,.T.);
#527=FACE_OUTER_BOUND('',#1064,.T.);
#528=FACE_OUTER_BOUND('',#1065,.T.);
#529=FACE_OUTER_BOUND('',#1066,.T.);
#530=FACE_OUTER_BOUND('',#1067,.T.);
#531=FACE_OUTER_BOUND('',#1068,.T.);
#532=FACE_OUTER_BOUND('',#1069,.T.);
#533=FACE_OUTER_BOUND('',#1070,.T.);
#534=FACE_OUTER_BOUND('',#1071,.T.);
#535=FACE_OUTER_BOUND('',#1073,.T.);
#536=FACE_OUTER_BOUND('',#1074,.T.);
#537=FACE_OUTER_BOUND('',#1075,.T.);
#538=FACE_OUTER_BOUND('',#1076,.T.);
#539=FACE_OUTER_BOUND('',#1077,.T.);
#540=FACE_OUTER_BOUND('',#1078,.T.);
#541=FACE_OUTER_BOUND('',#1079,.T.);
#542=FACE_OUTER_BOUND('',#1080,.T.);
#543=FACE_OUTER_BOUND('',#1081,.T.);
#544=FACE_OUTER_BOUND('',#1082,.T.);
#545=FACE_OUTER_BOUND('',#1083,.T.);
#546=FACE_OUTER_BOUND('',#1084,.T.);
#547=FACE_OUTER_BOUND('',#1085,.T.);
#548=FACE_OUTER_BOUND('',#1086,.T.);
#549=FACE_OUTER_BOUND('',#1087,.T.);
#550=FACE_OUTER_BOUND('',#1088,.T.);
#551=FACE_OUTER_BOUND('',#1089,.T.);
#552=FACE_OUTER_BOUND('',#1090,.T.);
#553=FACE_OUTER_BOUND('',#1092,.T.);
#554=FACE_OUTER_BOUND('',#1093,.T.);
#555=FACE_OUTER_BOUND('',#1094,.T.);
#556=FACE_OUTER_BOUND('',#1096,.T.);
#557=FACE_OUTER_BOUND('',#1097,.T.);
#558=FACE_OUTER_BOUND('',#1098,.T.);
#559=FACE_OUTER_BOUND('',#1099,.T.);
#560=FACE_OUTER_BOUND('',#1100,.T.);
#561=FACE_OUTER_BOUND('',#1101,.T.);
#562=FACE_OUTER_BOUND('',#1102,.T.);
#563=FACE_OUTER_BOUND('',#1104,.T.);
#564=FACE_OUTER_BOUND('',#1105,.T.);
#565=FACE_OUTER_BOUND('',#1107,.T.);
#566=FACE_OUTER_BOUND('',#1108,.T.);
#567=FACE_OUTER_BOUND('',#1109,.T.);
#568=FACE_OUTER_BOUND('',#1110,.T.);
#569=FACE_OUTER_BOUND('',#1111,.T.);
#570=FACE_OUTER_BOUND('',#1112,.T.);
#571=FACE_OUTER_BOUND('',#1113,.T.);
#572=FACE_OUTER_BOUND('',#1114,.T.);
#573=FACE_OUTER_BOUND('',#1115,.T.);
#574=FACE_OUTER_BOUND('',#1116,.T.);
#575=FACE_OUTER_BOUND('',#1117,.T.);
#576=FACE_OUTER_BOUND('',#1118,.T.);
#577=FACE_OUTER_BOUND('',#1119,.T.);
#578=FACE_OUTER_BOUND('',#1120,.T.);
#579=FACE_OUTER_BOUND('',#1121,.T.);
#580=FACE_OUTER_BOUND('',#1122,.T.);
#581=FACE_OUTER_BOUND('',#1123,.T.);
#582=FACE_OUTER_BOUND('',#1124,.T.);
#583=FACE_OUTER_BOUND('',#1125,.T.);
#584=FACE_OUTER_BOUND('',#1126,.T.);
#585=FACE_OUTER_BOUND('',#1127,.T.);
#586=FACE_OUTER_BOUND('',#1128,.T.);
#587=FACE_OUTER_BOUND('',#1129,.T.);
#588=FACE_OUTER_BOUND('',#1130,.T.);
#589=FACE_OUTER_BOUND('',#1131,.T.);
#590=FACE_OUTER_BOUND('',#1132,.T.);
#591=FACE_OUTER_BOUND('',#1133,.T.);
#592=FACE_OUTER_BOUND('',#1134,.T.);
#593=FACE_OUTER_BOUND('',#1135,.T.);
#594=FACE_OUTER_BOUND('',#1136,.T.);
#595=FACE_OUTER_BOUND('',#1137,.T.);
#596=FACE_OUTER_BOUND('',#1138,.T.);
#597=FACE_OUTER_BOUND('',#1139,.T.);
#598=FACE_OUTER_BOUND('',#1140,.T.);
#599=FACE_OUTER_BOUND('',#1141,.T.);
#600=FACE_OUTER_BOUND('',#1142,.T.);
#601=FACE_OUTER_BOUND('',#1143,.T.);
#602=FACE_OUTER_BOUND('',#1144,.T.);
#603=FACE_OUTER_BOUND('',#1145,.T.);
#604=FACE_OUTER_BOUND('',#1146,.T.);
#605=FACE_OUTER_BOUND('',#1147,.T.);
#606=FACE_OUTER_BOUND('',#1148,.T.);
#607=FACE_OUTER_BOUND('',#1149,.T.);
#608=FACE_OUTER_BOUND('',#1150,.T.);
#609=FACE_OUTER_BOUND('',#1151,.T.);
#610=FACE_OUTER_BOUND('',#1152,.T.);
#611=FACE_OUTER_BOUND('',#1153,.T.);
#612=FACE_OUTER_BOUND('',#1154,.T.);
#613=FACE_OUTER_BOUND('',#1155,.T.);
#614=FACE_OUTER_BOUND('',#1156,.T.);
#615=FACE_OUTER_BOUND('',#1157,.T.);
#616=FACE_OUTER_BOUND('',#1158,.T.);
#617=FACE_OUTER_BOUND('',#1159,.T.);
#618=FACE_OUTER_BOUND('',#1160,.T.);
#619=FACE_OUTER_BOUND('',#1161,.T.);
#620=FACE_OUTER_BOUND('',#1162,.T.);
#621=FACE_OUTER_BOUND('',#1163,.T.);
#622=FACE_OUTER_BOUND('',#1164,.T.);
#623=FACE_OUTER_BOUND('',#1165,.T.);
#624=FACE_OUTER_BOUND('',#1166,.T.);
#625=FACE_OUTER_BOUND('',#1167,.T.);
#626=FACE_OUTER_BOUND('',#1168,.T.);
#627=FACE_OUTER_BOUND('',#1169,.T.);
#628=FACE_OUTER_BOUND('',#1170,.T.);
#629=FACE_OUTER_BOUND('',#1171,.T.);
#630=FACE_OUTER_BOUND('',#1172,.T.);
#631=FACE_OUTER_BOUND('',#1173,.T.);
#632=FACE_OUTER_BOUND('',#1174,.T.);
#633=FACE_OUTER_BOUND('',#1175,.T.);
#634=FACE_OUTER_BOUND('',#1176,.T.);
#635=FACE_OUTER_BOUND('',#1177,.T.);
#636=FACE_OUTER_BOUND('',#1178,.T.);
#637=FACE_OUTER_BOUND('',#1179,.T.);
#638=FACE_OUTER_BOUND('',#1180,.T.);
#639=FACE_OUTER_BOUND('',#1181,.T.);
#640=FACE_OUTER_BOUND('',#1182,.T.);
#641=FACE_OUTER_BOUND('',#1183,.T.);
#642=FACE_OUTER_BOUND('',#1184,.T.);
#643=FACE_OUTER_BOUND('',#1185,.T.);
#644=FACE_OUTER_BOUND('',#1186,.T.);
#645=FACE_OUTER_BOUND('',#1187,.T.);
#646=FACE_OUTER_BOUND('',#1188,.T.);
#647=FACE_OUTER_BOUND('',#1189,.T.);
#648=FACE_OUTER_BOUND('',#1190,.T.);
#649=FACE_OUTER_BOUND('',#1191,.T.);
#650=FACE_OUTER_BOUND('',#1192,.T.);
#651=FACE_OUTER_BOUND('',#1193,.T.);
#652=FACE_OUTER_BOUND('',#1194,.T.);
#653=FACE_OUTER_BOUND('',#1195,.T.);
#654=FACE_OUTER_BOUND('',#1196,.T.);
#655=FACE_OUTER_BOUND('',#1197,.T.);
#656=FACE_OUTER_BOUND('',#1198,.T.);
#657=FACE_OUTER_BOUND('',#1199,.T.);
#658=FACE_OUTER_BOUND('',#1200,.T.);
#659=FACE_OUTER_BOUND('',#1201,.T.);
#660=FACE_OUTER_BOUND('',#1202,.T.);
#661=FACE_OUTER_BOUND('',#1203,.T.);
#662=FACE_OUTER_BOUND('',#1204,.T.);
#663=FACE_OUTER_BOUND('',#1205,.T.);
#664=FACE_OUTER_BOUND('',#1206,.T.);
#665=FACE_OUTER_BOUND('',#1207,.T.);
#666=FACE_OUTER_BOUND('',#1208,.T.);
#667=FACE_OUTER_BOUND('',#1209,.T.);
#668=FACE_OUTER_BOUND('',#1210,.T.);
#669=FACE_OUTER_BOUND('',#1211,.T.);
#670=FACE_OUTER_BOUND('',#1212,.T.);
#671=FACE_OUTER_BOUND('',#1213,.T.);
#672=FACE_OUTER_BOUND('',#1214,.T.);
#673=FACE_OUTER_BOUND('',#1215,.T.);
#674=FACE_OUTER_BOUND('',#1216,.T.);
#675=FACE_OUTER_BOUND('',#1217,.T.);
#676=FACE_OUTER_BOUND('',#1218,.T.);
#677=FACE_OUTER_BOUND('',#1219,.T.);
#678=FACE_OUTER_BOUND('',#1220,.T.);
#679=FACE_OUTER_BOUND('',#1221,.T.);
#680=FACE_OUTER_BOUND('',#1222,.T.);
#681=FACE_OUTER_BOUND('',#1223,.T.);
#682=FACE_OUTER_BOUND('',#1224,.T.);
#683=FACE_OUTER_BOUND('',#1225,.T.);
#684=FACE_OUTER_BOUND('',#1226,.T.);
#685=FACE_OUTER_BOUND('',#1227,.T.);
#686=FACE_OUTER_BOUND('',#1228,.T.);
#687=FACE_OUTER_BOUND('',#1229,.T.);
#688=FACE_OUTER_BOUND('',#1230,.T.);
#689=FACE_OUTER_BOUND('',#1231,.T.);
#690=FACE_OUTER_BOUND('',#1232,.T.);
#691=FACE_OUTER_BOUND('',#1233,.T.);
#692=FACE_OUTER_BOUND('',#1234,.T.);
#693=FACE_OUTER_BOUND('',#1235,.T.);
#694=FACE_OUTER_BOUND('',#1237,.T.);
#695=FACE_OUTER_BOUND('',#1238,.T.);
#696=FACE_OUTER_BOUND('',#1239,.T.);
#697=FACE_OUTER_BOUND('',#1242,.T.);
#698=FACE_OUTER_BOUND('',#1243,.T.);
#699=FACE_OUTER_BOUND('',#1244,.T.);
#700=FACE_OUTER_BOUND('',#1245,.T.);
#701=FACE_OUTER_BOUND('',#1246,.T.);
#702=FACE_OUTER_BOUND('',#1247,.T.);
#703=FACE_OUTER_BOUND('',#1248,.T.);
#704=FACE_OUTER_BOUND('',#1249,.T.);
#705=FACE_OUTER_BOUND('',#1250,.T.);
#706=FACE_OUTER_BOUND('',#1252,.T.);
#707=FACE_OUTER_BOUND('',#1253,.T.);
#708=FACE_OUTER_BOUND('',#1254,.T.);
#709=FACE_OUTER_BOUND('',#1255,.T.);
#710=FACE_OUTER_BOUND('',#1256,.T.);
#711=FACE_OUTER_BOUND('',#1257,.T.);
#712=FACE_OUTER_BOUND('',#1258,.T.);
#713=FACE_OUTER_BOUND('',#1259,.T.);
#714=FACE_OUTER_BOUND('',#1260,.T.);
#715=FACE_OUTER_BOUND('',#1261,.T.);
#716=FACE_OUTER_BOUND('',#1262,.T.);
#717=FACE_OUTER_BOUND('',#1263,.T.);
#718=FACE_OUTER_BOUND('',#1264,.T.);
#719=FACE_OUTER_BOUND('',#1265,.T.);
#720=FACE_OUTER_BOUND('',#1266,.T.);
#721=FACE_OUTER_BOUND('',#1267,.T.);
#722=FACE_OUTER_BOUND('',#1268,.T.);
#723=FACE_OUTER_BOUND('',#1269,.T.);
#724=FACE_OUTER_BOUND('',#1270,.T.);
#725=FACE_OUTER_BOUND('',#1271,.T.);
#726=FACE_OUTER_BOUND('',#1272,.T.);
#727=FACE_OUTER_BOUND('',#1274,.T.);
#728=FACE_OUTER_BOUND('',#1275,.T.);
#729=FACE_OUTER_BOUND('',#1277,.T.);
#730=FACE_OUTER_BOUND('',#1278,.T.);
#731=FACE_OUTER_BOUND('',#1279,.T.);
#732=FACE_OUTER_BOUND('',#1280,.T.);
#733=FACE_OUTER_BOUND('',#1281,.T.);
#734=FACE_OUTER_BOUND('',#1282,.T.);
#735=FACE_OUTER_BOUND('',#1283,.T.);
#736=FACE_OUTER_BOUND('',#1284,.T.);
#737=FACE_OUTER_BOUND('',#1285,.T.);
#738=FACE_OUTER_BOUND('',#1286,.T.);
#739=FACE_OUTER_BOUND('',#1287,.T.);
#740=FACE_OUTER_BOUND('',#1288,.T.);
#741=FACE_OUTER_BOUND('',#1289,.T.);
#742=FACE_OUTER_BOUND('',#1290,.T.);
#743=FACE_OUTER_BOUND('',#1291,.T.);
#744=FACE_OUTER_BOUND('',#1292,.T.);
#745=FACE_OUTER_BOUND('',#1293,.T.);
#746=FACE_OUTER_BOUND('',#1294,.T.);
#747=FACE_OUTER_BOUND('',#1295,.T.);
#748=FACE_OUTER_BOUND('',#1296,.T.);
#749=FACE_OUTER_BOUND('',#1297,.T.);
#750=FACE_OUTER_BOUND('',#1299,.T.);
#751=FACE_OUTER_BOUND('',#1300,.T.);
#752=FACE_OUTER_BOUND('',#1301,.T.);
#753=FACE_OUTER_BOUND('',#1302,.T.);
#754=FACE_OUTER_BOUND('',#1303,.T.);
#755=FACE_OUTER_BOUND('',#1304,.T.);
#756=FACE_OUTER_BOUND('',#1305,.T.);
#757=FACE_OUTER_BOUND('',#1306,.T.);
#758=FACE_OUTER_BOUND('',#1307,.T.);
#759=FACE_OUTER_BOUND('',#1308,.T.);
#760=FACE_OUTER_BOUND('',#1309,.T.);
#761=FACE_OUTER_BOUND('',#1310,.T.);
#762=FACE_OUTER_BOUND('',#1311,.T.);
#763=FACE_OUTER_BOUND('',#1312,.T.);
#764=FACE_OUTER_BOUND('',#1313,.T.);
#765=FACE_OUTER_BOUND('',#1314,.T.);
#766=FACE_OUTER_BOUND('',#1315,.T.);
#767=FACE_OUTER_BOUND('',#1316,.T.);
#768=FACE_OUTER_BOUND('',#1317,.T.);
#769=FACE_OUTER_BOUND('',#1318,.T.);
#770=FACE_OUTER_BOUND('',#1319,.T.);
#771=FACE_OUTER_BOUND('',#1320,.T.);
#772=FACE_OUTER_BOUND('',#1321,.T.);
#773=FACE_OUTER_BOUND('',#1322,.T.);
#774=FACE_OUTER_BOUND('',#1323,.T.);
#775=FACE_OUTER_BOUND('',#1324,.T.);
#776=FACE_OUTER_BOUND('',#1325,.T.);
#777=FACE_OUTER_BOUND('',#1326,.T.);
#778=FACE_OUTER_BOUND('',#1327,.T.);
#779=FACE_OUTER_BOUND('',#1328,.T.);
#780=FACE_OUTER_BOUND('',#1329,.T.);
#781=FACE_OUTER_BOUND('',#1330,.T.);
#782=FACE_OUTER_BOUND('',#1331,.T.);
#783=FACE_OUTER_BOUND('',#1332,.T.);
#784=FACE_OUTER_BOUND('',#1333,.T.);
#785=FACE_OUTER_BOUND('',#1334,.T.);
#786=FACE_OUTER_BOUND('',#1335,.T.);
#787=FACE_OUTER_BOUND('',#1336,.T.);
#788=FACE_OUTER_BOUND('',#1337,.T.);
#789=FACE_OUTER_BOUND('',#1338,.T.);
#790=FACE_OUTER_BOUND('',#1339,.T.);
#791=FACE_OUTER_BOUND('',#1340,.T.);
#792=FACE_OUTER_BOUND('',#1341,.T.);
#793=FACE_OUTER_BOUND('',#1342,.T.);
#794=FACE_OUTER_BOUND('',#1343,.T.);
#795=FACE_OUTER_BOUND('',#1344,.T.);
#796=FACE_OUTER_BOUND('',#1345,.T.);
#797=FACE_OUTER_BOUND('',#1346,.T.);
#798=FACE_OUTER_BOUND('',#1347,.T.);
#799=FACE_OUTER_BOUND('',#1348,.T.);
#800=FACE_OUTER_BOUND('',#1349,.T.);
#801=FACE_OUTER_BOUND('',#1350,.T.);
#802=FACE_OUTER_BOUND('',#1351,.T.);
#803=FACE_OUTER_BOUND('',#1352,.T.);
#804=FACE_OUTER_BOUND('',#1353,.T.);
#805=FACE_OUTER_BOUND('',#1354,.T.);
#806=FACE_OUTER_BOUND('',#1355,.T.);
#807=FACE_OUTER_BOUND('',#1356,.T.);
#808=FACE_OUTER_BOUND('',#1357,.T.);
#809=FACE_OUTER_BOUND('',#1358,.T.);
#810=FACE_OUTER_BOUND('',#1359,.T.);
#811=FACE_OUTER_BOUND('',#1360,.T.);
#812=FACE_OUTER_BOUND('',#1361,.T.);
#813=FACE_OUTER_BOUND('',#1362,.T.);
#814=FACE_OUTER_BOUND('',#1363,.T.);
#815=FACE_OUTER_BOUND('',#1364,.T.);
#816=FACE_OUTER_BOUND('',#1365,.T.);
#817=FACE_OUTER_BOUND('',#1366,.T.);
#818=FACE_OUTER_BOUND('',#1367,.T.);
#819=FACE_OUTER_BOUND('',#1368,.T.);
#820=FACE_OUTER_BOUND('',#1369,.T.);
#821=FACE_OUTER_BOUND('',#1370,.T.);
#822=FACE_OUTER_BOUND('',#1371,.T.);
#823=FACE_OUTER_BOUND('',#1372,.T.);
#824=FACE_OUTER_BOUND('',#1373,.T.);
#825=FACE_OUTER_BOUND('',#1374,.T.);
#826=FACE_OUTER_BOUND('',#1375,.T.);
#827=FACE_OUTER_BOUND('',#1376,.T.);
#828=FACE_OUTER_BOUND('',#1377,.T.);
#829=FACE_OUTER_BOUND('',#1378,.T.);
#830=FACE_OUTER_BOUND('',#1379,.T.);
#831=FACE_OUTER_BOUND('',#1380,.T.);
#832=FACE_OUTER_BOUND('',#1381,.T.);
#833=FACE_OUTER_BOUND('',#1382,.T.);
#834=FACE_OUTER_BOUND('',#1383,.T.);
#835=FACE_OUTER_BOUND('',#1384,.T.);
#836=FACE_OUTER_BOUND('',#1385,.T.);
#837=FACE_OUTER_BOUND('',#1386,.T.);
#838=FACE_OUTER_BOUND('',#1387,.T.);
#839=FACE_OUTER_BOUND('',#1388,.T.);
#840=FACE_OUTER_BOUND('',#1389,.T.);
#841=FACE_OUTER_BOUND('',#1390,.T.);
#842=FACE_OUTER_BOUND('',#1391,.T.);
#843=FACE_OUTER_BOUND('',#1392,.T.);
#844=FACE_OUTER_BOUND('',#1393,.T.);
#845=FACE_OUTER_BOUND('',#1394,.T.);
#846=FACE_OUTER_BOUND('',#1395,.T.);
#847=FACE_OUTER_BOUND('',#1396,.T.);
#848=FACE_OUTER_BOUND('',#1397,.T.);
#849=FACE_OUTER_BOUND('',#1398,.T.);
#850=FACE_OUTER_BOUND('',#1399,.T.);
#851=FACE_OUTER_BOUND('',#1401,.T.);
#852=FACE_OUTER_BOUND('',#1402,.T.);
#853=FACE_OUTER_BOUND('',#1403,.T.);
#854=FACE_OUTER_BOUND('',#1404,.T.);
#855=FACE_OUTER_BOUND('',#1405,.T.);
#856=FACE_OUTER_BOUND('',#1407,.T.);
#857=FACE_OUTER_BOUND('',#1408,.T.);
#858=FACE_OUTER_BOUND('',#1410,.T.);
#859=FACE_OUTER_BOUND('',#1411,.T.);
#860=FACE_OUTER_BOUND('',#1412,.T.);
#861=FACE_OUTER_BOUND('',#1413,.T.);
#862=FACE_OUTER_BOUND('',#1414,.T.);
#863=FACE_OUTER_BOUND('',#1415,.T.);
#864=FACE_OUTER_BOUND('',#1416,.T.);
#865=FACE_OUTER_BOUND('',#1417,.T.);
#866=FACE_OUTER_BOUND('',#1418,.T.);
#867=FACE_OUTER_BOUND('',#1419,.T.);
#868=FACE_OUTER_BOUND('',#1420,.T.);
#869=FACE_OUTER_BOUND('',#1421,.T.);
#870=FACE_OUTER_BOUND('',#1422,.T.);
#871=FACE_OUTER_BOUND('',#1423,.T.);
#872=FACE_OUTER_BOUND('',#1424,.T.);
#873=FACE_OUTER_BOUND('',#1426,.T.);
#874=FACE_OUTER_BOUND('',#1427,.T.);
#875=FACE_OUTER_BOUND('',#1428,.T.);
#876=FACE_OUTER_BOUND('',#1429,.T.);
#877=FACE_OUTER_BOUND('',#1430,.T.);
#878=FACE_OUTER_BOUND('',#1431,.T.);
#879=FACE_OUTER_BOUND('',#1432,.T.);
#880=FACE_OUTER_BOUND('',#1433,.T.);
#881=FACE_OUTER_BOUND('',#1434,.T.);
#882=FACE_OUTER_BOUND('',#1435,.T.);
#883=FACE_OUTER_BOUND('',#1436,.T.);
#884=FACE_OUTER_BOUND('',#1437,.T.);
#885=FACE_OUTER_BOUND('',#1438,.T.);
#886=FACE_OUTER_BOUND('',#1439,.T.);
#887=FACE_OUTER_BOUND('',#1440,.T.);
#888=FACE_OUTER_BOUND('',#1441,.T.);
#889=FACE_OUTER_BOUND('',#1442,.T.);
#890=FACE_OUTER_BOUND('',#1443,.T.);
#891=FACE_OUTER_BOUND('',#1444,.T.);
#892=FACE_OUTER_BOUND('',#1445,.T.);
#893=FACE_OUTER_BOUND('',#1446,.T.);
#894=FACE_OUTER_BOUND('',#1447,.T.);
#895=FACE_OUTER_BOUND('',#1448,.T.);
#896=FACE_OUTER_BOUND('',#1449,.T.);
#897=FACE_OUTER_BOUND('',#1450,.T.);
#898=FACE_OUTER_BOUND('',#1451,.T.);
#899=FACE_OUTER_BOUND('',#1452,.T.);
#900=FACE_OUTER_BOUND('',#1453,.T.);
#901=FACE_OUTER_BOUND('',#1454,.T.);
#902=FACE_OUTER_BOUND('',#1455,.T.);
#903=FACE_OUTER_BOUND('',#1456,.T.);
#904=FACE_OUTER_BOUND('',#1457,.T.);
#905=FACE_OUTER_BOUND('',#1458,.T.);
#906=FACE_OUTER_BOUND('',#1459,.T.);
#907=FACE_OUTER_BOUND('',#1460,.T.);
#908=FACE_OUTER_BOUND('',#1461,.T.);
#909=FACE_OUTER_BOUND('',#1462,.T.);
#910=FACE_OUTER_BOUND('',#1463,.T.);
#911=FACE_OUTER_BOUND('',#1464,.T.);
#912=FACE_OUTER_BOUND('',#1465,.T.);
#913=FACE_OUTER_BOUND('',#1466,.T.);
#914=FACE_OUTER_BOUND('',#1467,.T.);
#915=FACE_OUTER_BOUND('',#1468,.T.);
#916=FACE_OUTER_BOUND('',#1469,.T.);
#917=FACE_OUTER_BOUND('',#1470,.T.);
#918=FACE_OUTER_BOUND('',#1471,.T.);
#919=FACE_OUTER_BOUND('',#1472,.T.);
#920=FACE_OUTER_BOUND('',#1473,.T.);
#921=FACE_OUTER_BOUND('',#1474,.T.);
#922=FACE_OUTER_BOUND('',#1475,.T.);
#923=FACE_OUTER_BOUND('',#1476,.T.);
#924=FACE_OUTER_BOUND('',#1478,.T.);
#925=FACE_OUTER_BOUND('',#1479,.T.);
#926=FACE_OUTER_BOUND('',#1480,.T.);
#927=FACE_OUTER_BOUND('',#1482,.T.);
#928=FACE_OUTER_BOUND('',#1483,.T.);
#929=FACE_OUTER_BOUND('',#1484,.T.);
#930=FACE_OUTER_BOUND('',#1485,.T.);
#931=FACE_OUTER_BOUND('',#1486,.T.);
#932=FACE_OUTER_BOUND('',#1487,.T.);
#933=FACE_OUTER_BOUND('',#1488,.T.);
#934=FACE_OUTER_BOUND('',#1489,.T.);
#935=FACE_OUTER_BOUND('',#1490,.T.);
#936=FACE_OUTER_BOUND('',#1491,.T.);
#937=FACE_OUTER_BOUND('',#1492,.T.);
#938=FACE_OUTER_BOUND('',#1493,.T.);
#939=FACE_OUTER_BOUND('',#1494,.T.);
#940=FACE_OUTER_BOUND('',#1495,.T.);
#941=FACE_OUTER_BOUND('',#1496,.T.);
#942=FACE_OUTER_BOUND('',#1497,.T.);
#943=FACE_OUTER_BOUND('',#1498,.T.);
#944=FACE_OUTER_BOUND('',#1500,.T.);
#945=FACE_OUTER_BOUND('',#1502,.T.);
#946=FACE_OUTER_BOUND('',#1504,.T.);
#947=FACE_OUTER_BOUND('',#1505,.T.);
#948=FACE_OUTER_BOUND('',#1508,.T.);
#949=FACE_OUTER_BOUND('',#1509,.T.);
#950=FACE_OUTER_BOUND('',#1511,.T.);
#951=FACE_OUTER_BOUND('',#1512,.T.);
#952=FACE_OUTER_BOUND('',#1513,.T.);
#953=FACE_OUTER_BOUND('',#1514,.T.);
#954=FACE_OUTER_BOUND('',#1515,.T.);
#955=FACE_OUTER_BOUND('',#1516,.T.);
#956=FACE_OUTER_BOUND('',#1517,.T.);
#957=FACE_OUTER_BOUND('',#1518,.T.);
#958=FACE_OUTER_BOUND('',#1519,.T.);
#959=FACE_OUTER_BOUND('',#1520,.T.);
#960=FACE_OUTER_BOUND('',#1521,.T.);
#961=FACE_OUTER_BOUND('',#1522,.T.);
#962=FACE_OUTER_BOUND('',#1523,.T.);
#963=FACE_OUTER_BOUND('',#1524,.T.);
#964=FACE_OUTER_BOUND('',#1525,.T.);
#965=FACE_OUTER_BOUND('',#1526,.T.);
#966=FACE_OUTER_BOUND('',#1527,.T.);
#967=FACE_OUTER_BOUND('',#1528,.T.);
#968=FACE_OUTER_BOUND('',#1529,.T.);
#969=FACE_OUTER_BOUND('',#1530,.T.);
#970=FACE_OUTER_BOUND('',#1531,.T.);
#971=FACE_OUTER_BOUND('',#1532,.T.);
#972=FACE_OUTER_BOUND('',#1533,.T.);
#973=FACE_OUTER_BOUND('',#1534,.T.);
#974=FACE_OUTER_BOUND('',#1535,.T.);
#975=FACE_OUTER_BOUND('',#1536,.T.);
#976=FACE_OUTER_BOUND('',#1537,.T.);
#977=FACE_OUTER_BOUND('',#1538,.T.);
#978=FACE_OUTER_BOUND('',#1539,.T.);
#979=FACE_OUTER_BOUND('',#1540,.T.);
#980=FACE_OUTER_BOUND('',#1541,.T.);
#981=FACE_OUTER_BOUND('',#1542,.T.);
#982=FACE_OUTER_BOUND('',#1543,.T.);
#983=FACE_OUTER_BOUND('',#1544,.T.);
#984=FACE_OUTER_BOUND('',#1546,.T.);
#985=FACE_OUTER_BOUND('',#1547,.T.);
#986=FACE_OUTER_BOUND('',#1549,.T.);
#987=FACE_OUTER_BOUND('',#1550,.T.);
#988=FACE_OUTER_BOUND('',#1552,.T.);
#989=FACE_OUTER_BOUND('',#1553,.T.);
#990=FACE_OUTER_BOUND('',#1554,.T.);
#991=FACE_OUTER_BOUND('',#1555,.T.);
#992=FACE_OUTER_BOUND('',#1556,.T.);
#993=FACE_OUTER_BOUND('',#1557,.T.);
#994=FACE_OUTER_BOUND('',#1558,.T.);
#995=FACE_OUTER_BOUND('',#1559,.T.);
#996=FACE_OUTER_BOUND('',#1560,.T.);
#997=FACE_OUTER_BOUND('',#1561,.T.);
#998=FACE_OUTER_BOUND('',#1562,.T.);
#999=FACE_OUTER_BOUND('',#1563,.T.);
#1000=FACE_OUTER_BOUND('',#1564,.T.);
#1001=FACE_OUTER_BOUND('',#1565,.T.);
#1002=FACE_OUTER_BOUND('',#1566,.T.);
#1003=FACE_OUTER_BOUND('',#1567,.T.);
#1004=FACE_OUTER_BOUND('',#1568,.T.);
#1005=FACE_OUTER_BOUND('',#1569,.T.);
#1006=FACE_OUTER_BOUND('',#1570,.T.);
#1007=FACE_OUTER_BOUND('',#1571,.T.);
#1008=FACE_OUTER_BOUND('',#1572,.T.);
#1009=FACE_OUTER_BOUND('',#1573,.T.);
#1010=FACE_OUTER_BOUND('',#1574,.T.);
#1011=FACE_OUTER_BOUND('',#1575,.T.);
#1012=FACE_OUTER_BOUND('',#1576,.T.);
#1013=FACE_OUTER_BOUND('',#1577,.T.);
#1014=FACE_OUTER_BOUND('',#1579,.T.);
#1015=FACE_OUTER_BOUND('',#1580,.T.);
#1016=FACE_OUTER_BOUND('',#1582,.T.);
#1017=FACE_OUTER_BOUND('',#1583,.T.);
#1018=FACE_OUTER_BOUND('',#1585,.T.);
#1019=FACE_OUTER_BOUND('',#1586,.T.);
#1020=FACE_OUTER_BOUND('',#1588,.T.);
#1021=FACE_OUTER_BOUND('',#1589,.T.);
#1022=FACE_OUTER_BOUND('',#1590,.T.);
#1023=FACE_OUTER_BOUND('',#1592,.T.);
#1024=FACE_OUTER_BOUND('',#1593,.T.);
#1025=FACE_OUTER_BOUND('',#1594,.T.);
#1026=FACE_OUTER_BOUND('',#1595,.T.);
#1027=FACE_OUTER_BOUND('',#1596,.T.);
#1028=FACE_OUTER_BOUND('',#1597,.T.);
#1029=FACE_OUTER_BOUND('',#1598,.T.);
#1030=FACE_OUTER_BOUND('',#1599,.T.);
#1031=FACE_OUTER_BOUND('',#1600,.T.);
#1032=FACE_OUTER_BOUND('',#1601,.T.);
#1033=FACE_OUTER_BOUND('',#1602,.T.);
#1034=FACE_OUTER_BOUND('',#1603,.T.);
#1035=FACE_OUTER_BOUND('',#1604,.T.);
#1036=FACE_OUTER_BOUND('',#1605,.T.);
#1037=FACE_OUTER_BOUND('',#1606,.T.);
#1038=FACE_OUTER_BOUND('',#1607,.T.);
#1039=FACE_OUTER_BOUND('',#1608,.T.);
#1040=FACE_OUTER_BOUND('',#1609,.T.);
#1041=FACE_OUTER_BOUND('',#1610,.T.);
#1042=FACE_OUTER_BOUND('',#1611,.T.);
#1043=FACE_OUTER_BOUND('',#1612,.T.);
#1044=FACE_OUTER_BOUND('',#1613,.T.);
#1045=FACE_OUTER_BOUND('',#1614,.T.);
#1046=FACE_OUTER_BOUND('',#1615,.T.);
#1047=FACE_OUTER_BOUND('',#1617,.T.);
#1048=FACE_OUTER_BOUND('',#1618,.T.);
#1049=FACE_OUTER_BOUND('',#1620,.T.);
#1050=FACE_OUTER_BOUND('',#1621,.T.);
#1051=FACE_OUTER_BOUND('',#1623,.T.);
#1052=FACE_OUTER_BOUND('',#1624,.T.);
#1053=FACE_OUTER_BOUND('',#1625,.T.);
#1054=FACE_OUTER_BOUND('',#1626,.T.);
#1055=EDGE_LOOP('',(#5620,#5621,#5622,#5623,#5624,#5625));
#1056=EDGE_LOOP('',(#5626,#5627,#5628,#5629));
#1057=EDGE_LOOP('',(#5630,#5631,#5632,#5633,#5634));
#1058=EDGE_LOOP('',(#5635,#5636,#5637,#5638,#5639));
#1059=EDGE_LOOP('',(#5640,#5641,#5642,#5643));
#1060=EDGE_LOOP('',(#5644,#5645,#5646,#5647,#5648));
#1061=EDGE_LOOP('',(#5649,#5650,#5651,#5652,#5653,#5654));
#1062=EDGE_LOOP('',(#5655,#5656,#5657,#5658,#5659,#5660));
#1063=EDGE_LOOP('',(#5661,#5662,#5663,#5664,#5665,#5666));
#1064=EDGE_LOOP('',(#5667,#5668,#5669,#5670,#5671));
#1065=EDGE_LOOP('',(#5672,#5673,#5674,#5675,#5676,#5677));
#1066=EDGE_LOOP('',(#5678,#5679,#5680,#5681,#5682,#5683));
#1067=EDGE_LOOP('',(#5684,#5685,#5686,#5687));
#1068=EDGE_LOOP('',(#5688,#5689,#5690,#5691));
#1069=EDGE_LOOP('',(#5692,#5693,#5694,#5695));
#1070=EDGE_LOOP('',(#5696,#5697,#5698,#5699));
#1071=EDGE_LOOP('',(#5700));
#1072=EDGE_LOOP('',(#5701,#5702,#5703,#5704));
#1073=EDGE_LOOP('',(#5705,#5706,#5707));
#1074=EDGE_LOOP('',(#5708,#5709,#5710,#5711,#5712));
#1075=EDGE_LOOP('',(#5713,#5714,#5715,#5716,#5717,#5718,#5719));
#1076=EDGE_LOOP('',(#5720,#5721,#5722,#5723,#5724));
#1077=EDGE_LOOP('',(#5725,#5726,#5727,#5728));
#1078=EDGE_LOOP('',(#5729,#5730,#5731,#5732));
#1079=EDGE_LOOP('',(#5733,#5734,#5735,#5736,#5737));
#1080=EDGE_LOOP('',(#5738,#5739,#5740,#5741,#5742));
#1081=EDGE_LOOP('',(#5743,#5744,#5745,#5746,#5747));
#1082=EDGE_LOOP('',(#5748,#5749,#5750,#5751,#5752));
#1083=EDGE_LOOP('',(#5753,#5754,#5755,#5756,#5757,#5758));
#1084=EDGE_LOOP('',(#5759,#5760,#5761,#5762,#5763));
#1085=EDGE_LOOP('',(#5764,#5765,#5766,#5767,#5768,#5769));
#1086=EDGE_LOOP('',(#5770,#5771,#5772));
#1087=EDGE_LOOP('',(#5773,#5774,#5775));
#1088=EDGE_LOOP('',(#5776,#5777,#5778,#5779,#5780));
#1089=EDGE_LOOP('',(#5781,#5782,#5783,#5784));
#1090=EDGE_LOOP('',(#5785));
#1091=EDGE_LOOP('',(#5786));
#1092=EDGE_LOOP('',(#5787,#5788,#5789,#5790,#5791));
#1093=EDGE_LOOP('',(#5792,#5793,#5794,#5795));
#1094=EDGE_LOOP('',(#5796,#5797,#5798,#5799,#5800,#5801,#5802,#5803,#5804,
#5805,#5806,#5807,#5808,#5809,#5810,#5811,#5812,#5813,#5814,#5815,#5816,
#5817,#5818,#5819,#5820,#5821,#5822,#5823,#5824,#5825,#5826,#5827,#5828,
#5829,#5830,#5831,#5832,#5833,#5834,#5835,#5836,#5837,#5838,#5839,#5840,
#5841,#5842,#5843,#5844,#5845,#5846,#5847,#5848,#5849,#5850,#5851,#5852,
#5853,#5854,#5855,#5856,#5857,#5858,#5859,#5860,#5861,#5862,#5863,#5864,
#5865,#5866,#5867,#5868,#5869,#5870,#5871,#5872,#5873,#5874,#5875,#5876,
#5877,#5878,#5879,#5880,#5881,#5882,#5883,#5884,#5885,#5886,#5887,#5888,
#5889,#5890,#5891));
#1095=EDGE_LOOP('',(#5892,#5893,#5894,#5895,#5896,#5897));
#1096=EDGE_LOOP('',(#5898,#5899,#5900,#5901));
#1097=EDGE_LOOP('',(#5902,#5903,#5904,#5905));
#1098=EDGE_LOOP('',(#5906,#5907,#5908,#5909));
#1099=EDGE_LOOP('',(#5910,#5911,#5912,#5913));
#1100=EDGE_LOOP('',(#5914,#5915,#5916,#5917));
#1101=EDGE_LOOP('',(#5918,#5919,#5920,#5921));
#1102=EDGE_LOOP('',(#5922));
#1103=EDGE_LOOP('',(#5923,#5924,#5925,#5926,#5927,#5928));
#1104=EDGE_LOOP('',(#5929,#5930,#5931,#5932));
#1105=EDGE_LOOP('',(#5933,#5934,#5935,#5936,#5937,#5938,#5939,#5940,#5941,
#5942,#5943,#5944,#5945,#5946,#5947,#5948,#5949,#5950,#5951,#5952,#5953,
#5954,#5955,#5956,#5957,#5958,#5959,#5960,#5961,#5962,#5963,#5964,#5965,
#5966,#5967,#5968,#5969,#5970,#5971,#5972,#5973,#5974,#5975,#5976,#5977,
#5978,#5979,#5980,#5981,#5982,#5983,#5984,#5985,#5986,#5987,#5988,#5989,
#5990,#5991,#5992,#5993,#5994,#5995,#5996,#5997,#5998,#5999,#6000,#6001,
#6002,#6003,#6004,#6005,#6006,#6007,#6008,#6009,#6010,#6011,#6012,#6013,
#6014,#6015,#6016,#6017,#6018,#6019,#6020,#6021,#6022,#6023,#6024,#6025,
#6026,#6027,#6028));
#1106=EDGE_LOOP('',(#6029));
#1107=EDGE_LOOP('',(#6030,#6031,#6032,#6033));
#1108=EDGE_LOOP('',(#6034,#6035,#6036,#6037));
#1109=EDGE_LOOP('',(#6038,#6039,#6040,#6041));
#1110=EDGE_LOOP('',(#6042,#6043,#6044,#6045));
#1111=EDGE_LOOP('',(#6046,#6047,#6048,#6049));
#1112=EDGE_LOOP('',(#6050,#6051,#6052,#6053));
#1113=EDGE_LOOP('',(#6054,#6055,#6056,#6057));
#1114=EDGE_LOOP('',(#6058,#6059,#6060,#6061));
#1115=EDGE_LOOP('',(#6062,#6063,#6064,#6065));
#1116=EDGE_LOOP('',(#6066,#6067,#6068,#6069));
#1117=EDGE_LOOP('',(#6070,#6071,#6072,#6073));
#1118=EDGE_LOOP('',(#6074,#6075,#6076,#6077));
#1119=EDGE_LOOP('',(#6078,#6079,#6080,#6081));
#1120=EDGE_LOOP('',(#6082,#6083,#6084,#6085));
#1121=EDGE_LOOP('',(#6086,#6087,#6088,#6089));
#1122=EDGE_LOOP('',(#6090,#6091,#6092,#6093));
#1123=EDGE_LOOP('',(#6094,#6095,#6096,#6097));
#1124=EDGE_LOOP('',(#6098,#6099,#6100,#6101,#6102,#6103));
#1125=EDGE_LOOP('',(#6104,#6105,#6106,#6107));
#1126=EDGE_LOOP('',(#6108,#6109,#6110,#6111));
#1127=EDGE_LOOP('',(#6112,#6113,#6114,#6115));
#1128=EDGE_LOOP('',(#6116,#6117,#6118,#6119,#6120,#6121));
#1129=EDGE_LOOP('',(#6122,#6123,#6124,#6125));
#1130=EDGE_LOOP('',(#6126,#6127,#6128,#6129));
#1131=EDGE_LOOP('',(#6130,#6131,#6132,#6133,#6134,#6135));
#1132=EDGE_LOOP('',(#6136,#6137,#6138,#6139));
#1133=EDGE_LOOP('',(#6140,#6141,#6142,#6143,#6144,#6145));
#1134=EDGE_LOOP('',(#6146,#6147,#6148,#6149));
#1135=EDGE_LOOP('',(#6150,#6151,#6152,#6153));
#1136=EDGE_LOOP('',(#6154,#6155,#6156,#6157));
#1137=EDGE_LOOP('',(#6158,#6159,#6160,#6161));
#1138=EDGE_LOOP('',(#6162,#6163,#6164,#6165,#6166,#6167));
#1139=EDGE_LOOP('',(#6168,#6169,#6170,#6171));
#1140=EDGE_LOOP('',(#6172,#6173,#6174,#6175));
#1141=EDGE_LOOP('',(#6176,#6177,#6178,#6179));
#1142=EDGE_LOOP('',(#6180,#6181,#6182,#6183,#6184,#6185));
#1143=EDGE_LOOP('',(#6186,#6187,#6188,#6189));
#1144=EDGE_LOOP('',(#6190,#6191,#6192,#6193));
#1145=EDGE_LOOP('',(#6194,#6195,#6196,#6197,#6198,#6199));
#1146=EDGE_LOOP('',(#6200,#6201,#6202,#6203));
#1147=EDGE_LOOP('',(#6204,#6205,#6206,#6207));
#1148=EDGE_LOOP('',(#6208,#6209,#6210,#6211));
#1149=EDGE_LOOP('',(#6212,#6213,#6214,#6215,#6216,#6217));
#1150=EDGE_LOOP('',(#6218,#6219,#6220,#6221));
#1151=EDGE_LOOP('',(#6222,#6223,#6224,#6225));
#1152=EDGE_LOOP('',(#6226,#6227,#6228,#6229,#6230,#6231));
#1153=EDGE_LOOP('',(#6232,#6233,#6234,#6235));
#1154=EDGE_LOOP('',(#6236,#6237,#6238,#6239));
#1155=EDGE_LOOP('',(#6240,#6241,#6242,#6243));
#1156=EDGE_LOOP('',(#6244,#6245,#6246,#6247,#6248,#6249));
#1157=EDGE_LOOP('',(#6250,#6251,#6252,#6253));
#1158=EDGE_LOOP('',(#6254,#6255,#6256,#6257));
#1159=EDGE_LOOP('',(#6258,#6259,#6260,#6261,#6262,#6263));
#1160=EDGE_LOOP('',(#6264,#6265,#6266,#6267));
#1161=EDGE_LOOP('',(#6268,#6269,#6270,#6271));
#1162=EDGE_LOOP('',(#6272,#6273,#6274,#6275));
#1163=EDGE_LOOP('',(#6276,#6277,#6278,#6279,#6280,#6281));
#1164=EDGE_LOOP('',(#6282,#6283,#6284,#6285));
#1165=EDGE_LOOP('',(#6286,#6287,#6288,#6289));
#1166=EDGE_LOOP('',(#6290,#6291,#6292,#6293,#6294,#6295));
#1167=EDGE_LOOP('',(#6296,#6297,#6298,#6299));
#1168=EDGE_LOOP('',(#6300,#6301,#6302,#6303));
#1169=EDGE_LOOP('',(#6304,#6305,#6306,#6307));
#1170=EDGE_LOOP('',(#6308,#6309,#6310,#6311,#6312,#6313));
#1171=EDGE_LOOP('',(#6314,#6315,#6316,#6317));
#1172=EDGE_LOOP('',(#6318,#6319,#6320,#6321));
#1173=EDGE_LOOP('',(#6322,#6323,#6324,#6325,#6326,#6327));
#1174=EDGE_LOOP('',(#6328,#6329,#6330,#6331));
#1175=EDGE_LOOP('',(#6332,#6333,#6334,#6335));
#1176=EDGE_LOOP('',(#6336,#6337,#6338,#6339));
#1177=EDGE_LOOP('',(#6340,#6341,#6342,#6343,#6344,#6345));
#1178=EDGE_LOOP('',(#6346,#6347,#6348,#6349));
#1179=EDGE_LOOP('',(#6350,#6351,#6352,#6353));
#1180=EDGE_LOOP('',(#6354,#6355,#6356,#6357,#6358,#6359));
#1181=EDGE_LOOP('',(#6360,#6361,#6362,#6363));
#1182=EDGE_LOOP('',(#6364,#6365,#6366,#6367));
#1183=EDGE_LOOP('',(#6368,#6369,#6370,#6371));
#1184=EDGE_LOOP('',(#6372,#6373,#6374,#6375,#6376,#6377));
#1185=EDGE_LOOP('',(#6378,#6379,#6380,#6381));
#1186=EDGE_LOOP('',(#6382,#6383,#6384,#6385));
#1187=EDGE_LOOP('',(#6386,#6387,#6388,#6389,#6390,#6391));
#1188=EDGE_LOOP('',(#6392,#6393,#6394,#6395));
#1189=EDGE_LOOP('',(#6396,#6397,#6398,#6399));
#1190=EDGE_LOOP('',(#6400,#6401,#6402,#6403));
#1191=EDGE_LOOP('',(#6404,#6405,#6406,#6407,#6408,#6409));
#1192=EDGE_LOOP('',(#6410,#6411,#6412,#6413));
#1193=EDGE_LOOP('',(#6414,#6415,#6416,#6417));
#1194=EDGE_LOOP('',(#6418,#6419,#6420,#6421,#6422,#6423));
#1195=EDGE_LOOP('',(#6424,#6425,#6426,#6427));
#1196=EDGE_LOOP('',(#6428,#6429,#6430,#6431));
#1197=EDGE_LOOP('',(#6432,#6433,#6434,#6435));
#1198=EDGE_LOOP('',(#6436,#6437,#6438,#6439,#6440,#6441));
#1199=EDGE_LOOP('',(#6442,#6443,#6444,#6445));
#1200=EDGE_LOOP('',(#6446,#6447,#6448,#6449));
#1201=EDGE_LOOP('',(#6450,#6451,#6452,#6453,#6454,#6455));
#1202=EDGE_LOOP('',(#6456,#6457,#6458,#6459));
#1203=EDGE_LOOP('',(#6460,#6461,#6462,#6463));
#1204=EDGE_LOOP('',(#6464,#6465,#6466,#6467));
#1205=EDGE_LOOP('',(#6468,#6469,#6470,#6471,#6472,#6473));
#1206=EDGE_LOOP('',(#6474,#6475,#6476,#6477));
#1207=EDGE_LOOP('',(#6478,#6479,#6480,#6481));
#1208=EDGE_LOOP('',(#6482,#6483,#6484,#6485,#6486,#6487));
#1209=EDGE_LOOP('',(#6488,#6489,#6490,#6491));
#1210=EDGE_LOOP('',(#6492,#6493,#6494,#6495));
#1211=EDGE_LOOP('',(#6496,#6497,#6498,#6499));
#1212=EDGE_LOOP('',(#6500,#6501,#6502,#6503,#6504,#6505));
#1213=EDGE_LOOP('',(#6506,#6507,#6508,#6509));
#1214=EDGE_LOOP('',(#6510,#6511,#6512,#6513));
#1215=EDGE_LOOP('',(#6514,#6515,#6516,#6517,#6518,#6519));
#1216=EDGE_LOOP('',(#6520,#6521,#6522,#6523));
#1217=EDGE_LOOP('',(#6524,#6525,#6526,#6527));
#1218=EDGE_LOOP('',(#6528,#6529,#6530,#6531));
#1219=EDGE_LOOP('',(#6532,#6533,#6534,#6535,#6536,#6537));
#1220=EDGE_LOOP('',(#6538,#6539,#6540,#6541));
#1221=EDGE_LOOP('',(#6542,#6543,#6544,#6545));
#1222=EDGE_LOOP('',(#6546,#6547,#6548,#6549,#6550,#6551));
#1223=EDGE_LOOP('',(#6552,#6553,#6554,#6555));
#1224=EDGE_LOOP('',(#6556,#6557,#6558,#6559));
#1225=EDGE_LOOP('',(#6560,#6561,#6562,#6563));
#1226=EDGE_LOOP('',(#6564,#6565,#6566,#6567,#6568,#6569));
#1227=EDGE_LOOP('',(#6570,#6571,#6572,#6573));
#1228=EDGE_LOOP('',(#6574,#6575,#6576,#6577));
#1229=EDGE_LOOP('',(#6578,#6579,#6580,#6581,#6582,#6583));
#1230=EDGE_LOOP('',(#6584,#6585,#6586,#6587));
#1231=EDGE_LOOP('',(#6588,#6589,#6590,#6591,#6592,#6593));
#1232=EDGE_LOOP('',(#6594,#6595,#6596,#6597));
#1233=EDGE_LOOP('',(#6598,#6599,#6600,#6601));
#1234=EDGE_LOOP('',(#6602,#6603,#6604,#6605));
#1235=EDGE_LOOP('',(#6606));
#1236=EDGE_LOOP('',(#6607,#6608,#6609,#6610,#6611,#6612));
#1237=EDGE_LOOP('',(#6613,#6614,#6615,#6616));
#1238=EDGE_LOOP('',(#6617,#6618,#6619,#6620));
#1239=EDGE_LOOP('',(#6621,#6622,#6623,#6624));
#1240=EDGE_LOOP('',(#6625));
#1241=EDGE_LOOP('',(#6626,#6627));
#1242=EDGE_LOOP('',(#6628,#6629,#6630));
#1243=EDGE_LOOP('',(#6631,#6632,#6633,#6634,#6635));
#1244=EDGE_LOOP('',(#6636,#6637,#6638,#6639));
#1245=EDGE_LOOP('',(#6640,#6641,#6642,#6643));
#1246=EDGE_LOOP('',(#6644,#6645,#6646,#6647));
#1247=EDGE_LOOP('',(#6648,#6649,#6650,#6651));
#1248=EDGE_LOOP('',(#6652,#6653,#6654,#6655));
#1249=EDGE_LOOP('',(#6656,#6657,#6658,#6659));
#1250=EDGE_LOOP('',(#6660,#6661,#6662,#6663,#6664,#6665));
#1251=EDGE_LOOP('',(#6666,#6667,#6668,#6669,#6670,#6671));
#1252=EDGE_LOOP('',(#6672,#6673,#6674));
#1253=EDGE_LOOP('',(#6675,#6676,#6677,#6678,#6679,#6680));
#1254=EDGE_LOOP('',(#6681,#6682,#6683,#6684,#6685,#6686));
#1255=EDGE_LOOP('',(#6687,#6688,#6689,#6690));
#1256=EDGE_LOOP('',(#6691,#6692,#6693,#6694));
#1257=EDGE_LOOP('',(#6695,#6696,#6697,#6698));
#1258=EDGE_LOOP('',(#6699,#6700,#6701,#6702));
#1259=EDGE_LOOP('',(#6703,#6704,#6705,#6706));
#1260=EDGE_LOOP('',(#6707,#6708,#6709,#6710,#6711));
#1261=EDGE_LOOP('',(#6712,#6713,#6714,#6715));
#1262=EDGE_LOOP('',(#6716,#6717,#6718,#6719,#6720,#6721,#6722));
#1263=EDGE_LOOP('',(#6723,#6724,#6725));
#1264=EDGE_LOOP('',(#6726,#6727,#6728,#6729,#6730));
#1265=EDGE_LOOP('',(#6731,#6732,#6733,#6734,#6735));
#1266=EDGE_LOOP('',(#6736,#6737,#6738,#6739,#6740));
#1267=EDGE_LOOP('',(#6741,#6742,#6743,#6744,#6745));
#1268=EDGE_LOOP('',(#6746,#6747,#6748,#6749,#6750));
#1269=EDGE_LOOP('',(#6751,#6752,#6753,#6754,#6755));
#1270=EDGE_LOOP('',(#6756,#6757,#6758,#6759,#6760));
#1271=EDGE_LOOP('',(#6761,#6762,#6763));
#1272=EDGE_LOOP('',(#6764));
#1273=EDGE_LOOP('',(#6765));
#1274=EDGE_LOOP('',(#6766,#6767,#6768,#6769));
#1275=EDGE_LOOP('',(#6770));
#1276=EDGE_LOOP('',(#6771));
#1277=EDGE_LOOP('',(#6772,#6773,#6774,#6775));
#1278=EDGE_LOOP('',(#6776,#6777,#6778));
#1279=EDGE_LOOP('',(#6779,#6780));
#1280=EDGE_LOOP('',(#6781,#6782,#6783,#6784,#6785));
#1281=EDGE_LOOP('',(#6786,#6787,#6788,#6789,#6790,#6791));
#1282=EDGE_LOOP('',(#6792,#6793,#6794,#6795,#6796,#6797));
#1283=EDGE_LOOP('',(#6798,#6799,#6800));
#1284=EDGE_LOOP('',(#6801,#6802,#6803,#6804,#6805,#6806));
#1285=EDGE_LOOP('',(#6807,#6808,#6809,#6810,#6811));
#1286=EDGE_LOOP('',(#6812,#6813,#6814,#6815));
#1287=EDGE_LOOP('',(#6816,#6817,#6818,#6819,#6820));
#1288=EDGE_LOOP('',(#6821,#6822,#6823,#6824,#6825));
#1289=EDGE_LOOP('',(#6826,#6827,#6828,#6829));
#1290=EDGE_LOOP('',(#6830,#6831,#6832,#6833,#6834));
#1291=EDGE_LOOP('',(#6835,#6836,#6837,#6838,#6839,#6840,#6841));
#1292=EDGE_LOOP('',(#6842,#6843,#6844,#6845,#6846,#6847,#6848,#6849,#6850));
#1293=EDGE_LOOP('',(#6851,#6852,#6853,#6854,#6855,#6856,#6857,#6858));
#1294=EDGE_LOOP('',(#6859,#6860,#6861,#6862,#6863));
#1295=EDGE_LOOP('',(#6864,#6865,#6866,#6867,#6868));
#1296=EDGE_LOOP('',(#6869,#6870,#6871,#6872));
#1297=EDGE_LOOP('',(#6873));
#1298=EDGE_LOOP('',(#6874));
#1299=EDGE_LOOP('',(#6875,#6876,#6877,#6878,#6879));
#1300=EDGE_LOOP('',(#6880,#6881,#6882,#6883,#6884,#6885,#6886,#6887,#6888,
#6889,#6890,#6891,#6892,#6893,#6894,#6895,#6896,#6897,#6898,#6899,#6900,
#6901,#6902,#6903,#6904,#6905,#6906,#6907,#6908));
#1301=EDGE_LOOP('',(#6909,#6910,#6911,#6912,#6913));
#1302=EDGE_LOOP('',(#6914,#6915,#6916,#6917));
#1303=EDGE_LOOP('',(#6918,#6919,#6920,#6921,#6922,#6923,#6924,#6925,#6926,
#6927,#6928,#6929,#6930,#6931,#6932,#6933,#6934,#6935,#6936,#6937,#6938,
#6939,#6940,#6941));
#1304=EDGE_LOOP('',(#6942,#6943,#6944,#6945,#6946));
#1305=EDGE_LOOP('',(#6947,#6948,#6949,#6950));
#1306=EDGE_LOOP('',(#6951,#6952,#6953,#6954));
#1307=EDGE_LOOP('',(#6955,#6956,#6957,#6958));
#1308=EDGE_LOOP('',(#6959,#6960,#6961,#6962));
#1309=EDGE_LOOP('',(#6963,#6964,#6965,#6966,#6967));
#1310=EDGE_LOOP('',(#6968,#6969,#6970,#6971));
#1311=EDGE_LOOP('',(#6972,#6973,#6974,#6975));
#1312=EDGE_LOOP('',(#6976,#6977,#6978,#6979));
#1313=EDGE_LOOP('',(#6980,#6981,#6982,#6983));
#1314=EDGE_LOOP('',(#6984,#6985,#6986,#6987));
#1315=EDGE_LOOP('',(#6988,#6989,#6990,#6991,#6992));
#1316=EDGE_LOOP('',(#6993,#6994,#6995,#6996));
#1317=EDGE_LOOP('',(#6997,#6998,#6999,#7000));
#1318=EDGE_LOOP('',(#7001,#7002,#7003,#7004,#7005));
#1319=EDGE_LOOP('',(#7006,#7007,#7008,#7009));
#1320=EDGE_LOOP('',(#7010,#7011,#7012,#7013,#7014));
#1321=EDGE_LOOP('',(#7015,#7016,#7017,#7018));
#1322=EDGE_LOOP('',(#7019,#7020,#7021,#7022));
#1323=EDGE_LOOP('',(#7023,#7024,#7025,#7026));
#1324=EDGE_LOOP('',(#7027,#7028,#7029,#7030,#7031));
#1325=EDGE_LOOP('',(#7032,#7033,#7034,#7035));
#1326=EDGE_LOOP('',(#7036,#7037,#7038,#7039,#7040));
#1327=EDGE_LOOP('',(#7041,#7042,#7043,#7044));
#1328=EDGE_LOOP('',(#7045,#7046,#7047,#7048,#7049));
#1329=EDGE_LOOP('',(#7050,#7051,#7052,#7053));
#1330=EDGE_LOOP('',(#7054,#7055,#7056,#7057,#7058,#7059,#7060,#7061,#7062,
#7063,#7064));
#1331=EDGE_LOOP('',(#7065,#7066,#7067,#7068));
#1332=EDGE_LOOP('',(#7069,#7070,#7071));
#1333=EDGE_LOOP('',(#7072,#7073,#7074));
#1334=EDGE_LOOP('',(#7075,#7076,#7077));
#1335=EDGE_LOOP('',(#7078,#7079,#7080));
#1336=EDGE_LOOP('',(#7081,#7082,#7083,#7084));
#1337=EDGE_LOOP('',(#7085,#7086,#7087,#7088));
#1338=EDGE_LOOP('',(#7089,#7090,#7091,#7092,#7093));
#1339=EDGE_LOOP('',(#7094,#7095,#7096,#7097));
#1340=EDGE_LOOP('',(#7098,#7099,#7100,#7101,#7102));
#1341=EDGE_LOOP('',(#7103,#7104,#7105,#7106));
#1342=EDGE_LOOP('',(#7107,#7108,#7109,#7110));
#1343=EDGE_LOOP('',(#7111,#7112,#7113,#7114,#7115,#7116,#7117,#7118,#7119,
#7120,#7121));
#1344=EDGE_LOOP('',(#7122,#7123,#7124));
#1345=EDGE_LOOP('',(#7125,#7126,#7127,#7128));
#1346=EDGE_LOOP('',(#7129,#7130,#7131,#7132,#7133,#7134));
#1347=EDGE_LOOP('',(#7135,#7136,#7137,#7138,#7139,#7140));
#1348=EDGE_LOOP('',(#7141,#7142,#7143,#7144,#7145));
#1349=EDGE_LOOP('',(#7146,#7147,#7148,#7149,#7150,#7151));
#1350=EDGE_LOOP('',(#7152,#7153,#7154));
#1351=EDGE_LOOP('',(#7155,#7156,#7157,#7158));
#1352=EDGE_LOOP('',(#7159,#7160,#7161,#7162));
#1353=EDGE_LOOP('',(#7163,#7164,#7165,#7166));
#1354=EDGE_LOOP('',(#7167,#7168,#7169));
#1355=EDGE_LOOP('',(#7170,#7171,#7172,#7173));
#1356=EDGE_LOOP('',(#7174,#7175,#7176,#7177,#7178));
#1357=EDGE_LOOP('',(#7179,#7180,#7181,#7182));
#1358=EDGE_LOOP('',(#7183,#7184,#7185,#7186));
#1359=EDGE_LOOP('',(#7187,#7188,#7189,#7190));
#1360=EDGE_LOOP('',(#7191,#7192,#7193,#7194));
#1361=EDGE_LOOP('',(#7195,#7196,#7197,#7198));
#1362=EDGE_LOOP('',(#7199,#7200,#7201,#7202));
#1363=EDGE_LOOP('',(#7203,#7204,#7205,#7206));
#1364=EDGE_LOOP('',(#7207,#7208,#7209,#7210,#7211));
#1365=EDGE_LOOP('',(#7212,#7213,#7214,#7215));
#1366=EDGE_LOOP('',(#7216,#7217,#7218,#7219,#7220));
#1367=EDGE_LOOP('',(#7221,#7222,#7223,#7224));
#1368=EDGE_LOOP('',(#7225,#7226,#7227));
#1369=EDGE_LOOP('',(#7228,#7229,#7230,#7231));
#1370=EDGE_LOOP('',(#7232,#7233,#7234,#7235));
#1371=EDGE_LOOP('',(#7236,#7237,#7238,#7239));
#1372=EDGE_LOOP('',(#7240,#7241,#7242,#7243));
#1373=EDGE_LOOP('',(#7244,#7245,#7246));
#1374=EDGE_LOOP('',(#7247,#7248,#7249,#7250));
#1375=EDGE_LOOP('',(#7251,#7252,#7253,#7254,#7255));
#1376=EDGE_LOOP('',(#7256,#7257,#7258,#7259,#7260,#7261,#7262,#7263,#7264,
#7265,#7266,#7267));
#1377=EDGE_LOOP('',(#7268,#7269,#7270,#7271,#7272));
#1378=EDGE_LOOP('',(#7273,#7274,#7275,#7276));
#1379=EDGE_LOOP('',(#7277,#7278,#7279,#7280));
#1380=EDGE_LOOP('',(#7281,#7282,#7283,#7284));
#1381=EDGE_LOOP('',(#7285,#7286,#7287,#7288,#7289));
#1382=EDGE_LOOP('',(#7290,#7291,#7292,#7293));
#1383=EDGE_LOOP('',(#7294,#7295,#7296,#7297,#7298,#7299,#7300,#7301,#7302,
#7303,#7304,#7305,#7306,#7307,#7308,#7309));
#1384=EDGE_LOOP('',(#7310,#7311,#7312,#7313));
#1385=EDGE_LOOP('',(#7314,#7315,#7316,#7317));
#1386=EDGE_LOOP('',(#7318,#7319,#7320,#7321));
#1387=EDGE_LOOP('',(#7322,#7323,#7324,#7325,#7326,#7327,#7328,#7329,#7330,
#7331,#7332,#7333,#7334,#7335,#7336,#7337));
#1388=EDGE_LOOP('',(#7338,#7339,#7340,#7341));
#1389=EDGE_LOOP('',(#7342,#7343,#7344,#7345));
#1390=EDGE_LOOP('',(#7346,#7347,#7348,#7349));
#1391=EDGE_LOOP('',(#7350,#7351,#7352,#7353));
#1392=EDGE_LOOP('',(#7354,#7355,#7356,#7357));
#1393=EDGE_LOOP('',(#7358,#7359,#7360,#7361));
#1394=EDGE_LOOP('',(#7362,#7363,#7364,#7365));
#1395=EDGE_LOOP('',(#7366,#7367,#7368,#7369));
#1396=EDGE_LOOP('',(#7370,#7371,#7372,#7373));
#1397=EDGE_LOOP('',(#7374,#7375,#7376,#7377));
#1398=EDGE_LOOP('',(#7378,#7379,#7380,#7381));
#1399=EDGE_LOOP('',(#7382,#7383,#7384,#7385));
#1400=EDGE_LOOP('',(#7386,#7387,#7388,#7389));
#1401=EDGE_LOOP('',(#7390,#7391,#7392));
#1402=EDGE_LOOP('',(#7393,#7394));
#1403=EDGE_LOOP('',(#7395,#7396,#7397,#7398,#7399,#7400,#7401,#7402,#7403));
#1404=EDGE_LOOP('',(#7404,#7405,#7406,#7407,#7408));
#1405=EDGE_LOOP('',(#7409));
#1406=EDGE_LOOP('',(#7410));
#1407=EDGE_LOOP('',(#7411,#7412,#7413,#7414));
#1408=EDGE_LOOP('',(#7415));
#1409=EDGE_LOOP('',(#7416));
#1410=EDGE_LOOP('',(#7417,#7418,#7419,#7420));
#1411=EDGE_LOOP('',(#7421,#7422,#7423,#7424));
#1412=EDGE_LOOP('',(#7425,#7426,#7427,#7428));
#1413=EDGE_LOOP('',(#7429,#7430,#7431,#7432));
#1414=EDGE_LOOP('',(#7433,#7434,#7435,#7436));
#1415=EDGE_LOOP('',(#7437,#7438,#7439));
#1416=EDGE_LOOP('',(#7440,#7441,#7442,#7443));
#1417=EDGE_LOOP('',(#7444,#7445,#7446,#7447));
#1418=EDGE_LOOP('',(#7448,#7449,#7450));
#1419=EDGE_LOOP('',(#7451,#7452,#7453));
#1420=EDGE_LOOP('',(#7454,#7455,#7456,#7457));
#1421=EDGE_LOOP('',(#7458,#7459,#7460,#7461));
#1422=EDGE_LOOP('',(#7462,#7463,#7464,#7465));
#1423=EDGE_LOOP('',(#7466,#7467,#7468,#7469));
#1424=EDGE_LOOP('',(#7470));
#1425=EDGE_LOOP('',(#7471,#7472,#7473,#7474,#7475,#7476,#7477,#7478,#7479,
#7480,#7481,#7482,#7483,#7484,#7485,#7486,#7487,#7488,#7489,#7490,#7491,
#7492,#7493,#7494));
#1426=EDGE_LOOP('',(#7495,#7496,#7497,#7498));
#1427=EDGE_LOOP('',(#7499,#7500,#7501,#7502));
#1428=EDGE_LOOP('',(#7503,#7504,#7505,#7506,#7507));
#1429=EDGE_LOOP('',(#7508,#7509,#7510,#7511,#7512,#7513,#7514));
#1430=EDGE_LOOP('',(#7515,#7516,#7517,#7518));
#1431=EDGE_LOOP('',(#7519,#7520,#7521,#7522,#7523,#7524));
#1432=EDGE_LOOP('',(#7525,#7526,#7527,#7528,#7529));
#1433=EDGE_LOOP('',(#7530,#7531,#7532,#7533,#7534));
#1434=EDGE_LOOP('',(#7535,#7536,#7537,#7538,#7539));
#1435=EDGE_LOOP('',(#7540,#7541,#7542,#7543,#7544));
#1436=EDGE_LOOP('',(#7545,#7546,#7547,#7548,#7549));
#1437=EDGE_LOOP('',(#7550,#7551,#7552,#7553,#7554));
#1438=EDGE_LOOP('',(#7555,#7556,#7557,#7558,#7559));
#1439=EDGE_LOOP('',(#7560,#7561,#7562,#7563,#7564));
#1440=EDGE_LOOP('',(#7565,#7566,#7567,#7568,#7569));
#1441=EDGE_LOOP('',(#7570,#7571,#7572,#7573,#7574,#7575));
#1442=EDGE_LOOP('',(#7576,#7577,#7578,#7579,#7580));
#1443=EDGE_LOOP('',(#7581,#7582,#7583));
#1444=EDGE_LOOP('',(#7584,#7585,#7586,#7587));
#1445=EDGE_LOOP('',(#7588,#7589,#7590,#7591));
#1446=EDGE_LOOP('',(#7592,#7593,#7594,#7595));
#1447=EDGE_LOOP('',(#7596,#7597,#7598,#7599));
#1448=EDGE_LOOP('',(#7600,#7601,#7602,#7603));
#1449=EDGE_LOOP('',(#7604,#7605,#7606,#7607));
#1450=EDGE_LOOP('',(#7608,#7609,#7610,#7611));
#1451=EDGE_LOOP('',(#7612,#7613,#7614,#7615));
#1452=EDGE_LOOP('',(#7616,#7617,#7618,#7619));
#1453=EDGE_LOOP('',(#7620,#7621,#7622,#7623,#7624,#7625,#7626,#7627,#7628,
#7629,#7630,#7631,#7632,#7633,#7634,#7635,#7636,#7637,#7638,#7639,#7640,
#7641,#7642,#7643));
#1454=EDGE_LOOP('',(#7644,#7645,#7646,#7647));
#1455=EDGE_LOOP('',(#7648,#7649,#7650,#7651));
#1456=EDGE_LOOP('',(#7652,#7653,#7654,#7655));
#1457=EDGE_LOOP('',(#7656,#7657,#7658,#7659));
#1458=EDGE_LOOP('',(#7660,#7661,#7662,#7663));
#1459=EDGE_LOOP('',(#7664,#7665,#7666,#7667));
#1460=EDGE_LOOP('',(#7668,#7669,#7670,#7671));
#1461=EDGE_LOOP('',(#7672,#7673,#7674,#7675));
#1462=EDGE_LOOP('',(#7676,#7677,#7678,#7679));
#1463=EDGE_LOOP('',(#7680,#7681,#7682,#7683));
#1464=EDGE_LOOP('',(#7684,#7685,#7686,#7687));
#1465=EDGE_LOOP('',(#7688,#7689,#7690,#7691));
#1466=EDGE_LOOP('',(#7692,#7693,#7694,#7695));
#1467=EDGE_LOOP('',(#7696,#7697,#7698,#7699));
#1468=EDGE_LOOP('',(#7700,#7701,#7702,#7703));
#1469=EDGE_LOOP('',(#7704,#7705,#7706,#7707));
#1470=EDGE_LOOP('',(#7708,#7709,#7710,#7711));
#1471=EDGE_LOOP('',(#7712,#7713,#7714,#7715));
#1472=EDGE_LOOP('',(#7716,#7717,#7718,#7719));
#1473=EDGE_LOOP('',(#7720,#7721,#7722,#7723));
#1474=EDGE_LOOP('',(#7724,#7725,#7726,#7727));
#1475=EDGE_LOOP('',(#7728,#7729,#7730,#7731));
#1476=EDGE_LOOP('',(#7732,#7733,#7734,#7735,#7736,#7737));
#1477=EDGE_LOOP('',(#7738));
#1478=EDGE_LOOP('',(#7739,#7740,#7741,#7742,#7743));
#1479=EDGE_LOOP('',(#7744,#7745,#7746,#7747,#7748));
#1480=EDGE_LOOP('',(#7749));
#1481=EDGE_LOOP('',(#7750));
#1482=EDGE_LOOP('',(#7751,#7752,#7753,#7754,#7755));
#1483=EDGE_LOOP('',(#7756,#7757,#7758,#7759,#7760,#7761));
#1484=EDGE_LOOP('',(#7762,#7763,#7764,#7765,#7766));
#1485=EDGE_LOOP('',(#7767,#7768,#7769,#7770,#7771,#7772));
#1486=EDGE_LOOP('',(#7773,#7774,#7775,#7776,#7777,#7778,#7779,#7780));
#1487=EDGE_LOOP('',(#7781,#7782,#7783,#7784));
#1488=EDGE_LOOP('',(#7785,#7786,#7787,#7788));
#1489=EDGE_LOOP('',(#7789,#7790,#7791,#7792,#7793,#7794));
#1490=EDGE_LOOP('',(#7795,#7796,#7797,#7798,#7799));
#1491=EDGE_LOOP('',(#7800,#7801,#7802,#7803,#7804));
#1492=EDGE_LOOP('',(#7805,#7806,#7807,#7808,#7809));
#1493=EDGE_LOOP('',(#7810,#7811,#7812,#7813,#7814));
#1494=EDGE_LOOP('',(#7815,#7816,#7817,#7818,#7819,#7820));
#1495=EDGE_LOOP('',(#7821,#7822,#7823,#7824));
#1496=EDGE_LOOP('',(#7825,#7826,#7827,#7828));
#1497=EDGE_LOOP('',(#7829,#7830,#7831,#7832));
#1498=EDGE_LOOP('',(#7833));
#1499=EDGE_LOOP('',(#7834));
#1500=EDGE_LOOP('',(#7835,#7836,#7837,#7838));
#1501=EDGE_LOOP('',(#7839,#7840));
#1502=EDGE_LOOP('',(#7841));
#1503=EDGE_LOOP('',(#7842));
#1504=EDGE_LOOP('',(#7843,#7844,#7845,#7846));
#1505=EDGE_LOOP('',(#7847,#7848,#7849,#7850,#7851,#7852,#7853,#7854,#7855,
#7856,#7857,#7858,#7859,#7860,#7861));
#1506=EDGE_LOOP('',(#7862));
#1507=EDGE_LOOP('',(#7863));
#1508=EDGE_LOOP('',(#7864,#7865,#7866,#7867));
#1509=EDGE_LOOP('',(#7868,#7869,#7870,#7871));
#1510=EDGE_LOOP('',(#7872));
#1511=EDGE_LOOP('',(#7873,#7874,#7875,#7876));
#1512=EDGE_LOOP('',(#7877,#7878,#7879,#7880));
#1513=EDGE_LOOP('',(#7881,#7882,#7883,#7884));
#1514=EDGE_LOOP('',(#7885,#7886,#7887,#7888));
#1515=EDGE_LOOP('',(#7889,#7890,#7891,#7892));
#1516=EDGE_LOOP('',(#7893,#7894,#7895,#7896));
#1517=EDGE_LOOP('',(#7897,#7898,#7899,#7900));
#1518=EDGE_LOOP('',(#7901,#7902,#7903,#7904));
#1519=EDGE_LOOP('',(#7905,#7906,#7907,#7908));
#1520=EDGE_LOOP('',(#7909,#7910,#7911,#7912));
#1521=EDGE_LOOP('',(#7913,#7914,#7915,#7916));
#1522=EDGE_LOOP('',(#7917,#7918,#7919,#7920));
#1523=EDGE_LOOP('',(#7921,#7922,#7923,#7924));
#1524=EDGE_LOOP('',(#7925,#7926,#7927,#7928));
#1525=EDGE_LOOP('',(#7929,#7930,#7931,#7932));
#1526=EDGE_LOOP('',(#7933,#7934,#7935,#7936));
#1527=EDGE_LOOP('',(#7937,#7938,#7939,#7940));
#1528=EDGE_LOOP('',(#7941,#7942,#7943,#7944,#7945,#7946,#7947,#7948,#7949,
#7950));
#1529=EDGE_LOOP('',(#7951,#7952,#7953,#7954));
#1530=EDGE_LOOP('',(#7955,#7956,#7957,#7958));
#1531=EDGE_LOOP('',(#7959,#7960,#7961,#7962,#7963,#7964));
#1532=EDGE_LOOP('',(#7965,#7966,#7967,#7968,#7969));
#1533=EDGE_LOOP('',(#7970,#7971,#7972,#7973,#7974));
#1534=EDGE_LOOP('',(#7975,#7976,#7977,#7978));
#1535=EDGE_LOOP('',(#7979,#7980,#7981,#7982));
#1536=EDGE_LOOP('',(#7983,#7984,#7985,#7986,#7987,#7988,#7989,#7990));
#1537=EDGE_LOOP('',(#7991,#7992,#7993));
#1538=EDGE_LOOP('',(#7994,#7995,#7996,#7997));
#1539=EDGE_LOOP('',(#7998,#7999,#8000,#8001));
#1540=EDGE_LOOP('',(#8002,#8003,#8004,#8005,#8006,#8007));
#1541=EDGE_LOOP('',(#8008,#8009,#8010,#8011));
#1542=EDGE_LOOP('',(#8012,#8013,#8014,#8015));
#1543=EDGE_LOOP('',(#8016,#8017,#8018,#8019));
#1544=EDGE_LOOP('',(#8020,#8021,#8022,#8023,#8024,#8025));
#1545=EDGE_LOOP('',(#8026));
#1546=EDGE_LOOP('',(#8027,#8028,#8029,#8030));
#1547=EDGE_LOOP('',(#8031));
#1548=EDGE_LOOP('',(#8032));
#1549=EDGE_LOOP('',(#8033,#8034,#8035,#8036,#8037,#8038,#8039,#8040));
#1550=EDGE_LOOP('',(#8041,#8042,#8043,#8044,#8045,#8046,#8047,#8048));
#1551=EDGE_LOOP('',(#8049));
#1552=EDGE_LOOP('',(#8050,#8051,#8052,#8053));
#1553=EDGE_LOOP('',(#8054,#8055,#8056,#8057,#8058,#8059));
#1554=EDGE_LOOP('',(#8060,#8061,#8062,#8063));
#1555=EDGE_LOOP('',(#8064,#8065,#8066,#8067));
#1556=EDGE_LOOP('',(#8068,#8069,#8070,#8071,#8072));
#1557=EDGE_LOOP('',(#8073,#8074,#8075,#8076,#8077));
#1558=EDGE_LOOP('',(#8078,#8079,#8080,#8081,#8082,#8083));
#1559=EDGE_LOOP('',(#8084,#8085,#8086,#8087));
#1560=EDGE_LOOP('',(#8088,#8089,#8090,#8091));
#1561=EDGE_LOOP('',(#8092,#8093,#8094,#8095));
#1562=EDGE_LOOP('',(#8096,#8097,#8098,#8099));
#1563=EDGE_LOOP('',(#8100,#8101,#8102,#8103));
#1564=EDGE_LOOP('',(#8104,#8105,#8106,#8107));
#1565=EDGE_LOOP('',(#8108,#8109,#8110,#8111));
#1566=EDGE_LOOP('',(#8112,#8113,#8114));
#1567=EDGE_LOOP('',(#8115,#8116,#8117,#8118));
#1568=EDGE_LOOP('',(#8119,#8120,#8121,#8122,#8123,#8124,#8125));
#1569=EDGE_LOOP('',(#8126,#8127,#8128,#8129));
#1570=EDGE_LOOP('',(#8130,#8131,#8132,#8133));
#1571=EDGE_LOOP('',(#8134,#8135,#8136,#8137));
#1572=EDGE_LOOP('',(#8138,#8139,#8140,#8141));
#1573=EDGE_LOOP('',(#8142,#8143,#8144,#8145));
#1574=EDGE_LOOP('',(#8146,#8147,#8148,#8149));
#1575=EDGE_LOOP('',(#8150,#8151,#8152,#8153));
#1576=EDGE_LOOP('',(#8154,#8155,#8156,#8157));
#1577=EDGE_LOOP('',(#8158));
#1578=EDGE_LOOP('',(#8159));
#1579=EDGE_LOOP('',(#8160,#8161,#8162,#8163));
#1580=EDGE_LOOP('',(#8164));
#1581=EDGE_LOOP('',(#8165));
#1582=EDGE_LOOP('',(#8166,#8167,#8168,#8169));
#1583=EDGE_LOOP('',(#8170,#8171,#8172,#8173,#8174));
#1584=EDGE_LOOP('',(#8175));
#1585=EDGE_LOOP('',(#8176,#8177,#8178,#8179));
#1586=EDGE_LOOP('',(#8180));
#1587=EDGE_LOOP('',(#8181));
#1588=EDGE_LOOP('',(#8182,#8183,#8184,#8185,#8186,#8187,#8188,#8189,#8190,
#8191,#8192,#8193,#8194,#8195,#8196,#8197));
#1589=EDGE_LOOP('',(#8198,#8199,#8200,#8201));
#1590=EDGE_LOOP('',(#8202,#8203,#8204,#8205,#8206,#8207,#8208,#8209,#8210,
#8211,#8212,#8213));
#1591=EDGE_LOOP('',(#8214));
#1592=EDGE_LOOP('',(#8215,#8216,#8217,#8218,#8219,#8220));
#1593=EDGE_LOOP('',(#8221,#8222,#8223,#8224));
#1594=EDGE_LOOP('',(#8225,#8226,#8227,#8228,#8229));
#1595=EDGE_LOOP('',(#8230,#8231,#8232,#8233,#8234));
#1596=EDGE_LOOP('',(#8235,#8236,#8237,#8238,#8239));
#1597=EDGE_LOOP('',(#8240,#8241,#8242,#8243,#8244,#8245));
#1598=EDGE_LOOP('',(#8246,#8247,#8248,#8249));
#1599=EDGE_LOOP('',(#8250,#8251,#8252,#8253,#8254));
#1600=EDGE_LOOP('',(#8255,#8256,#8257,#8258));
#1601=EDGE_LOOP('',(#8259,#8260,#8261,#8262));
#1602=EDGE_LOOP('',(#8263,#8264,#8265,#8266,#8267,#8268));
#1603=EDGE_LOOP('',(#8269,#8270,#8271,#8272));
#1604=EDGE_LOOP('',(#8273,#8274,#8275,#8276));
#1605=EDGE_LOOP('',(#8277,#8278,#8279,#8280));
#1606=EDGE_LOOP('',(#8281,#8282,#8283,#8284));
#1607=EDGE_LOOP('',(#8285,#8286,#8287,#8288));
#1608=EDGE_LOOP('',(#8289,#8290,#8291,#8292));
#1609=EDGE_LOOP('',(#8293,#8294,#8295,#8296));
#1610=EDGE_LOOP('',(#8297,#8298,#8299,#8300));
#1611=EDGE_LOOP('',(#8301,#8302,#8303,#8304,#8305));
#1612=EDGE_LOOP('',(#8306,#8307,#8308,#8309));
#1613=EDGE_LOOP('',(#8310,#8311,#8312,#8313));
#1614=EDGE_LOOP('',(#8314,#8315,#8316,#8317));
#1615=EDGE_LOOP('',(#8318));
#1616=EDGE_LOOP('',(#8319));
#1617=EDGE_LOOP('',(#8320,#8321,#8322,#8323));
#1618=EDGE_LOOP('',(#8324));
#1619=EDGE_LOOP('',(#8325));
#1620=EDGE_LOOP('',(#8326,#8327,#8328,#8329));
#1621=EDGE_LOOP('',(#8330));
#1622=EDGE_LOOP('',(#8331));
#1623=EDGE_LOOP('',(#8332,#8333,#8334,#8335));
#1624=EDGE_LOOP('',(#8336,#8337,#8338));
#1625=EDGE_LOOP('',(#8339,#8340,#8341,#8342,#8343));
#1626=EDGE_LOOP('',(#8344,#8345,#8346,#8347));
#1627=CIRCLE('',#9278,2.25);
#1628=CIRCLE('',#9285,2.25);
#1629=CIRCLE('',#9288,1.25);
#1630=CIRCLE('',#9292,1.25);
#1631=CIRCLE('',#9296,3.5);
#1632=CIRCLE('',#9298,3.5);
#1633=CIRCLE('',#9299,3.5);
#1634=CIRCLE('',#9301,12.5);
#1635=CIRCLE('',#9304,4.2705);
#1636=CIRCLE('',#9305,6.);
#1637=CIRCLE('',#9306,1.825);
#1638=CIRCLE('',#9307,5.6245);
#1639=CIRCLE('',#9308,1.825);
#1640=CIRCLE('',#9309,6.);
#1641=CIRCLE('',#9310,4.2705);
#1642=CIRCLE('',#9311,6.);
#1643=CIRCLE('',#9312,1.825);
#1644=CIRCLE('',#9313,5.6245);
#1645=CIRCLE('',#9314,1.825);
#1646=CIRCLE('',#9315,6.);
#1647=CIRCLE('',#9316,4.2705);
#1648=CIRCLE('',#9317,6.);
#1649=CIRCLE('',#9318,1.825);
#1650=CIRCLE('',#9319,5.6245);
#1651=CIRCLE('',#9320,1.825);
#1652=CIRCLE('',#9321,6.);
#1653=CIRCLE('',#9322,4.2705);
#1654=CIRCLE('',#9323,6.);
#1655=CIRCLE('',#9324,1.825);
#1656=CIRCLE('',#9325,5.6245);
#1657=CIRCLE('',#9326,1.825);
#1658=CIRCLE('',#9327,6.);
#1659=CIRCLE('',#9328,4.2705);
#1660=CIRCLE('',#9329,6.);
#1661=CIRCLE('',#9330,1.825);
#1662=CIRCLE('',#9331,5.6245);
#1663=CIRCLE('',#9332,1.825);
#1664=CIRCLE('',#9333,6.);
#1665=CIRCLE('',#9334,4.2705);
#1666=CIRCLE('',#9335,6.);
#1667=CIRCLE('',#9336,1.825);
#1668=CIRCLE('',#9337,5.6245);
#1669=CIRCLE('',#9338,1.825);
#1670=CIRCLE('',#9339,6.);
#1671=CIRCLE('',#9340,4.2705);
#1672=CIRCLE('',#9341,6.);
#1673=CIRCLE('',#9342,1.825);
#1674=CIRCLE('',#9343,5.6245);
#1675=CIRCLE('',#9344,1.825);
#1676=CIRCLE('',#9345,6.);
#1677=CIRCLE('',#9346,4.2705);
#1678=CIRCLE('',#9347,6.);
#1679=CIRCLE('',#9348,1.825);
#1680=CIRCLE('',#9349,5.6245);
#1681=CIRCLE('',#9350,1.825);
#1682=CIRCLE('',#9351,6.);
#1683=CIRCLE('',#9352,4.2705);
#1684=CIRCLE('',#9353,6.);
#1685=CIRCLE('',#9354,1.825);
#1686=CIRCLE('',#9355,5.6245);
#1687=CIRCLE('',#9356,1.825);
#1688=CIRCLE('',#9357,6.);
#1689=CIRCLE('',#9358,4.2705);
#1690=CIRCLE('',#9359,6.);
#1691=CIRCLE('',#9360,1.825);
#1692=CIRCLE('',#9361,5.6245);
#1693=CIRCLE('',#9362,1.825);
#1694=CIRCLE('',#9363,6.);
#1695=CIRCLE('',#9364,4.2705);
#1696=CIRCLE('',#9365,6.);
#1697=CIRCLE('',#9366,1.825);
#1698=CIRCLE('',#9367,5.6245);
#1699=CIRCLE('',#9368,1.825);
#1700=CIRCLE('',#9369,6.);
#1701=CIRCLE('',#9370,4.2705);
#1702=CIRCLE('',#9371,6.);
#1703=CIRCLE('',#9372,1.825);
#1704=CIRCLE('',#9373,5.6245);
#1705=CIRCLE('',#9374,1.825);
#1706=CIRCLE('',#9375,6.);
#1707=CIRCLE('',#9376,4.2705);
#1708=CIRCLE('',#9377,6.);
#1709=CIRCLE('',#9378,1.825);
#1710=CIRCLE('',#9379,5.6245);
#1711=CIRCLE('',#9380,1.825);
#1712=CIRCLE('',#9381,6.);
#1713=CIRCLE('',#9382,4.2705);
#1714=CIRCLE('',#9383,6.);
#1715=CIRCLE('',#9384,1.825);
#1716=CIRCLE('',#9385,5.6245);
#1717=CIRCLE('',#9386,1.825);
#1718=CIRCLE('',#9387,6.);
#1719=CIRCLE('',#9388,4.2705);
#1720=CIRCLE('',#9389,6.);
#1721=CIRCLE('',#9390,1.825);
#1722=CIRCLE('',#9391,5.6245);
#1723=CIRCLE('',#9392,1.825);
#1724=CIRCLE('',#9393,6.);
#1725=CIRCLE('',#9394,4.2705);
#1726=CIRCLE('',#9395,6.);
#1727=CIRCLE('',#9396,1.825);
#1728=CIRCLE('',#9397,5.6245);
#1729=CIRCLE('',#9398,1.825);
#1730=CIRCLE('',#9399,6.);
#1731=CIRCLE('',#9407,3.5);
#1732=CIRCLE('',#9409,3.5);
#1733=CIRCLE('',#9411,4.2705);
#1734=CIRCLE('',#9412,6.);
#1735=CIRCLE('',#9413,1.825);
#1736=CIRCLE('',#9414,5.6245);
#1737=CIRCLE('',#9415,1.825);
#1738=CIRCLE('',#9416,6.);
#1739=CIRCLE('',#9417,4.2705);
#1740=CIRCLE('',#9418,6.);
#1741=CIRCLE('',#9419,1.825);
#1742=CIRCLE('',#9420,5.6245);
#1743=CIRCLE('',#9421,1.825);
#1744=CIRCLE('',#9422,6.);
#1745=CIRCLE('',#9423,4.2705);
#1746=CIRCLE('',#9424,6.);
#1747=CIRCLE('',#9425,1.825);
#1748=CIRCLE('',#9426,5.6245);
#1749=CIRCLE('',#9427,1.825);
#1750=CIRCLE('',#9428,6.);
#1751=CIRCLE('',#9429,4.2705);
#1752=CIRCLE('',#9430,6.);
#1753=CIRCLE('',#9431,1.825);
#1754=CIRCLE('',#9432,5.6245);
#1755=CIRCLE('',#9433,1.825);
#1756=CIRCLE('',#9434,6.);
#1757=CIRCLE('',#9435,4.2705);
#1758=CIRCLE('',#9436,6.);
#1759=CIRCLE('',#9437,1.825);
#1760=CIRCLE('',#9438,5.6245);
#1761=CIRCLE('',#9439,1.825);
#1762=CIRCLE('',#9440,6.);
#1763=CIRCLE('',#9441,4.2705);
#1764=CIRCLE('',#9442,6.);
#1765=CIRCLE('',#9443,1.825);
#1766=CIRCLE('',#9444,5.6245);
#1767=CIRCLE('',#9445,1.825);
#1768=CIRCLE('',#9446,6.);
#1769=CIRCLE('',#9447,4.2705);
#1770=CIRCLE('',#9448,6.);
#1771=CIRCLE('',#9449,1.825);
#1772=CIRCLE('',#9450,5.6245);
#1773=CIRCLE('',#9451,1.825);
#1774=CIRCLE('',#9452,6.);
#1775=CIRCLE('',#9453,4.2705);
#1776=CIRCLE('',#9454,6.);
#1777=CIRCLE('',#9455,1.825);
#1778=CIRCLE('',#9456,5.6245);
#1779=CIRCLE('',#9457,1.825);
#1780=CIRCLE('',#9458,6.);
#1781=CIRCLE('',#9459,4.2705);
#1782=CIRCLE('',#9460,6.);
#1783=CIRCLE('',#9461,1.825);
#1784=CIRCLE('',#9462,5.6245);
#1785=CIRCLE('',#9463,1.825);
#1786=CIRCLE('',#9464,6.);
#1787=CIRCLE('',#9465,4.2705);
#1788=CIRCLE('',#9466,6.);
#1789=CIRCLE('',#9467,1.825);
#1790=CIRCLE('',#9468,5.6245);
#1791=CIRCLE('',#9469,1.825);
#1792=CIRCLE('',#9470,6.);
#1793=CIRCLE('',#9471,4.2705);
#1794=CIRCLE('',#9472,6.);
#1795=CIRCLE('',#9473,1.825);
#1796=CIRCLE('',#9474,5.6245);
#1797=CIRCLE('',#9475,1.825);
#1798=CIRCLE('',#9476,6.);
#1799=CIRCLE('',#9477,4.2705);
#1800=CIRCLE('',#9478,6.);
#1801=CIRCLE('',#9479,1.825);
#1802=CIRCLE('',#9480,5.6245);
#1803=CIRCLE('',#9481,1.825);
#1804=CIRCLE('',#9482,6.);
#1805=CIRCLE('',#9483,4.2705);
#1806=CIRCLE('',#9484,6.);
#1807=CIRCLE('',#9485,1.825);
#1808=CIRCLE('',#9486,5.6245);
#1809=CIRCLE('',#9487,1.825);
#1810=CIRCLE('',#9488,6.);
#1811=CIRCLE('',#9489,4.2705);
#1812=CIRCLE('',#9490,6.);
#1813=CIRCLE('',#9491,1.825);
#1814=CIRCLE('',#9492,5.6245);
#1815=CIRCLE('',#9493,1.825);
#1816=CIRCLE('',#9494,6.);
#1817=CIRCLE('',#9495,4.2705);
#1818=CIRCLE('',#9496,6.);
#1819=CIRCLE('',#9497,1.825);
#1820=CIRCLE('',#9498,5.6245);
#1821=CIRCLE('',#9499,1.825);
#1822=CIRCLE('',#9500,6.);
#1823=CIRCLE('',#9501,4.2705);
#1824=CIRCLE('',#9502,6.);
#1825=CIRCLE('',#9503,1.825);
#1826=CIRCLE('',#9504,5.6245);
#1827=CIRCLE('',#9505,1.825);
#1828=CIRCLE('',#9506,6.);
#1829=CIRCLE('',#9526,3.38723968927587);
#1830=CIRCLE('',#9527,3.38723968927705);
#1831=CIRCLE('',#9535,3.38723968881628);
#1832=CIRCLE('',#9536,3.38723968881655);
#1833=CIRCLE('',#9544,3.38723968906544);
#1834=CIRCLE('',#9545,3.38723968906746);
#1835=CIRCLE('',#9553,3.38723968947446);
#1836=CIRCLE('',#9554,3.38723968947391);
#1837=CIRCLE('',#9562,3.38723968881629);
#1838=CIRCLE('',#9563,3.38723968881655);
#1839=CIRCLE('',#9571,3.38723968927622);
#1840=CIRCLE('',#9572,3.38723968927713);
#1841=CIRCLE('',#9580,3.38723968906544);
#1842=CIRCLE('',#9581,3.38723968906746);
#1843=CIRCLE('',#9589,3.38723968947446);
#1844=CIRCLE('',#9590,3.38723968947391);
#1845=CIRCLE('',#9598,3.38723968881628);
#1846=CIRCLE('',#9599,3.38723968881655);
#1847=CIRCLE('',#9607,3.38723968927587);
#1848=CIRCLE('',#9608,3.38723968927705);
#1849=CIRCLE('',#9616,3.38723968906544);
#1850=CIRCLE('',#9617,3.38723968906746);
#1851=CIRCLE('',#9625,3.38723968947446);
#1852=CIRCLE('',#9626,3.38723968947391);
#1853=CIRCLE('',#9634,3.38723968881629);
#1854=CIRCLE('',#9635,3.38723968881655);
#1855=CIRCLE('',#9643,3.38723968927622);
#1856=CIRCLE('',#9644,3.38723968927713);
#1857=CIRCLE('',#9652,3.38723968906544);
#1858=CIRCLE('',#9653,3.38723968906746);
#1859=CIRCLE('',#9661,3.38723968916632);
#1860=CIRCLE('',#9662,3.38723968916588);
#1861=CIRCLE('',#9669,3.);
#1862=CIRCLE('',#9671,3.);
#1863=CIRCLE('',#9673,3.);
#1864=CIRCLE('',#9674,3.);
#1865=CIRCLE('',#9676,4.705);
#1866=CIRCLE('',#9678,5.);
#1867=CIRCLE('',#9687,1.5);
#1868=CIRCLE('',#9691,1.5);
#1869=CIRCLE('',#9696,3.2);
#1870=CIRCLE('',#9697,1.6);
#1871=CIRCLE('',#9699,1.6);
#1872=CIRCLE('',#9701,3.2);
#1873=CIRCLE('',#9703,0.25);
#1874=CIRCLE('',#9706,1.331411920116);
#1875=CIRCLE('',#9708,1.116987298108);
#1876=CIRCLE('',#9710,1.116987298108);
#1877=CIRCLE('',#9713,0.4);
#1878=CIRCLE('',#9714,1.331411920116);
#1879=CIRCLE('',#9715,0.4);
#1880=CIRCLE('',#9716,1.707288968431);
#1881=CIRCLE('',#9720,3.);
#1882=CIRCLE('',#9722,3.);
#1883=CIRCLE('',#9723,3.);
#1884=CIRCLE('',#9724,1.092121597166);
#1885=CIRCLE('',#9727,1.092121597166);
#1886=CIRCLE('',#9728,1.092121597166);
#1887=CIRCLE('',#9730,1.092121597166);
#1888=CIRCLE('',#9781,1.00153545743576);
#1889=CIRCLE('',#9782,1.);
#1890=CIRCLE('',#9784,4.3);
#1891=CIRCLE('',#9785,49.4822348431);
#1892=CIRCLE('',#9787,49.4822348431);
#1893=CIRCLE('',#9788,4.3);
#1894=CIRCLE('',#9790,4.3);
#1895=CIRCLE('',#9791,49.4822348431);
#1896=CIRCLE('',#9793,49.4822348431);
#1897=CIRCLE('',#9794,4.3);
#1898=CIRCLE('',#9796,1.0015363217743);
#1899=CIRCLE('',#9797,1.);
#1900=CIRCLE('',#9798,1.000000000559);
#1901=CIRCLE('',#9800,0.5);
#1902=CIRCLE('',#9801,3.8);
#1903=CIRCLE('',#9802,0.5);
#1904=CIRCLE('',#9803,0.5000047256893);
#1905=CIRCLE('',#9805,0.5);
#1906=CIRCLE('',#9806,0.5);
#1907=CIRCLE('',#9807,49.98193025661);
#1908=CIRCLE('',#9808,0.5);
#1909=CIRCLE('',#9809,0.512087492200193);
#1910=CIRCLE('',#9811,0.5);
#1911=CIRCLE('',#9815,0.5);
#1912=CIRCLE('',#9817,3.8);
#1913=CIRCLE('',#9819,3.8);
#1914=CIRCLE('',#9821,3.8);
#1915=CIRCLE('',#9823,3.8);
#1916=CIRCLE('',#9824,3.8);
#1917=CIRCLE('',#9825,0.4999999975627);
#1918=CIRCLE('',#9826,0.5);
#1919=CIRCLE('',#9827,0.5);
#1920=CIRCLE('',#9828,0.5);
#1921=CIRCLE('',#9829,0.5);
#1922=CIRCLE('',#9830,0.5000047256893);
#1923=CIRCLE('',#9831,0.5);
#1924=CIRCLE('',#9833,0.5);
#1925=CIRCLE('',#9834,49.98193025661);
#1926=CIRCLE('',#9835,0.5);
#1927=CIRCLE('',#9836,0.512090006867649);
#1928=CIRCLE('',#9838,0.5);
#1929=CIRCLE('',#9839,0.5);
#1930=CIRCLE('',#9841,0.5);
#1931=CIRCLE('',#9842,0.5);
#1932=CIRCLE('',#9843,0.5);
#1933=CIRCLE('',#9845,0.5);
#1934=CIRCLE('',#9846,1.00152854151208);
#1935=CIRCLE('',#9847,0.512097491395091);
#1936=CIRCLE('',#9849,49.98193025661);
#1937=CIRCLE('',#9850,0.5);
#1938=CIRCLE('',#9851,0.4999999975627);
#1939=CIRCLE('',#9852,0.4999999999921);
#1940=CIRCLE('',#9854,3.8);
#1941=CIRCLE('',#9855,0.5);
#1942=CIRCLE('',#9856,1.);
#1943=CIRCLE('',#9857,0.9999999994882);
#1944=CIRCLE('',#9858,0.5000000000015);
#1945=CIRCLE('',#9859,0.5);
#1946=CIRCLE('',#9860,0.5);
#1947=CIRCLE('',#9861,0.5);
#1948=CIRCLE('',#9862,1.000001436707);
#1949=CIRCLE('',#9864,3.8);
#1950=CIRCLE('',#9866,3.3);
#1951=CIRCLE('',#9867,0.5);
#1952=CIRCLE('',#9868,3.8);
#1953=CIRCLE('',#9870,0.4999999999921);
#1954=CIRCLE('',#9871,0.5);
#1955=CIRCLE('',#9872,1.000000783793);
#1956=CIRCLE('',#9873,1.);
#1957=CIRCLE('',#9875,1.00152887460701);
#1958=CIRCLE('',#9876,0.5);
#1959=CIRCLE('',#9877,0.5);
#1960=CIRCLE('',#9878,0.512097487101245);
#1961=CIRCLE('',#9880,49.98193025661);
#1962=CIRCLE('',#9883,0.5);
#1963=CIRCLE('',#9885,0.5);
#1964=CIRCLE('',#9887,0.5);
#1965=CIRCLE('',#9889,0.5);
#1966=CIRCLE('',#9890,0.5);
#1967=CIRCLE('',#9891,0.5);
#1968=CIRCLE('',#9893,0.5);
#1969=CIRCLE('',#9894,0.5);
#1970=CIRCLE('',#9896,0.5);
#1971=CIRCLE('',#9897,0.5);
#1972=CIRCLE('',#9900,2.6);
#1973=CIRCLE('',#9901,2.6);
#1974=CIRCLE('',#9903,2.6);
#1975=CIRCLE('',#9905,1.25);
#1976=CIRCLE('',#9906,1.25);
#1977=CIRCLE('',#9908,1.25);
#1978=CIRCLE('',#9910,2.5);
#1979=CIRCLE('',#9912,2.5);
#1980=CIRCLE('',#9914,0.5);
#1981=CIRCLE('',#9916,0.5);
#1982=CIRCLE('',#9917,0.5);
#1983=CIRCLE('',#9918,0.5000000000015);
#1984=CIRCLE('',#9919,0.5);
#1985=CIRCLE('',#9923,2.35);
#1986=CIRCLE('',#9937,2.35);
#1987=CIRCLE('',#9939,1.1);
#1988=CIRCLE('',#9941,0.7);
#1989=CIRCLE('',#9942,1.1);
#1990=CIRCLE('',#9943,1.1);
#1991=CIRCLE('',#9945,1.25);
#1992=CIRCLE('',#9946,1.25);
#1993=CIRCLE('',#9989,7.5);
#1994=CIRCLE('',#9990,6.);
#1995=CIRCLE('',#9992,5.);
#1996=CIRCLE('',#9993,5.);
#1997=CIRCLE('',#9994,1.);
#1998=CIRCLE('',#9996,5.);
#1999=CIRCLE('',#9998,4.);
#2000=CIRCLE('',#10000,4.);
#2001=CIRCLE('',#10001,4.);
#2002=CIRCLE('',#10003,4.);
#2003=CIRCLE('',#10007,6.);
#2004=CIRCLE('',#10009,6.);
#2005=CIRCLE('',#10011,6.75);
#2006=CIRCLE('',#10013,6.75);
#2007=CIRCLE('',#10015,7.5);
#2008=CIRCLE('',#10016,1.5);
#2009=CIRCLE('',#10017,2.5);
#2010=CIRCLE('',#10018,1.5);
#2011=CIRCLE('',#10019,7.5);
#2012=CIRCLE('',#10020,1.25);
#2013=CIRCLE('',#10022,1.25);
#2014=CIRCLE('',#10024,9.);
#2015=CIRCLE('',#10025,2.5);
#2016=CIRCLE('',#10027,0.5);
#2017=CIRCLE('',#10028,1.);
#2018=CIRCLE('',#10029,1.);
#2019=CIRCLE('',#10031,1.);
#2020=CIRCLE('',#10032,8.);
#2021=CIRCLE('',#10033,1.);
#2022=CIRCLE('',#10035,1.);
#2023=CIRCLE('',#10037,0.5);
#2024=CIRCLE('',#10038,0.5);
#2025=CIRCLE('',#10040,0.5);
#2026=CIRCLE('',#10043,0.5);
#2027=CIRCLE('',#10045,3.);
#2028=CIRCLE('',#10047,3.);
#2029=CIRCLE('',#10049,0.5);
#2030=CIRCLE('',#10051,0.5);
#2031=CIRCLE('',#10054,1.);
#2032=CIRCLE('',#10056,0.5);
#2033=CIRCLE('',#10058,8.);
#2034=CIRCLE('',#10059,0.5);
#2035=CIRCLE('',#10061,8.);
#2036=CIRCLE('',#10062,8.);
#2037=CIRCLE('',#10064,0.5);
#2038=CIRCLE('',#10066,0.5);
#2039=CIRCLE('',#10068,1.);
#2040=CIRCLE('',#10072,0.5);
#2041=CIRCLE('',#10073,0.4999999959631);
#2042=CIRCLE('',#10076,0.9999999999978);
#2043=CIRCLE('',#10077,0.5000000000709);
#2044=CIRCLE('',#10078,0.5);
#2045=CIRCLE('',#10079,1.);
#2046=CIRCLE('',#10080,0.5000000000042);
#2047=CIRCLE('',#10082,1.);
#2048=CIRCLE('',#10083,0.5);
#2049=CIRCLE('',#10084,0.5);
#2050=CIRCLE('',#10085,0.5);
#2051=CIRCLE('',#10087,2.5);
#2052=CIRCLE('',#10088,3.6);
#2053=CIRCLE('',#10090,3.6);
#2054=CIRCLE('',#10092,3.23);
#2055=CIRCLE('',#10094,3.23);
#2056=CIRCLE('',#10103,1.);
#2057=CIRCLE('',#10105,0.50000015263);
#2058=CIRCLE('',#10113,0.5000000000013);
#2059=CIRCLE('',#10116,0.5000003490389);
#2060=CIRCLE('',#10117,0.5000000000992);
#2061=CIRCLE('',#10120,0.5);
#2062=CIRCLE('',#10122,3.);
#2063=CIRCLE('',#10123,0.5);
#2064=CIRCLE('',#10125,0.5);
#2065=CIRCLE('',#10127,0.5);
#2066=CIRCLE('',#10134,6.2);
#2067=CIRCLE('',#10135,4.);
#2068=CIRCLE('',#10137,4.);
#2069=CIRCLE('',#10139,6.2);
#2070=CIRCLE('',#10141,0.8);
#2071=CIRCLE('',#10144,3.125);
#2072=CIRCLE('',#10146,3.125);
#2073=CIRCLE('',#10148,3.5);
#2074=CIRCLE('',#10150,1.);
#2075=CIRCLE('',#10152,1.);
#2076=CIRCLE('',#10153,1.);
#2077=CIRCLE('',#10154,1.);
#2078=CIRCLE('',#10155,1.);
#2079=CIRCLE('',#10156,1.);
#2080=CIRCLE('',#10157,4.);
#2081=CIRCLE('',#10173,0.75);
#2082=CIRCLE('',#10174,2.6);
#2083=CIRCLE('',#10177,3.8);
#2084=CIRCLE('',#10178,2.5);
#2085=CIRCLE('',#10180,2.5);
#2086=CIRCLE('',#10182,3.8);
#2087=CIRCLE('',#10186,6.65);
#2088=CIRCLE('',#10187,5.65);
#2089=CIRCLE('',#10189,6.65);
#2090=CIRCLE('',#10191,50.);
#2091=CIRCLE('',#10193,5.65);
#2092=CIRCLE('',#10194,5.65);
#2093=CIRCLE('',#10196,49.5);
#2094=B_SPLINE_CURVE_WITH_KNOTS('',3,(#12552,#12553,#12554,#12555,#12556,
#12557,#12558,#12559,#12560,#12561,#12562,#12563,#12564,#12565,#12566,#12567,
#12568,#12569,#12570,#12571,#12572,#12573,#12574,#12575,#12576,#12577,#12578,
#12579,#12580,#12581,#12582,#12583,#12584,#12585,#12586,#12587,#12588,#12589,
#12590,#12591,#12592,#12593,#12594,#12595,#12596,#12597,#12598,#12599,#12600,
#12601,#12602,#12603),.UNSPECIFIED.,.F.,.F.,(4,2,2,2,2,2,2,2,2,2,2,2,2,
2,2,2,2,2,2,2,2,2,2,2,2,4),(2.14502562436384,2.18712156060152,2.27622566969401,
2.32089041959239,2.36538765547986,2.45376151983945,2.4982791356259,2.54277391955066,
2.58737028222014,2.67694633287528,2.72140315755377,2.76570334662978,2.85489268765083,
2.89952573822096,2.94404144281776,3.03280270260246,3.07729710502769,3.12175138462939,
3.16636646470874,3.25602651891706,3.30048521246139,3.34474880671133,3.43400504589525,
3.46917173238361,3.52205339439103,3.57498321837689),.UNSPECIFIED.);
#2095=B_SPLINE_CURVE_WITH_KNOTS('',3,(#12612,#12613,#12614,#12615,#12616,
#12617,#12618,#12619,#12620,#12621,#12622,#12623,#12624,#12625,#12626,#12627,
#12628,#12629,#12630,#12631,#12632,#12633,#12634,#12635,#12636,#12637,#12638,
#12639,#12640,#12641,#12642,#12643,#12644,#12645,#12646,#12647,#12648,#12649,
#12650,#12651,#12652,#12653,#12654,#12655,#12656,#12657,#12658,#12659,#12660,
#12661,#12662,#12663,#12664,#12665),.UNSPECIFIED.,.F.,.F.,(4,2,2,2,2,2,
2,2,2,2,2,2,2,2,2,2,2,2,2,2,2,2,2,2,2,2,4),(0.714866971049495,0.72011528738726,
0.809316049507178,0.853618221320616,0.898069747103448,0.987629225690559,
1.03222343976808,1.07672364266554,1.12123519646787,1.2096051565493,1.25409829695009,
1.29876912997362,1.3878844113741,1.43223900550291,1.47669632479167,1.56609535939874,
1.61066571850577,1.65521605463951,1.69976297657141,1.78749336285472,1.87522704043972,
1.91977971115659,1.96432372106055,2.00889621585214,2.09830830202093,2.14277057212069,
2.14502562436384),.UNSPECIFIED.);
#2096=B_SPLINE_CURVE_WITH_KNOTS('',3,(#12666,#12667,#12668,#12669,#12670,
#12671,#12672,#12673,#12674,#12675,#12676,#12677,#12678,#12679,#12680,#12681,
#12682,#12683,#12684,#12685,#12686,#12687,#12688,#12689,#12690,#12691,#12692,
#12693,#12694,#12695,#12696,#12697,#12698,#12699,#12700,#12701,#12702,#12703,
#12704,#12705,#12706,#12707,#12708,#12709,#12710,#12711,#12712,#12713,#12714,
#12715,#12716,#12717),.UNSPECIFIED.,.F.,.F.,(4,2,2,2,2,2,2,2,2,2,2,2,2,
2,2,2,2,2,2,2,2,2,2,2,2,4),(1.0000000638874E-6,0.0529432525790578,0.105836830109484,
0.141014199970554,0.230281459970461,0.274545373941572,0.318998103364306,
0.408638735078214,0.453251377644336,0.497709833041615,0.542197575952712,
0.630949700434586,0.675460895509643,0.720099378845943,0.809300087921693,
0.853602222275693,0.898053716322623,0.98761314604962,1.03220733122512,1.07670749657416,
1.12121901503127,1.20958897541431,1.25408208681528,1.29875288369215,1.3878681140945,
1.4299206384854),.UNSPECIFIED.);
#2097=B_SPLINE_CURVE_WITH_KNOTS('',3,(#12723,#12724,#12725,#12726,#12727,
#12728,#12729,#12730,#12731,#12732,#12733,#12734,#12735,#12736,#12737,#12738,
#12739,#12740,#12741,#12742,#12743,#12744,#12745,#12746,#12747,#12748,#12749,
#12750),.UNSPECIFIED.,.F.,.F.,(4,2,2,2,2,2,2,2,2,2,2,2,2,4),(2.86008561622508,
2.89952817344818,2.94404372203974,3.03280213002521,3.0772967112602,3.12175133798389,
3.1663662648552,3.25602576693473,3.30048442341296,3.34474833908933,3.4340039704133,
3.46917521608883,3.52206341792462,3.57496743915675),.UNSPECIFIED.);
#2098=B_SPLINE_CURVE_WITH_KNOTS('',3,(#12751,#12752,#12753,#12754,#12755,
#12756,#12757,#12758,#12759,#12760,#12761,#12762,#12763,#12764,#12765,#12766,
#12767,#12768,#12769,#12770,#12771,#12772,#12773,#12774,#12775,#12776,#12777,
#12778),.UNSPECIFIED.,.F.,.F.,(4,2,2,2,2,2,2,2,2,2,2,2,2,4),(1.94943175665867E-5,
0.0529485196822737,0.105848261883074,0.141029742242418,0.230297056939625,
0.274561007064076,0.319013767542678,0.408654455292159,0.453267127336578,
0.497725619328092,0.542213396377112,0.630965543886577,0.675476768340537,
0.714866971049495),.UNSPECIFIED.);
#2099=B_SPLINE_CURVE_WITH_KNOTS('',3,(#12779,#12780,#12781,#12782,#12783,
#12784,#12785,#12786,#12787,#12788,#12789,#12790,#12791,#12792,#12793,#12794,
#12795,#12796,#12797,#12798,#12799,#12800,#12801,#12802,#12803,#12804,#12805,
#12806,#12807,#12808,#12809,#12810,#12811,#12812,#12813,#12814,#12815,#12816,
#12817,#12818,#12819,#12820,#12821,#12822,#12823,#12824,#12825,#12826,#12827,
#12828,#12829,#12830,#12831,#12832),.UNSPECIFIED.,.F.,.F.,(4,2,2,2,2,2,
2,2,2,2,2,2,2,2,2,2,2,2,2,2,2,2,2,2,2,2,4),(1.4299206384854,1.43222267048901,
1.47667998786036,1.56607905094836,1.61064941319619,1.65519974160521,1.69974665739337,
1.78747715470346,1.87521086672082,1.91976354413251,1.96430756284278,2.0088800513862,
2.09829209315722,2.1427543640379,2.18710539147204,2.27620954348202,2.3208743295338,
2.36537159165582,2.45374542602367,2.49826307689474,2.54275789886887,2.58735428763111,
2.67693037733929,2.72138723206035,2.76568745901495,2.85487684558239,2.86008592505616),
 .UNSPECIFIED.);
#2100=B_SPLINE_CURVE_WITH_KNOTS('',3,(#12837,#12838,#12839,#12840,#12841,
#12842,#12843,#12844,#12845,#12846,#12847,#12848,#12849,#12850,#12851,#12852,
#12853,#12854,#12855,#12856,#12857,#12858,#12859,#12860,#12861,#12862,#12863,
#12864,#12865,#12866,#12867,#12868,#12869,#12870,#12871,#12872,#12873,#12874,
#12875,#12876,#12877,#12878,#12879,#12880,#12881,#12882,#12883,#12884,#12885,
#12886,#12887,#12888,#12889,#12890),.UNSPECIFIED.,.F.,.F.,(4,2,2,2,2,2,
2,2,2,2,2,2,2,2,2,2,2,2,2,2,2,2,2,2,2,2,4),(1.42992065923686,1.43223977969029,
1.47669703588382,1.56609757048888,1.61066812124717,1.65521810141441,1.69976474727003,
1.787500783217,1.87523625403487,1.91978929642496,1.9643337839075,2.00890599824737,
2.09831591280814,2.14277825682906,2.18712978796684,2.27623305258158,2.32089811540851,
2.36539517067194,2.45376453680926,2.49828241705732,2.54277761521628,2.58737378670215,
2.67694877874516,2.72140561612856,2.76570621753569,2.85489484220979,2.86008561622508),
 .UNSPECIFIED.);
#2101=B_SPLINE_CURVE_WITH_KNOTS('',3,(#12892,#12893,#12894,#12895,#12896,
#12897,#12898,#12899,#12900,#12901,#12902,#12903,#12904,#12905,#12906,#12907,
#12908,#12909,#12910,#12911,#12912,#12913,#12914,#12915,#12916,#12917,#12918,
#12919),.UNSPECIFIED.,.F.,.F.,(4,2,2,2,2,2,2,2,2,2,2,2,2,4),(2.86008592505616,
2.89950993164355,2.94402566297617,3.03278692566152,3.07728136145645,3.1217356777481,
3.16635078468632,3.2560108880428,3.30046961064402,3.3447332409437,3.43398952787311,
3.46916115583476,3.52205022597488,3.5749680558315),.UNSPECIFIED.);
#2102=B_SPLINE_CURVE_WITH_KNOTS('',3,(#12920,#12921,#12922,#12923,#12924,
#12925,#12926,#12927,#12928,#12929,#12930,#12931,#12932,#12933,#12934,#12935,
#12936,#12937,#12938,#12939,#12940,#12941,#12942,#12943,#12944,#12945,#12946,
#12947),.UNSPECIFIED.,.F.,.F.,(4,2,2,2,2,2,2,2,2,2,2,2,2,4),(3.26034835787405E-5,
0.0529536178204587,0.105858380107734,0.141043201484947,0.23031053022423,
0.274574474417073,0.319027236436972,0.408667936702993,0.453280612706133,
0.497739098337324,0.542226872563317,0.630979078799732,0.675490307249623,
0.714880126578297),.UNSPECIFIED.);
#2103=B_SPLINE_CURVE_WITH_KNOTS('',3,(#12952,#12953,#12954,#12955,#12956,
#12957,#12958,#12959,#12960,#12961,#12962,#12963,#12964,#12965,#12966,#12967,
#12968,#12969,#12970,#12971,#12972,#12973,#12974,#12975,#12976,#12977,#12978,
#12979,#12980,#12981,#12982,#12983,#12984,#12985,#12986,#12987,#12988,#12989,
#12990,#12991,#12992,#12993,#12994,#12995,#12996,#12997,#12998,#12999,#13000,
#13001,#13002,#13003),.UNSPECIFIED.,.F.,.F.,(4,2,2,2,2,2,2,2,2,2,2,2,2,
2,2,2,2,2,2,2,2,2,2,2,2,4),(1.00000006295758E-6,0.0529473084571401,0.105845005097466,
0.141024979753782,0.230292688622603,0.274556378984213,0.319009143379118,
0.408650170385479,0.453262931403543,0.497721148223992,0.542208775050986,
0.630962893371619,0.675474208251199,0.720112502998726,0.809313740248424,
0.853615587847759,0.898067083267914,0.987627259379836,1.03222159080723,
1.07672147192959,1.12123281554438,1.20960590707816,1.25409915637214,1.29876974423772,
1.38788560124205,1.42992065923686),.UNSPECIFIED.);
#2104=B_SPLINE_CURVE_WITH_KNOTS('',3,(#13004,#13005,#13006,#13007,#13008,
#13009,#13010,#13011,#13012,#13013,#13014,#13015,#13016,#13017,#13018,#13019,
#13020,#13021,#13022,#13023,#13024,#13025,#13026,#13027,#13028,#13029,#13030,
#13031,#13032,#13033,#13034,#13035,#13036,#13037,#13038,#13039,#13040,#13041,
#13042,#13043,#13044,#13045,#13046,#13047,#13048,#13049,#13050,#13051,#13052,
#13053,#13054,#13055,#13056,#13057),.UNSPECIFIED.,.F.,.F.,(4,2,2,2,2,2,
2,2,2,2,2,2,2,2,2,2,2,2,2,2,2,2,2,2,2,2,4),(0.714880126578297,0.720128821383708,
0.809329599837282,0.853631763893768,0.898083290245698,0.987642791510278,
1.03223701035026,1.0767372055681,1.12124875484821,1.20961880657035,1.25411195148966,
1.29878277901107,1.38789807957833,1.43225266331332,1.47670998136068,1.56610905963984,
1.61067942473116,1.65522975133509,1.69977666599439,1.78750721371321,1.87524094334269,
1.91979362512494,1.96433764910848,2.0089101364871,2.09832216229164,2.14278443501037,
2.14503879498624),.UNSPECIFIED.);
#2105=B_SPLINE_CURVE_WITH_KNOTS('',3,(#13060,#13061,#13062,#13063,#13064,
#13065),.UNSPECIFIED.,.F.,.F.,(4,2,4),(-0.0939490999539409,-0.0470050902016758,
-1.84510844862747E-5),.UNSPECIFIED.);
#2106=B_SPLINE_CURVE_WITH_KNOTS('',3,(#13067,#13068,#13069,#13070,#13071,
#13072),.UNSPECIFIED.,.F.,.F.,(4,2,4),(-0.0245511647397311,-0.012301164739731,
-4.98173261989365E-5),.UNSPECIFIED.);
#2107=B_SPLINE_CURVE_WITH_KNOTS('',3,(#13074,#13075,#13076,#13077,#13078,
#13079),.UNSPECIFIED.,.F.,.F.,(4,2,4),(-0.024549949138571,-0.0123012966393727,
-5.12966393727537E-5),.UNSPECIFIED.);
#2108=B_SPLINE_CURVE_WITH_KNOTS('',3,(#13080,#13081,#13082,#13083,#13084,
#13085),.UNSPECIFIED.,.F.,.F.,(4,2,4),(-0.0940281721018956,-0.0470425165176012,
-9.75232268322135E-5),.UNSPECIFIED.);
#2109=B_SPLINE_CURVE_WITH_KNOTS('',3,(#13088,#13089,#13090,#13091,#13092,
#13093,#13094,#13095,#13096,#13097,#13098,#13099,#13100,#13101,#13102,#13103,
#13104,#13105,#13106,#13107,#13108,#13109,#13110,#13111,#13112,#13113,#13114,
#13115,#13116,#13117,#13118,#13119,#13120,#13121,#13122,#13123,#13124,#13125,
#13126,#13127,#13128,#13129,#13130,#13131,#13132,#13133,#13134,#13135,#13136,
#13137,#13138,#13139),.UNSPECIFIED.,.F.,.F.,(4,2,2,2,2,2,2,2,2,2,2,2,2,
2,2,2,2,2,2,2,2,2,2,2,2,4),(2.14503879498624,2.1871354385732,2.27623952298521,
2.32090428141422,2.36540151183267,2.45377524812087,2.49829287105407,2.54278766638035,
2.58738402328276,2.67696004328402,2.72141686796932,2.76571706839078,2.85490638840218,
2.89953944658785,2.9440551464135,3.03281632471489,3.07731073186083,3.12176502096226,
3.16638009635026,3.25604013423686,3.30049882637889,3.3447624293985,3.43401865064795,
3.46918523193177,3.52206672757312,3.5749963877086),.UNSPECIFIED.);
#2110=B_SPLINE_CURVE_WITH_KNOTS('',3,(#13285,#13286,#13287,#13288,#13289,
#13290,#13291,#13292,#13293,#13294,#13295,#13296,#13297,#13298,#13299,#13300,
#13301,#13302,#13303,#13304,#13305,#13306,#13307,#13308,#13309,#13310,#13311,
#13312,#13313,#13314,#13315,#13316,#13317,#13318,#13319,#13320,#13321,#13322,
#13323,#13324,#13325,#13326,#13327,#13328,#13329,#13330,#13331,#13332,#13333,
#13334,#13335,#13336,#13337,#13338,#13339,#13340,#13341,#13342,#13343,#13344,
#13345,#13346,#13347,#13348,#13349,#13350,#13351,#13352,#13353,#13354,#13355,
#13356,#13357,#13358,#13359,#13360,#13361,#13362,#13363,#13364,#13365,#13366,
#13367,#13368,#13369,#13370),.UNSPECIFIED.,.F.,.F.,(4,2,2,2,2,2,2,2,2,2,
2,2,2,2,2,2,2,2,2,2,2,2,2,2,2,2,2,2,2,2,2,2,2,2,2,2,2,2,2,2,2,2,4),(-3.85123506044155,
-3.78487541403508,-3.71861843740112,-3.63108565202321,-3.56307062788875,
-3.48955351073223,-3.39011116153264,-3.28756064765323,-3.21142501850155,
-3.13819263854922,-3.04447171553351,-2.91317755199343,-2.82034930299588,
-2.74581519796329,-2.6482372951938,-2.50362504362689,-2.40302458529268,
-2.32466081344229,-2.23654291442963,-2.1160510015302,-2.00788420853694,
-1.92564309108704,-1.84340197363715,-1.73523518064389,-1.61474326774443,
-1.52662536873178,-1.44826159688142,-1.34766113854725,-1.20304888698038,
-1.10547098421093,-1.03093687917837,-0.938108630180896,-0.806814466640977,
-0.713093543625373,-0.63986116367313,-0.563725534521538,-0.461175020642281,
-0.361732671442888,-0.288215554286479,-0.220200530152141,-0.132667744774381,
-0.0664107174211822,-5.07026194194161E-5),.UNSPECIFIED.);
#2111=B_SPLINE_CURVE_WITH_KNOTS('',3,(#13513,#13514,#13515,#13516,#13517,
#13518,#13519,#13520,#13521,#13522,#13523,#13524,#13525,#13526,#13527,#13528,
#13529,#13530,#13531,#13532,#13533,#13534,#13535,#13536,#13537,#13538,#13539,
#13540,#13541,#13542,#13543,#13544,#13545,#13546,#13547,#13548,#13549,#13550,
#13551,#13552,#13553,#13554,#13555,#13556,#13557,#13558,#13559,#13560,#13561,
#13562,#13563,#13564,#13565,#13566,#13567,#13568,#13569,#13570,#13571,#13572,
#13573,#13574,#13575,#13576,#13577,#13578,#13579,#13580,#13581,#13582,#13583,
#13584,#13585,#13586,#13587,#13588,#13589,#13590,#13591,#13592,#13593,#13594,
#13595,#13596,#13597,#13598),.UNSPECIFIED.,.F.,.F.,(4,2,2,2,2,2,2,2,2,2,
2,2,2,2,2,2,2,2,2,2,2,2,2,2,2,2,2,2,2,2,2,2,2,2,2,2,2,2,2,2,2,2,4),(-3.85123405850883,
-3.78487517864781,-3.71861815415721,-3.63108537256124,-3.56307035136544,
-3.48955323738529,-3.39011089248222,-3.28756038303362,-3.21142475717148,
-3.13819238038325,-3.04447146141686,-2.91317730354951,-2.82034905856273,
-2.74581495675049,-2.64823705819698,-2.50362481287822,-2.40302435889057,
-2.32466059042599,-2.23654269522057,-2.11605078752714,-2.00788399920737,
-1.9256428853108,-1.84340177141424,-1.73523498309445,-1.61474307540097,
-1.52662518019554,-1.44826141173097,-1.34766095774334,-1.2030487124246,
-1.10547081387111,-1.03093671205888,-0.938108467072148,-0.806814309204971,
-0.713093390238713,-0.639861013450582,-0.563725387588521,-0.461174878140013,
-0.361732533237043,-0.288215419256955,-0.220200398061198,-0.132667616465267,
-0.066410653998432,-5.0998807349829E-5),.UNSPECIFIED.);
#2112=B_SPLINE_CURVE_WITH_KNOTS('',3,(#13599,#13600,#13601,#13602,#13603,
#13604),.UNSPECIFIED.,.F.,.F.,(4,2,4),(-0.0940291329153355,-0.0470424937982037,
-9.84840459302137E-5),.UNSPECIFIED.);
#2113=B_SPLINE_CURVE_WITH_KNOTS('',3,(#13607,#13608,#13609,#13610,#13611,
#13612),.UNSPECIFIED.,.F.,.F.,(4,2,4),(-0.024552644052882,-0.0123012966393732,
-5.12966393733071E-5),.UNSPECIFIED.);
#2114=B_SPLINE_CURVE_WITH_KNOTS('',3,(#13614,#13615,#13616,#13617,#13618,
#13619),.UNSPECIFIED.,.F.,.F.,(4,2,4),(-0.0245511874584252,-0.0123011874584247,
-5.25349590649871E-5),.UNSPECIFIED.);
#2115=B_SPLINE_CURVE_WITH_KNOTS('',3,(#13620,#13621,#13622,#13623,#13624,
#13625),.UNSPECIFIED.,.F.,.F.,(4,2,4),(-0.0939527595126648,-0.0470077662219547,
-2.21106376590829E-5),.UNSPECIFIED.);
#2116=B_SPLINE_CURVE_WITH_KNOTS('',3,(#13767,#13768,#13769,#13770,#13771,
#13772,#13773,#13774,#13775,#13776,#13777,#13778,#13779,#13780,#13781,#13782,
#13783,#13784,#13785,#13786,#13787,#13788,#13789,#13790,#13791,#13792,#13793,
#13794,#13795,#13796,#13797,#13798,#13799,#13800,#13801,#13802,#13803,#13804,
#13805,#13806,#13807,#13808,#13809,#13810,#13811,#13812,#13813,#13814,#13815,
#13816,#13817,#13818,#13819,#13820,#13821,#13822,#13823,#13824,#13825,#13826,
#13827,#13828,#13829,#13830,#13831,#13832,#13833,#13834,#13835,#13836,#13837,
#13838,#13839,#13840,#13841,#13842,#13843,#13844,#13845,#13846,#13847,#13848,
#13849,#13850,#13851,#13852),.UNSPECIFIED.,.F.,.F.,(4,2,2,2,2,2,2,2,2,2,
2,2,2,2,2,2,2,2,2,2,2,2,2,2,2,2,2,2,2,2,2,2,2,2,2,2,2,2,2,2,2,2,4),(5.07026194164673E-5,
0.0664107174211822,0.13266774477438,0.220200530152142,0.288215554286479,
0.361732671442871,0.461175020642267,0.563725534521481,0.639861163673004,
0.713093543625183,0.806814466640702,0.938108630180502,1.03093687917782,
1.10547098421022,1.20304888697946,1.34766113854594,1.44826159687985,1.52662536873,
1.61474326774239,1.73523518064143,1.84340197363434,1.92564309108396,2.00788420853358,
2.11605100152649,2.23654291442556,2.32466081343793,2.40302458528804,2.5036250436219,
2.64823729518831,2.74581519795744,2.82034930298975,2.91317755198693,3.04447171552645,
3.13819263854176,3.21142501849377,3.28756064764512,3.39011116152411,3.48955351072329,
3.56307062787951,3.63108565201366,3.71861843739117,3.78487541402478,3.85123506043089),
 .UNSPECIFIED.);
#2117=B_SPLINE_CURVE_WITH_KNOTS('',3,(#13994,#13995,#13996,#13997,#13998,
#13999,#14000,#14001,#14002,#14003,#14004,#14005,#14006,#14007,#14008,#14009,
#14010,#14011,#14012,#14013,#14014,#14015,#14016,#14017,#14018,#14019,#14020,
#14021,#14022,#14023,#14024,#14025,#14026,#14027,#14028,#14029,#14030,#14031,
#14032,#14033,#14034,#14035,#14036,#14037,#14038,#14039,#14040,#14041,#14042,
#14043,#14044,#14045,#14046,#14047,#14048,#14049,#14050,#14051,#14052,#14053,
#14054,#14055,#14056,#14057,#14058,#14059,#14060,#14061,#14062,#14063,#14064,
#14065,#14066,#14067,#14068,#14069,#14070,#14071,#14072,#14073,#14074,#14075,
#14076,#14077,#14078,#14079),.UNSPECIFIED.,.F.,.F.,(4,2,2,2,2,2,2,2,2,2,
2,2,2,2,2,2,2,2,2,2,2,2,2,2,2,2,2,2,2,2,2,2,2,2,2,2,2,2,2,2,2,2,4),(5.09988073474043E-5,
0.0664106539984153,0.132667616465238,0.220200398061176,0.288215419256946,
0.361732533237061,0.461174878140088,0.563725387588608,0.639861013450696,
0.713093390238879,0.806814309205198,0.938108467072451,1.03093671205917,
1.10547081387137,1.20304871242481,1.34766095774345,1.448261411731,1.52662518019551,
1.61474307540084,1.73523498309413,1.84340177141377,1.92564288531024,2.0078839992067,
2.11605078752635,2.23654269521968,2.324660590425,2.40302435888947,2.50362481287698,
2.64823705819555,2.74581495674892,2.82034905856104,2.91317730354766,3.04447146141472,
3.13819238038091,3.21142475716898,3.28756038303095,3.39011089247928,3.48955323738204,
3.56307035136197,3.63108537255756,3.71861815415326,3.78487517864366,3.85123405850448),
 .UNSPECIFIED.);
#2118=B_SPLINE_CURVE_WITH_KNOTS('',3,(#14222,#14223,#14224,#14225,#14226,
#14227,#14228,#14229,#14230,#14231,#14232,#14233,#14234,#14235,#14236,#14237,
#14238,#14239,#14240,#14241,#14242,#14243,#14244,#14245,#14246,#14247,#14248,
#14249,#14250,#14251,#14252,#14253,#14254,#14255,#14256,#14257,#14258,#14259,
#14260,#14261,#14262,#14263,#14264,#14265,#14266,#14267,#14268,#14269,#14270,
#14271,#14272,#14273,#14274,#14275,#14276,#14277,#14278,#14279,#14280,#14281,
#14282,#14283,#14284,#14285,#14286,#14287,#14288,#14289,#14290,#14291,#14292,
#14293,#14294,#14295,#14296,#14297,#14298,#14299,#14300,#14301,#14302,#14303,
#14304,#14305,#14306,#14307,#14308,#14309,#14310,#14311,#14312,#14313,#14314,
#14315,#14316,#14317,#14318,#14319,#14320,#14321,#14322,#14323,#14324,#14325,
#14326,#14327,#14328,#14329,#14330,#14331,#14332,#14333,#14334,#14335,#14336,
#14337,#14338,#14339,#14340,#14341,#14342,#14343,#14344,#14345,#14346,#14347,
#14348,#14349,#14350,#14351,#14352,#14353,#14354,#14355,#14356,#14357,#14358,
#14359,#14360,#14361,#14362,#14363,#14364,#14365,#14366,#14367,#14368,#14369,
#14370,#14371,#14372,#14373,#14374,#14375,#14376,#14377,#14378,#14379,#14380,
#14381,#14382,#14383,#14384,#14385,#14386,#14387,#14388,#14389,#14390,#14391,
#14392,#14393,#14394,#14395,#14396,#14397,#14398,#14399,#14400,#14401,#14402,
#14403,#14404,#14405,#14406,#14407,#14408,#14409,#14410,#14411,#14412,#14413,
#14414,#14415,#14416,#14417,#14418,#14419,#14420,#14421,#14422,#14423,#14424,
#14425,#14426,#14427,#14428,#14429,#14430,#14431,#14432,#14433,#14434,#14435,
#14436,#14437,#14438,#14439,#14440,#14441,#14442,#14443,#14444,#14445,#14446,
#14447,#14448,#14449,#14450,#14451,#14452,#14453,#14454,#14455,#14456,#14457,
#14458,#14459,#14460,#14461,#14462,#14463,#14464,#14465,#14466,#14467,#14468,
#14469,#14470,#14471,#14472,#14473,#14474,#14475,#14476,#14477,#14478,#14479,
#14480,#14481,#14482,#14483,#14484,#14485,#14486,#14487,#14488,#14489,#14490,
#14491,#14492,#14493,#14494,#14495,#14496,#14497,#14498,#14499,#14500,#14501,
#14502,#14503,#14504,#14505,#14506,#14507,#14508,#14509,#14510,#14511,#14512,
#14513,#14514,#14515,#14516,#14517,#14518,#14519,#14520,#14521,#14522,#14523,
#14524,#14525,#14526,#14527,#14528,#14529,#14530,#14531,#14532,#14533,#14534,
#14535,#14536,#14537,#14538,#14539,#14540,#14541,#14542,#14543,#14544,#14545,
#14546,#14547,#14548,#14549,#14550,#14551,#14552,#14553,#14554,#14555,#14556,
#14557,#14558,#14559,#14560,#14561,#14562,#14563,#14564,#14565,#14566,#14567,
#14568,#14569,#14570,#14571,#14572,#14573,#14574,#14575,#14576,#14577,#14578,
#14579,#14580,#14581,#14582,#14583,#14584,#14585,#14586,#14587,#14588,#14589,
#14590,#14591,#14592,#14593,#14594,#14595,#14596,#14597,#14598,#14599,#14600,
#14601,#14602,#14603,#14604,#14605,#14606,#14607,#14608,#14609,#14610,#14611,
#14612,#14613,#14614,#14615,#14616,#14617,#14618,#14619,#14620,#14621,#14622,
#14623,#14624),.UNSPECIFIED.,.F.,.F.,(4,3,3,3,3,3,3,3,3,3,3,3,3,3,3,3,3,
3,3,3,3,3,3,3,3,3,3,3,3,3,3,3,3,3,3,3,3,3,3,3,3,3,3,3,3,3,3,3,3,3,3,3,3,
3,3,3,3,3,3,3,3,3,3,3,3,3,3,3,3,3,3,3,3,3,3,3,3,3,3,3,3,3,3,3,3,3,3,3,3,
3,3,3,3,3,3,3,3,3,3,3,3,3,3,3,3,3,3,3,3,3,3,3,3,3,3,3,3,3,3,3,3,3,3,3,3,
3,3,3,3,3,3,3,3,3,4),(0.,0.009615384615385,0.0125000395761689,0.01923076923077,
0.02884615384615,0.03846153846154,0.0449999664041082,0.04807692307692,0.05769230769231,
0.06730769230769,0.07692307692308,0.0775000049929539,0.08653846153846,0.09615384615385,
0.1057692307692,0.110000014413493,0.1153846153846,0.125,0.1346153846154,
0.1424999755863,0.1442307692308,0.1538461538462,0.1634615384615,0.1730769230769,
0.175000027234005,0.1826923076923,0.1923076923077,0.2019230769231,0.207499981369673,
0.2115384615385,0.2211538461538,0.2307692307692,0.239999997337637,0.2403846153846,
0.25,0.2596153846154,0.2692307692308,0.272500030849891,0.2788461538462,
0.2884615384615,0.2980769230769,0.304999966725719,0.3076923076923,0.3173076923077,
0.3269230769231,0.3365384615385,0.337500011015578,0.3461538461538,0.3557692307692,
0.3653846153846,0.370000004926624,0.375,0.3846153846154,0.3942307692308,
0.402499982129091,0.4038461538462,0.4134615384615,0.4230769230769,0.4326923076923,
0.435000031453539,0.4423076923077,0.4519230769231,0.4615384615385,0.467499974129879,
0.4711538461538,0.4807692307692,0.4903846153846,0.5,0.5096153846154,0.5192307692308,
0.5288461538462,0.532500025870121,0.5384615384615,0.5480769230769,0.5576923076923,
0.564999968546461,0.5673076923077,0.5769230769231,0.5865384615385,0.5961538461538,
0.597500017870908,0.6057692307692,0.6153846153846,0.625,0.629999995073376,
0.6346153846154,0.6442307692308,0.6538461538462,0.662499988984422,0.6634615384615,
0.6730769230769,0.6826923076923,0.6923076923077,0.695000033274281,0.7019230769231,
0.7115384615385,0.7211538461538,0.727499969150109,0.7307692307692,0.7403846153846,
0.75,0.7596153846154,0.760000002662363,0.7692307692308,0.7788461538462,
0.7884615384615,0.792500018630328,0.7980769230769,0.8076923076923,0.8173076923077,
0.824999972765995,0.8269230769231,0.8365384615385,0.8461538461538,0.8557692307692,
0.8575000244137,0.8653846153846,0.875,0.8846153846154,0.889999985586514,
0.8942307692308,0.9038461538462,0.9134615384615,0.922499995007029,0.9230769230769,
0.9326923076923,0.9423076923077,0.9519230769231,0.955000033595907,0.9615384615385,
0.9711538461538,0.9807692307692,0.987499960423811,0.9903846153846,1.),
 .UNSPECIFIED.);
#2119=B_SPLINE_CURVE_WITH_KNOTS('',3,(#14906,#14907,#14908,#14909,#14910,
#14911,#14912,#14913,#14914,#14915,#14916,#14917,#14918,#14919,#14920,#14921,
#14922,#14923,#14924,#14925,#14926,#14927,#14928,#14929,#14930,#14931,#14932,
#14933,#14934,#14935,#14936,#14937,#14938,#14939,#14940,#14941,#14942,#14943,
#14944,#14945,#14946,#14947,#14948,#14949,#14950,#14951,#14952,#14953,#14954,
#14955,#14956,#14957,#14958,#14959,#14960,#14961,#14962,#14963,#14964,#14965,
#14966,#14967,#14968,#14969,#14970,#14971,#14972,#14973,#14974,#14975,#14976,
#14977,#14978,#14979,#14980,#14981,#14982,#14983,#14984,#14985,#14986,#14987,
#14988,#14989,#14990,#14991,#14992,#14993,#14994,#14995,#14996,#14997,#14998,
#14999,#15000,#15001,#15002,#15003,#15004,#15005,#15006,#15007,#15008,#15009,
#15010,#15011,#15012,#15013,#15014,#15015,#15016,#15017,#15018,#15019,#15020,
#15021,#15022,#15023,#15024,#15025,#15026,#15027,#15028,#15029,#15030,#15031,
#15032,#15033,#15034,#15035,#15036,#15037,#15038,#15039,#15040,#15041,#15042,
#15043,#15044,#15045,#15046,#15047,#15048,#15049,#15050,#15051,#15052,#15053,
#15054,#15055,#15056,#15057,#15058,#15059,#15060,#15061,#15062,#15063,#15064,
#15065,#15066,#15067,#15068,#15069,#15070,#15071,#15072,#15073,#15074,#15075,
#15076,#15077,#15078,#15079,#15080,#15081,#15082,#15083,#15084,#15085,#15086,
#15087,#15088,#15089,#15090,#15091,#15092,#15093,#15094,#15095,#15096,#15097,
#15098,#15099,#15100,#15101,#15102,#15103,#15104,#15105,#15106,#15107,#15108,
#15109,#15110,#15111,#15112,#15113,#15114,#15115,#15116,#15117,#15118,#15119,
#15120,#15121,#15122,#15123,#15124,#15125,#15126,#15127,#15128,#15129,#15130,
#15131,#15132,#15133,#15134,#15135,#15136,#15137,#15138,#15139,#15140,#15141,
#15142,#15143,#15144,#15145,#15146,#15147,#15148,#15149,#15150,#15151,#15152,
#15153,#15154,#15155,#15156,#15157,#15158,#15159,#15160,#15161,#15162,#15163,
#15164,#15165,#15166,#15167,#15168,#15169,#15170,#15171,#15172,#15173,#15174,
#15175,#15176,#15177,#15178,#15179,#15180,#15181,#15182,#15183,#15184,#15185,
#15186,#15187,#15188,#15189,#15190,#15191,#15192,#15193,#15194,#15195,#15196,
#15197,#15198,#15199,#15200,#15201,#15202,#15203,#15204,#15205,#15206,#15207,
#15208,#15209,#15210,#15211,#15212,#15213,#15214,#15215,#15216,#15217,#15218,
#15219,#15220,#15221,#15222,#15223,#15224,#15225,#15226,#15227,#15228,#15229,
#15230,#15231,#15232,#15233,#15234,#15235,#15236,#15237,#15238,#15239,#15240,
#15241,#15242,#15243,#15244,#15245,#15246,#15247,#15248,#15249,#15250,#15251,
#15252,#15253,#15254,#15255,#15256,#15257,#15258,#15259,#15260,#15261,#15262,
#15263,#15264,#15265,#15266,#15267,#15268,#15269,#15270,#15271,#15272,#15273,
#15274,#15275,#15276,#15277,#15278,#15279,#15280,#15281,#15282,#15283,#15284,
#15285,#15286,#15287,#15288,#15289,#15290,#15291,#15292,#15293,#15294,#15295,
#15296,#15297,#15298,#15299,#15300,#15301,#15302,#15303,#15304,#15305,#15306,
#15307,#15308),.UNSPECIFIED.,.F.,.F.,(4,3,3,3,3,3,3,3,3,3,3,3,3,3,3,3,3,
3,3,3,3,3,3,3,3,3,3,3,3,3,3,3,3,3,3,3,3,3,3,3,3,3,3,3,3,3,3,3,3,3,3,3,3,
3,3,3,3,3,3,3,3,3,3,3,3,3,3,3,3,3,3,3,3,3,3,3,3,3,3,3,3,3,3,3,3,3,3,3,3,
3,3,3,3,3,3,3,3,3,3,3,3,3,3,3,3,3,3,3,3,3,3,3,3,3,3,3,3,3,3,3,3,3,3,3,3,
3,3,3,3,3,3,3,3,3,4),(0.,0.009615384615385,0.0125000395761689,0.01923076923077,
0.02884615384615,0.03846153846154,0.0449999664041082,0.04807692307692,0.05769230769231,
0.06730769230769,0.07692307692308,0.0775000049929539,0.08653846153846,0.09615384615385,
0.1057692307692,0.110000014413493,0.1153846153846,0.125,0.1346153846154,
0.1424999755863,0.1442307692308,0.1538461538462,0.1634615384615,0.1730769230769,
0.175000027234005,0.1826923076923,0.1923076923077,0.2019230769231,0.207499981369672,
0.2115384615385,0.2211538461538,0.2307692307692,0.239999997337637,0.2403846153846,
0.25,0.2596153846154,0.2692307692308,0.272500030849891,0.2788461538462,
0.2884615384615,0.2980769230769,0.304999966725719,0.3076923076923,0.3173076923077,
0.3269230769231,0.3365384615385,0.337500011015578,0.3461538461538,0.3557692307692,
0.3653846153846,0.370000004926624,0.375,0.3846153846154,0.3942307692308,
0.402499982129091,0.4038461538462,0.4134615384615,0.4230769230769,0.4326923076923,
0.435000031453539,0.4423076923077,0.4519230769231,0.4615384615385,0.467499974129879,
0.4711538461538,0.4807692307692,0.4903846153846,0.5,0.5096153846154,0.5192307692308,
0.5288461538462,0.532500025870121,0.5384615384615,0.5480769230769,0.5576923076923,
0.564999968546461,0.5673076923077,0.5769230769231,0.5865384615385,0.5961538461538,
0.597500017870908,0.6057692307692,0.6153846153846,0.625,0.629999995073376,
0.6346153846154,0.6442307692308,0.6538461538462,0.662499988984422,0.6634615384615,
0.6730769230769,0.6826923076923,0.6923076923077,0.695000033274281,0.7019230769231,
0.7115384615385,0.7211538461538,0.727499969150109,0.7307692307692,0.7403846153846,
0.75,0.7596153846154,0.760000002662363,0.7692307692308,0.7788461538462,
0.7884615384615,0.792500018630328,0.7980769230769,0.8076923076923,0.8173076923077,
0.824999972765995,0.8269230769231,0.8365384615385,0.8461538461538,0.8557692307692,
0.8575000244137,0.8653846153846,0.875,0.8846153846154,0.889999985586515,
0.8942307692308,0.9038461538462,0.9134615384615,0.922499995007029,0.9230769230769,
0.9326923076923,0.9423076923077,0.9519230769231,0.955000033595907,0.9615384615385,
0.9711538461538,0.9807692307692,0.987499960423811,0.9903846153846,1.),
 .UNSPECIFIED.);
#2120=B_SPLINE_CURVE_WITH_KNOTS('',3,(#15456,#15457,#15458,#15459,#15460,
#15461,#15462,#15463,#15464,#15465,#15466,#15467,#15468,#15469),
 .UNSPECIFIED.,.F.,.F.,(4,2,2,2,2,2,4),(0.,0.0355906395315414,0.0702494491909799,
0.11384356616058,0.162348717043925,0.207260502710314,0.250804429192007),
 .UNSPECIFIED.);
#2121=B_SPLINE_CURVE_WITH_KNOTS('',3,(#15470,#15471,#15472,#15473),
 .UNSPECIFIED.,.F.,.F.,(4,4),(-0.00591028098960205,0.),.UNSPECIFIED.);
#2122=B_SPLINE_CURVE_WITH_KNOTS('',3,(#15476,#15477,#15478,#15479,#15480,
#15481,#15482,#15483,#15484,#15485,#15486,#15487,#15488,#15489,#15490,#15491,
#15492,#15493,#15494,#15495,#15496,#15497,#15498,#15499,#15500,#15501,#15502,
#15503,#15504,#15505,#15506,#15507,#15508,#15509,#15510,#15511,#15512,#15513,
#15514,#15515),.UNSPECIFIED.,.F.,.F.,(4,2,2,2,2,2,2,2,2,2,2,2,2,2,2,2,2,
2,2,4),(2.29225165853828E-5,0.0305122189456786,0.0532101150017384,0.0754571497564381,
0.104584917568519,0.142377147502123,0.162368429143501,0.191693310195574,
0.235517239689987,0.256050511622218,0.273508318076584,0.309278902134493,
0.335525645153663,0.379178507747342,0.40831102858237,0.429059497093713,
0.466876471116825,0.496068764353867,0.519112614876548,0.546227663897249),
 .UNSPECIFIED.);
#2123=B_SPLINE_CURVE_WITH_KNOTS('',3,(#15519,#15520,#15521,#15522,#15523,
#15524),.UNSPECIFIED.,.F.,.F.,(4,2,4),(-0.02824401145014,-0.0141111268813085,
-3.50485731018317E-5),.UNSPECIFIED.);
#2124=B_SPLINE_CURVE_WITH_KNOTS('',3,(#15526,#15527,#15528,#15529,#15530,
#15531),.UNSPECIFIED.,.F.,.F.,(4,2,4),(-0.0168790919016364,-0.00846513155472639,
-5.37848794413334E-5),.UNSPECIFIED.);
#2125=B_SPLINE_CURVE_WITH_KNOTS('',3,(#15532,#15533,#15534,#15535,#15536,
#15537),.UNSPECIFIED.,.F.,.F.,(4,2,4),(-0.000680132893780016,-0.00038988449192367,
-8.31318019695661E-6),.UNSPECIFIED.);
#2126=B_SPLINE_CURVE_WITH_KNOTS('',3,(#15679,#15680,#15681,#15682,#15683,
#15684,#15685,#15686,#15687,#15688,#15689,#15690,#15691,#15692,#15693,#15694,
#15695,#15696,#15697,#15698,#15699,#15700,#15701,#15702,#15703,#15704,#15705,
#15706,#15707,#15708,#15709,#15710,#15711,#15712,#15713,#15714,#15715,#15716,
#15717,#15718,#15719,#15720,#15721,#15722,#15723,#15724,#15725,#15726,#15727,
#15728,#15729,#15730,#15731,#15732,#15733,#15734,#15735,#15736,#15737,#15738,
#15739,#15740,#15741,#15742,#15743,#15744,#15745,#15746,#15747,#15748,#15749,
#15750,#15751,#15752,#15753,#15754,#15755,#15756,#15757,#15758,#15759,#15760,
#15761,#15762,#15763,#15764,#15765,#15766,#15767,#15768,#15769,#15770,#15771,
#15772,#15773,#15774,#15775,#15776,#15777,#15778,#15779,#15780,#15781,#15782,
#15783,#15784,#15785,#15786,#15787,#15788),.UNSPECIFIED.,.F.,.F.,(4,2,2,
2,2,2,2,2,2,2,2,2,2,2,2,2,2,2,2,2,2,2,2,2,2,2,2,2,2,2,2,2,2,2,2,2,2,2,2,
2,2,2,2,2,2,2,2,2,2,2,2,2,2,2,4),(-2.00382109951475,-1.97201129963151,-1.94433184367343,
-1.91464419504192,-1.88574115922005,-1.8514353042413,-1.81215756543003,
-1.76810090312334,-1.73023771802479,-1.69702662693861,-1.66354234713588,
-1.63101628430078,-1.59227967169984,-1.54786154099023,-1.50076256763616,
-1.46248270955476,-1.42893305519558,-1.39502934556627,-1.36214098153558,
-1.32284042358914,-1.27770158583834,-1.22982980708018,-1.19078386840074,
-1.1565906087955,-1.12196725706052,-1.08841938389405,-1.04820281978587,
-1.00193682403998,-0.955670828294093,-0.915454264185968,-0.881906391019558,
-0.847283039284548,-0.813089779679285,-0.774043840999812,-0.726172062241663,
-0.681033224490963,-0.641732666544431,-0.608844302513661,-0.574940592884397,
-0.541390938525295,-0.503111080443882,-0.456012107089795,-0.411593976380191,
-0.372857363779306,-0.340331300944244,-0.306847021141525,-0.27363593005535,
-0.235772744956746,-0.191716082650139,-0.152438343839065,-0.118132488860489,
-0.0892294530387735,-0.0595418044073706,-0.0318622560493046,-5.2727048378802E-5),
 .UNSPECIFIED.);
#2127=B_SPLINE_CURVE_WITH_KNOTS('',3,(#15791,#15792,#15793,#15794,#15795,
#15796,#15797,#15798,#15799,#15800,#15801,#15802,#15803,#15804,#15805,#15806,
#15807,#15808,#15809,#15810,#15811,#15812,#15813,#15814,#15815,#15816,#15817,
#15818,#15819,#15820,#15821,#15822,#15823,#15824,#15825,#15826,#15827,#15828,
#15829,#15830,#15831,#15832,#15833,#15834,#15835,#15836,#15837,#15838,#15839,
#15840,#15841,#15842,#15843,#15844,#15845,#15846,#15847,#15848,#15849,#15850,
#15851,#15852,#15853,#15854,#15855,#15856,#15857,#15858,#15859,#15860,#15861,
#15862,#15863,#15864,#15865,#15866,#15867,#15868,#15869,#15870,#15871,#15872,
#15873,#15874,#15875,#15876,#15877,#15878,#15879,#15880,#15881,#15882,#15883,
#15884,#15885,#15886,#15887,#15888,#15889,#15890,#15891,#15892,#15893,#15894,
#15895,#15896,#15897,#15898,#15899,#15900,#15901,#15902,#15903,#15904,#15905,
#15906,#15907,#15908,#15909,#15910,#15911,#15912,#15913,#15914,#15915,#15916,
#15917,#15918,#15919,#15920),.UNSPECIFIED.,.F.,.F.,(4,2,2,2,2,2,2,2,2,2,
2,2,2,2,2,2,2,2,2,2,2,2,2,2,2,2,2,2,2,2,2,2,2,2,2,2,2,2,2,2,2,2,2,2,2,2,
2,2,2,2,2,2,2,2,2,2,2,2,2,2,2,2,2,2,4),(-1.83625218848691,-1.80296123674716,
-1.77086825671766,-1.74211560059189,-1.71132774506505,-1.68640831841803,
-1.65714693616734,-1.62573150567781,-1.6008288419873,-1.57169238758313,
-1.54043408083162,-1.51554173836869,-1.48641103644225,-1.45515341445188,
-1.43027181930539,-1.40114891263515,-1.36990016990591,-1.34502960035837,
-1.31592204656361,-1.28468995316566,-1.25983025562054,-1.23073475026148,
-1.19951547514314,-1.17466668644213,-1.1455840541214,-1.11437869335724,
-1.08954080030501,-1.06047089597884,-1.02928577264449,-1.00445860133142,
-0.975398493160497,-0.943872179557161,-0.919064909412312,-0.894330101305452,
-0.861223437174857,-0.831260641947789,-0.806445883428347,-0.776752862964708,
-0.74718293112293,-0.722378895769069,-0.69153771031895,-0.661875784697552,
-0.637052233202022,-0.606408673955306,-0.576747969275706,-0.551910624025682,
-0.521194048999722,-0.491511324641091,-0.46665874037071,-0.435933945603862,
-0.406231981669284,-0.381364362589519,-0.350625227764694,-0.320911832012579,
-0.296029475423969,-0.265274334711648,-0.235538639512187,-0.210641308945321,
-0.179751853223789,-0.149928219526715,-0.125011810480556,-0.0947418078748108,
-0.0653387434889213,-0.0333024489493881,-2.53469989805008E-5),
 .UNSPECIFIED.);
#2128=B_SPLINE_CURVE_WITH_KNOTS('',3,(#16062,#16063,#16064,#16065,#16066,
#16067,#16068,#16069,#16070,#16071,#16072,#16073,#16074,#16075,#16076,#16077,
#16078,#16079,#16080,#16081,#16082,#16083,#16084,#16085,#16086,#16087,#16088,
#16089,#16090,#16091,#16092,#16093,#16094,#16095,#16096,#16097,#16098,#16099,
#16100,#16101,#16102,#16103,#16104,#16105,#16106,#16107,#16108,#16109,#16110,
#16111,#16112,#16113,#16114,#16115),.UNSPECIFIED.,.F.,.F.,(4,2,2,2,2,2,
2,2,2,2,2,2,2,2,2,2,2,2,2,2,2,2,2,2,2,2,4),(-0.750965113696085,-0.730368370240615,
-0.71363612769438,-0.694601232270837,-0.678242635614603,-0.66697556480159,
-0.637553682137494,-0.598436505921655,-0.565880747199001,-0.537592228302624,
-0.513432405865943,-0.480425777050235,-0.453424707065712,-0.437641522032812,
-0.41506346284529,-0.392734840588027,-0.340675533275673,-0.299351930108356,
-0.266313368147915,-0.237984909868301,-0.204824868419376,-0.16592819889631,
-0.137532920243293,-0.104590291383952,-0.0681247457833163,-0.0142696103655463,
-3.42971879727152E-5),.UNSPECIFIED.);
#2129=B_SPLINE_CURVE_WITH_KNOTS('',3,(#16118,#16119,#16120,#16121,#16122,
#16123,#16124,#16125,#16126,#16127,#16128,#16129,#16130,#16131,#16132,#16133,
#16134,#16135,#16136,#16137,#16138,#16139,#16140,#16141,#16142,#16143,#16144,
#16145,#16146,#16147,#16148,#16149,#16150,#16151,#16152,#16153,#16154,#16155,
#16156,#16157,#16158,#16159,#16160,#16161,#16162,#16163,#16164,#16165,#16166,
#16167,#16168,#16169,#16170,#16171,#16172,#16173,#16174,#16175,#16176,#16177,
#16178,#16179,#16180,#16181,#16182,#16183,#16184,#16185,#16186,#16187,#16188,
#16189,#16190,#16191,#16192,#16193,#16194,#16195,#16196,#16197,#16198,#16199,
#16200,#16201,#16202,#16203,#16204,#16205,#16206,#16207,#16208,#16209,#16210,
#16211,#16212,#16213,#16214,#16215,#16216,#16217,#16218,#16219,#16220,#16221,
#16222,#16223,#16224,#16225,#16226,#16227),.UNSPECIFIED.,.F.,.F.,(4,2,2,
2,2,2,2,2,2,2,2,2,2,2,2,2,2,2,2,2,2,2,2,2,2,2,2,2,2,2,2,2,2,2,2,2,2,2,2,
2,2,2,2,2,2,2,2,2,2,2,2,2,2,2,4),(5.22888875136238E-5,0.0318621331467355,
0.0595415760152274,0.0892292343844242,0.118132279686624,0.152438145917861,
0.191715897612406,0.235772574369891,0.273635771887746,0.306846873867313,
0.34033116465303,0.372857238156833,0.411593863463561,0.456012008742521,
0.503110997545273,0.541390868182636,0.574940533546252,0.608844254296138,
0.641732629114365,0.681033199951567,0.726172052508122,0.774043846968444,
0.813089798455132,0.847283069275912,0.881906432367515,0.915454316537837,
0.955670893837234,1.00193690475858,1.04820291567993,1.08841949297927,1.12196737714953,
1.15659074024116,1.19078401106196,1.22982996254868,1.27770175700899,1.32284060956542,
1.36214118040271,1.39502955522101,1.42893327597085,1.46248294133439,1.50076281197177,
1.54786180077453,1.59227994605348,1.63101657136015,1.6635426448639,1.69702693564962,
1.73023803762918,1.76810123514708,1.81215791190446,1.8514356635988,1.88574152982984,
1.91464457513187,1.94433223350095,1.97201179093797,2.00382132191843),
 .UNSPECIFIED.);
#2130=B_SPLINE_CURVE_WITH_KNOTS('',3,(#16510,#16511,#16512,#16513,#16514,
#16515,#16516,#16517,#16518,#16519,#16520,#16521,#16522,#16523,#16524,#16525,
#16526,#16527,#16528,#16529,#16530,#16531,#16532,#16533,#16534,#16535,#16536,
#16537,#16538,#16539,#16540,#16541,#16542,#16543,#16544,#16545,#16546,#16547,
#16548,#16549,#16550,#16551,#16552,#16553,#16554,#16555,#16556,#16557,#16558,
#16559,#16560,#16561,#16562,#16563,#16564,#16565,#16566,#16567,#16568,#16569,
#16570,#16571,#16572,#16573,#16574,#16575,#16576,#16577,#16578,#16579,#16580,
#16581,#16582,#16583,#16584,#16585,#16586,#16587,#16588,#16589,#16590,#16591,
#16592,#16593,#16594,#16595,#16596,#16597,#16598,#16599,#16600,#16601,#16602,
#16603,#16604,#16605,#16606,#16607,#16608,#16609,#16610,#16611,#16612,#16613,
#16614,#16615,#16616,#16617,#16618,#16619),.UNSPECIFIED.,.F.,.F.,(4,2,2,
2,2,2,2,2,2,2,2,2,2,2,2,2,2,2,2,2,2,2,2,2,2,2,2,2,2,2,2,2,2,2,2,2,2,2,2,
2,2,2,2,2,2,2,2,2,2,2,2,2,2,2,4),(5.27270482666441E-5,0.0318622560492564,
0.0595418044072771,0.0892294530387053,0.118132488860395,0.152438343838929,
0.191716082650089,0.235772744956499,0.273635930054719,0.306847021140621,
0.340331300943069,0.37285736377788,0.411593976378467,0.456012107087719,
0.503111080441407,0.541390938522476,0.574940592881332,0.608844302510329,
0.641732666540797,0.68103322448698,0.726172062237338,0.774043840995097,
0.813089779674242,0.847283039279203,0.881906391013914,0.91545426418006,
0.955670828287863,1.0019368240334,1.04820281977893,1.08841938388673,1.12196725705288,
1.15659060878759,1.19078386839256,1.22982980707169,1.27770158582945,1.32284042357981,
1.36214098152599,1.39502934555647,1.42893305518547,1.46248270954433,1.50076256762539,
1.54786154097908,1.59227967168835,1.63101628428893,1.66354234712375,1.6970266269262,
1.73023771801211,1.76810090311033,1.81215756541673,1.85143530422787,1.88574115920639,
1.91464419502807,1.94433184365948,1.97201139201748,2.00382091256426),
 .UNSPECIFIED.);
#2131=B_SPLINE_CURVE_WITH_KNOTS('',3,(#16622,#16623,#16624,#16625,#16626,
#16627,#16628,#16629,#16630,#16631,#16632,#16633,#16634,#16635,#16636,#16637,
#16638,#16639,#16640,#16641,#16642,#16643,#16644,#16645,#16646,#16647,#16648,
#16649,#16650,#16651,#16652,#16653,#16654,#16655,#16656,#16657,#16658,#16659,
#16660,#16661,#16662,#16663,#16664,#16665,#16666,#16667,#16668,#16669,#16670,
#16671,#16672,#16673,#16674,#16675,#16676,#16677,#16678,#16679,#16680,#16681,
#16682,#16683,#16684,#16685,#16686,#16687,#16688,#16689,#16690,#16691,#16692,
#16693,#16694,#16695,#16696,#16697,#16698,#16699,#16700,#16701,#16702,#16703,
#16704,#16705,#16706,#16707,#16708,#16709,#16710,#16711,#16712,#16713,#16714,
#16715,#16716,#16717,#16718,#16719,#16720,#16721,#16722,#16723,#16724,#16725,
#16726,#16727,#16728,#16729,#16730,#16731),.UNSPECIFIED.,.F.,.F.,(4,2,2,
2,2,2,2,2,2,2,2,2,2,2,2,2,2,2,2,2,2,2,2,2,2,2,2,2,2,2,2,2,2,2,2,2,2,2,2,
2,2,2,2,2,2,2,2,2,2,2,2,2,2,2,4),(-2.00382091256489,-1.97201139201814,-1.94433184366008,
-1.91464419502864,-1.88574115920694,-1.85143530422839,-1.81215756541722,
-1.76810090311079,-1.73023771801257,-1.69702662692665,-1.6635423471242,
-1.63101628428938,-1.59227967168878,-1.54786154097952,-1.50076256762582,
-1.46248270954475,-1.42893305518588,-1.39502934555687,-1.3621409815264,
-1.3228404235802,-1.27770158582984,-1.22982980707207,-1.19078386839291,
-1.15659060878794,-1.12196725705323,-1.08841938388707,-1.04820281977926,
-1.00193682403371,-0.955670828288167,-0.915454264180356,-0.8819063910142,
-0.847283039279479,-0.813089779674504,-0.774043840995357,-0.726172062237589,
-0.681033224487208,-0.641732666541015,-0.608844302510536,-0.574940592881528,
-0.541390938522659,-0.503111080441583,-0.456012107087879,-0.4115939763786,
-0.372857363778004,-0.340331300943183,-0.306847021140722,-0.273635930054805,
-0.235772744956571,-0.191716082650154,-0.152438343838999,-0.11813248886047,
-0.0892294530387833,-0.0595418044073568,-0.0318622560492987,-5.27270483708445E-5),
 .UNSPECIFIED.);
#2132=B_SPLINE_CURVE_WITH_KNOTS('',3,(#16873,#16874,#16875,#16876,#16877,
#16878,#16879,#16880,#16881,#16882,#16883,#16884,#16885,#16886,#16887,#16888,
#16889,#16890,#16891,#16892,#16893,#16894,#16895,#16896,#16897,#16898,#16899,
#16900,#16901,#16902,#16903,#16904,#16905,#16906,#16907,#16908,#16909,#16910,
#16911,#16912,#16913,#16914,#16915,#16916,#16917,#16918,#16919,#16920,#16921,
#16922,#16923,#16924,#16925,#16926,#16927,#16928,#16929,#16930,#16931,#16932,
#16933,#16934,#16935,#16936,#16937,#16938,#16939,#16940,#16941,#16942,#16943,
#16944,#16945,#16946,#16947,#16948,#16949,#16950,#16951,#16952,#16953,#16954,
#16955,#16956,#16957,#16958,#16959,#16960,#16961,#16962,#16963,#16964,#16965,
#16966,#16967,#16968,#16969,#16970,#16971,#16972,#16973,#16974,#16975,#16976,
#16977,#16978,#16979,#16980,#16981,#16982,#16983,#16984,#16985,#16986,#16987,
#16988,#16989,#16990,#16991,#16992,#16993,#16994,#16995,#16996,#16997,#16998,
#16999,#17000,#17001,#17002),.UNSPECIFIED.,.F.,.F.,(4,2,2,2,2,2,2,2,2,2,
2,2,2,2,2,2,2,2,2,2,2,2,2,2,2,2,2,2,2,2,2,2,2,2,2,2,2,2,2,2,2,2,2,2,2,2,
2,2,2,2,2,2,2,2,2,2,2,2,2,2,2,2,2,2,4),(-1.83561951873259,-1.80235844975814,
-1.77029427716558,-1.74156743012038,-1.71080721051427,-1.68591015214814,
-1.65667503562308,-1.62528780438682,-1.60040749393025,-1.57129719311318,
-1.54006694457515,-1.51519694608158,-1.48609239257846,-1.45486282824274,
-1.43000356741716,-1.40090680214813,-1.36968611497522,-1.34483786969891,
-1.31575644088785,-1.28455297753445,-1.25971557915402,-1.23064592334211,
-1.19949870357013,-1.17467106965797,-1.1455947194486,-1.11507291396498,
-1.09023936697185,-1.06088794575343,-1.02660547905822,-1.00186644644199,
-0.973997323135063,-0.948862180594986,-0.920459596649707,-0.895744960446151,
-0.860670082843373,-0.830239044945616,-0.805393512545119,-0.776808789940427,
-0.747243163128625,-0.722439176252239,-0.691584141646649,-0.66192066238225,
-0.637096800111612,-0.606456628004131,-0.576795951846665,-0.551958393276278,
-0.521240644871582,-0.491557566857789,-0.466704745602487,-0.435979884286414,
-0.406277661599022,-0.381409811250468,-0.35067033454635,-0.320956656424519,
-0.296074066980763,-0.26531865226729,-0.235582680284637,-0.210685117079743,
-0.179795369294768,-0.149971456539647,-0.125054814588245,-0.0947845298923839,
-0.0653811907334665,-0.0333252066690533,-6.53684496053783E-5),
 .UNSPECIFIED.);
#2133=B_SPLINE_CURVE_WITH_KNOTS('',3,(#17145,#17146,#17147,#17148,#17149,
#17150,#17151,#17152,#17153,#17154,#17155,#17156,#17157,#17158,#17159,#17160,
#17161,#17162,#17163,#17164,#17165,#17166,#17167,#17168,#17169,#17170,#17171,
#17172,#17173,#17174,#17175,#17176,#17177,#17178,#17179,#17180,#17181,#17182,
#17183,#17184,#17185,#17186,#17187,#17188,#17189,#17190,#17191,#17192,#17193,
#17194,#17195,#17196,#17197,#17198,#17199,#17200),.UNSPECIFIED.,.F.,.F.,
(4,2,2,2,2,2,2,2,2,2,2,2,2,2,2,2,2,2,2,2,2,2,2,2,2,2,2,4),(-1.0462023949558,
-1.02770916434491,-0.963207867413976,-0.91312002222191,-0.88354318731338,
-0.842015496578868,-0.791686095343267,-0.76026436767404,-0.719495385836737,
-0.668995568553684,-0.638516311726255,-0.597094721113933,-0.54650375020668,
-0.514711112380782,-0.47382163868678,-0.432772015023298,-0.402277229521919,
-0.371443744672249,-0.323513899110614,-0.258717091288244,-0.237510669203495,
-0.206526557725729,-0.166517534835296,-0.138197809313294,-0.104591110020813,
-0.0681236581910849,-0.0142648413735641,-3.42971879826158E-5),
 .UNSPECIFIED.);
#2134=B_SPLINE_CURVE_WITH_KNOTS('',3,(#17343,#17344,#17345,#17346,#17347,
#17348,#17349,#17350,#17351,#17352,#17353,#17354,#17355,#17356,#17357,#17358,
#17359,#17360,#17361,#17362,#17363,#17364,#17365,#17366,#17367,#17368,#17369,
#17370,#17371,#17372,#17373,#17374,#17375,#17376,#17377,#17378,#17379,#17380,
#17381,#17382,#17383,#17384,#17385,#17386,#17387,#17388,#17389,#17390,#17391,
#17392,#17393,#17394,#17395,#17396,#17397,#17398,#17399,#17400,#17401,#17402,
#17403,#17404,#17405,#17406,#17407,#17408,#17409,#17410,#17411,#17412,#17413,
#17414,#17415,#17416,#17417,#17418,#17419,#17420,#17421,#17422,#17423,#17424,
#17425,#17426,#17427,#17428,#17429,#17430,#17431,#17432,#17433,#17434,#17435,
#17436,#17437,#17438,#17439,#17440,#17441,#17442,#17443,#17444,#17445,#17446,
#17447,#17448,#17449,#17450,#17451,#17452,#17453,#17454),.UNSPECIFIED.,
 .F.,.F.,(4,2,2,2,2,2,2,2,2,2,2,2,2,2,2,2,2,2,2,2,2,2,2,2,2,2,2,2,2,2,2,
2,2,2,2,2,2,2,2,2,2,2,2,2,2,2,2,2,2,2,2,2,2,2,2,4),(-1.74231738659323,-1.71272813854196,
-1.68417838271532,-1.65861170299748,-1.63123533686212,-1.60907714051855,
-1.58305810475277,-1.55512370293588,-1.53298041210706,-1.50707246139104,
-1.47927777300709,-1.45714365974848,-1.43124082409921,-1.40344674460942,
-1.38132218779627,-1.35542628363528,-1.32764010052686,-1.3055253475805,
-1.27964309465111,-1.2518718165722,-1.2297667283235,-1.20389514364682,-1.17614465541501,
-1.15404902253465,-1.12818466554023,-1.10070401616129,-1.07861121041395,
-1.05264017735879,-1.02306666941232,-1.0010322038119,-0.975921411019613,
-0.954332580969174,-0.932111573457994,-0.903636393356442,-0.883192092893937,
-0.838253102959002,-0.812582949517684,-0.781618122961311,-0.742546052526065,
-0.695158920459714,-0.657943517604473,-0.607098500578842,-0.569371545127974,
-0.518888680069456,-0.479979748859535,-0.43362258666965,-0.397223341127724,
-0.346657163261735,-0.310296328919488,-0.259971486866278,-0.223517021715003,
-0.173445822844544,-0.136570721100847,-0.086863575551722,-0.0496665678786331,
-6.53688914877267E-5),.UNSPECIFIED.);
#2135=B_SPLINE_CURVE_WITH_KNOTS('',3,(#17456,#17457,#17458,#17459,#17460,
#17461,#17462,#17463,#17464,#17465,#17466,#17467,#17468,#17469,#17470,#17471,
#17472,#17473,#17474,#17475,#17476,#17477,#17478,#17479,#17480,#17481,#17482,
#17483,#17484,#17485,#17486,#17487,#17488,#17489,#17490,#17491,#17492,#17493,
#17494,#17495,#17496,#17497,#17498,#17499,#17500,#17501,#17502,#17503,#17504,
#17505),.UNSPECIFIED.,.F.,.F.,(4,2,2,2,2,2,2,2,2,2,2,2,2,2,2,2,2,2,2,2,
2,2,2,2,4),(-1.15405318984419,-1.13700531982188,-1.07753998041418,-1.03134662925519,
-0.959427083652358,-0.903949051282896,-0.818092854923278,-0.752201951754484,
-0.710444097003286,-0.657297506880136,-0.591014894046436,-0.555925429665672,
-0.521099070865684,-0.46097016602311,-0.376614638147581,-0.324415207912168,
-0.262381146764866,-0.237997672332685,-0.203720015827636,-0.165639244416124,
-0.13727850827765,-0.104604576414893,-0.0681040508243425,-0.0141799990057525,
-3.4421973892809E-5),.UNSPECIFIED.);
#2136=B_SPLINE_CURVE_WITH_KNOTS('',3,(#17508,#17509,#17510,#17511,#17512,
#17513,#17514,#17515,#17516,#17517,#17518,#17519,#17520,#17521,#17522,#17523,
#17524,#17525,#17526,#17527,#17528,#17529,#17530,#17531,#17532,#17533,#17534,
#17535,#17536,#17537,#17538,#17539,#17540,#17541,#17542,#17543,#17544,#17545,
#17546,#17547,#17548,#17549,#17550,#17551,#17552,#17553,#17554,#17555,#17556,
#17557,#17558,#17559,#17560,#17561,#17562,#17563,#17564,#17565,#17566,#17567,
#17568,#17569,#17570,#17571,#17572,#17573,#17574,#17575,#17576,#17577,#17578,
#17579,#17580,#17581,#17582,#17583,#17584,#17585,#17586,#17587,#17588,#17589,
#17590,#17591,#17592,#17593,#17594,#17595,#17596,#17597,#17598,#17599,#17600,
#17601,#17602,#17603,#17604,#17605,#17606,#17607,#17608,#17609,#17610,#17611,
#17612,#17613,#17614,#17615,#17616,#17617),.UNSPECIFIED.,.F.,.F.,(4,2,2,
2,2,2,2,2,2,2,2,2,2,2,2,2,2,2,2,2,2,2,2,2,2,2,2,2,2,2,2,2,2,2,2,2,2,2,2,
2,2,2,2,2,2,2,2,2,2,2,2,2,2,2,4),(5.27270482716431E-5,0.0318622560492676,
0.0595418044073026,0.089229453038713,0.118132488860435,0.152438343839018,
0.191716082650095,0.235772744956718,0.273635930055335,0.306847021141509,
0.340331300944227,0.372857363779289,0.41159397638018,0.456012107089798,
0.503111080443886,0.541390938525302,0.574940592884411,0.608844302513673,
0.641732666544447,0.681033224490987,0.726172062241692,0.774043840999849,
0.813089779679324,0.847283039284585,0.881906391019603,0.915454264186023,
0.955670828294158,1.00193682404004,1.04820281978592,1.08841938389412,1.12196725706059,
1.15659060879558,1.19078386840081,1.22982980708026,1.27770158583843,1.32284042358924,
1.36214098153568,1.39502934556638,1.42893305519569,1.46248270955487,1.50076256763627,
1.54786154099035,1.59227967169997,1.63101628430091,1.66354234713601,1.69702662693874,
1.73023771802493,1.76810090312348,1.81215756543019,1.85143530424147,1.88574115922024,
1.91464419504213,1.94433184367366,1.97201140238705,2.00382079698849),
 .UNSPECIFIED.);
#2137=B_SPLINE_CURVE_WITH_KNOTS('',3,(#17759,#17760,#17761,#17762,#17763,
#17764,#17765,#17766,#17767,#17768,#17769,#17770,#17771,#17772,#17773,#17774,
#17775,#17776,#17777,#17778,#17779,#17780,#17781,#17782,#17783,#17784,#17785,
#17786,#17787,#17788,#17789,#17790,#17791,#17792,#17793,#17794,#17795,#17796,
#17797,#17798,#17799,#17800,#17801,#17802,#17803,#17804,#17805,#17806,#17807,
#17808,#17809,#17810,#17811,#17812,#17813,#17814,#17815,#17816,#17817,#17818,
#17819,#17820,#17821,#17822,#17823,#17824,#17825,#17826,#17827,#17828,#17829,
#17830,#17831,#17832,#17833,#17834,#17835,#17836,#17837,#17838,#17839,#17840,
#17841,#17842,#17843,#17844,#17845,#17846,#17847,#17848,#17849,#17850,#17851,
#17852,#17853,#17854,#17855,#17856,#17857,#17858,#17859,#17860,#17861,#17862,
#17863,#17864,#17865,#17866,#17867,#17868),.UNSPECIFIED.,.F.,.F.,(4,2,2,
2,2,2,2,2,2,2,2,2,2,2,2,2,2,2,2,2,2,2,2,2,2,2,2,2,2,2,2,2,2,2,2,2,2,2,2,
2,2,2,2,2,2,2,2,2,2,2,2,2,2,2,4),(-2.00382122385324,-1.97201169537238,-1.94433214011032,
-1.91464448407403,-1.88574144104314,-1.85143557750779,-1.81215782889982,
-1.76810115560431,-1.73023796106162,-1.69702686169173,-1.66354257353715,
-1.63101650258923,-1.59227988032641,-1.54786173853774,-1.50076275343594,
-1.46248288580652,-1.42893322307924,-1.3950295049935,-1.3621411327595,-1.32284056501037,
-1.27770171600086,-1.22982992530222,-1.19078397688366,-1.1565907087497,
-1.12196734837871,-1.08841946684456,-1.04820289270536,-1.00193688541952,
-0.955670878133678,-0.915454303994412,-0.881906422460213,-0.84728306208925,
-0.813089793955311,-0.774043845536778,-0.72617205483812,-0.681033205828492,
-0.641732638079455,-0.60884426584553,-0.57494054775973,-0.541390885032382,
-0.503111017402976,-0.456012032301171,-0.411593890512498,-0.372857268249625,
-0.340331197301665,-0.306846909147073,-0.273635809777168,-0.235772615234533,
-0.191715941938926,-0.152438193330733,-0.118132329795171,-0.0892292867641046,
-0.0595416307276913,-0.0318621625886586,-5.24944897148018E-5),
 .UNSPECIFIED.);
#2138=B_SPLINE_CURVE_WITH_KNOTS('',3,(#18011,#18012,#18013,#18014,#18015,
#18016,#18017,#18018,#18019,#18020,#18021,#18022,#18023,#18024,#18025,#18026,
#18027,#18028,#18029,#18030,#18031,#18032,#18033,#18034,#18035,#18036,#18037,
#18038,#18039,#18040,#18041,#18042,#18043,#18044,#18045,#18046,#18047,#18048,
#18049,#18050,#18051,#18052,#18053,#18054,#18055,#18056,#18057,#18058,#18059,
#18060,#18061,#18062,#18063,#18064,#18065,#18066,#18067,#18068,#18069,#18070,
#18071,#18072,#18073,#18074,#18075,#18076,#18077,#18078,#18079,#18080,#18081,
#18082,#18083,#18084,#18085,#18086,#18087,#18088,#18089,#18090,#18091,#18092,
#18093,#18094,#18095,#18096,#18097,#18098,#18099,#18100,#18101,#18102,#18103,
#18104,#18105,#18106,#18107,#18108,#18109,#18110,#18111,#18112,#18113,#18114,
#18115,#18116,#18117,#18118,#18119,#18120,#18121,#18122,#18123,#18124,#18125,
#18126,#18127,#18128,#18129,#18130,#18131,#18132,#18133,#18134,#18135,#18136,
#18137,#18138),.UNSPECIFIED.,.F.,.F.,(4,2,2,2,2,2,2,2,2,2,2,2,2,2,2,2,2,
2,2,2,2,2,2,2,2,2,2,2,2,2,2,2,2,2,2,2,2,2,2,2,2,2,2,2,2,2,2,2,2,2,2,2,2,
2,2,2,2,2,2,2,2,2,2,4),(-0.724209442048021,-0.712012419228065,-0.699774873077863,
-0.681616457852927,-0.657341985081789,-0.629929009821504,-0.605852526236518,
-0.588109932419774,-0.574000009703252,-0.567069686309773,-0.552823216848468,
-0.541467982710213,-0.532126067407773,-0.527510625181189,-0.518055019712594,
-0.508582461845211,-0.499343005773517,-0.494751846095525,-0.48537530451312,
-0.475940089247624,-0.46676365554951,-0.462178749472849,-0.452841775748094,
-0.443408651260855,-0.434256693627476,-0.429661699527251,-0.420326774943473,
-0.410864213717641,-0.40170027949673,-0.397080753977129,-0.392376911709479,
-0.383407884051634,-0.378959110293847,-0.36958100457871,-0.364962404238539,
-0.35576581741293,-0.346284065020516,-0.336915288463779,-0.332312667618732,
-0.32310011095919,-0.313621704271534,-0.304228734377309,-0.299627376680961,
-0.290366677380499,-0.280861125252255,-0.271412143331777,-0.266796755617985,
-0.257458230849559,-0.247894532506044,-0.238360581007524,-0.233717042817114,
-0.22427442650142,-0.212771689213361,-0.198340223892403,-0.19133056640038,
-0.177011525952808,-0.15915412450686,-0.135775818155052,-0.124447490718968,
-0.101217094808881,-0.0719670763949736,-0.0361476301246094,-0.0180607317449348,
-0.000136180809809842),.UNSPECIFIED.);
#2139=B_SPLINE_CURVE_WITH_KNOTS('',3,(#18140,#18141,#18142,#18143,#18144,
#18145),.UNSPECIFIED.,.F.,.F.,(4,2,4),(-0.00483247580106661,-0.00242691911098953,
-3.7601910332494E-5),.UNSPECIFIED.);
#2140=B_SPLINE_CURVE_WITH_KNOTS('',3,(#18147,#18148,#18149,#18150,#18151,
#18152),.UNSPECIFIED.,.F.,.F.,(4,2,4),(-0.0275281976707898,-0.0137825502036224,
0.),.UNSPECIFIED.);
#2141=B_SPLINE_CURVE_WITH_KNOTS('',3,(#18153,#18154,#18155,#18156,#18157,
#18158,#18159,#18160,#18161,#18162,#18163,#18164,#18165,#18166,#18167,#18168,
#18169,#18170,#18171,#18172,#18173,#18174,#18175,#18176,#18177,#18178,#18179,
#18180,#18181,#18182,#18183,#18184,#18185,#18186,#18187,#18188,#18189,#18190,
#18191,#18192,#18193,#18194,#18195,#18196,#18197,#18198,#18199,#18200,#18201,
#18202,#18203,#18204,#18205,#18206,#18207,#18208,#18209,#18210,#18211,#18212,
#18213,#18214,#18215,#18216,#18217,#18218,#18219,#18220,#18221,#18222,#18223,
#18224,#18225,#18226,#18227,#18228,#18229,#18230,#18231,#18232,#18233,#18234,
#18235,#18236,#18237,#18238,#18239,#18240,#18241,#18242,#18243,#18244,#18245,
#18246,#18247,#18248,#18249,#18250,#18251,#18252,#18253,#18254,#18255,#18256,
#18257,#18258,#18259,#18260),.UNSPECIFIED.,.F.,.F.,(4,2,2,2,2,2,2,2,2,2,
2,2,2,2,2,2,2,2,2,2,2,2,2,2,2,2,2,2,2,2,2,2,2,2,2,2,2,2,2,2,2,2,2,2,2,2,
2,2,2,2,2,2,2,4),(-1.57864048508544,-1.54446598849513,-1.51282058354209,
-1.45635482471215,-1.38848776585317,-1.34517905219782,-1.29525802411295,
-1.25847858725278,-1.1746608395351,-1.0883691385114,-1.04485089132505,-0.983145009409519,
-0.934695536189604,-0.909958056093548,-0.863794529076489,-0.815460471775503,
-0.772619307001527,-0.754454882157872,-0.734069641642063,-0.713058389711127,
-0.676589030490018,-0.661713978186576,-0.645311909159579,-0.625653759340365,
-0.609503546676276,-0.593095359946264,-0.573586468342252,-0.558552932808393,
-0.526799939615536,-0.511275497870786,-0.479962305397725,-0.455344123339125,
-0.435814495644388,-0.426321102519358,-0.411609772310643,-0.391569769342903,
-0.380083028459815,-0.358611529716761,-0.34905248340869,-0.337758942861699,
-0.327260348971232,-0.302583518122225,-0.286919863682097,-0.273277943945509,
-0.2599164773094,-0.240329742861226,-0.22649402828818,-0.212635850179124,
-0.185447274727583,-0.1507298160219,-0.125935120495647,-0.0766598253180761,
-0.0387520613078884,-5.9346581474212E-5),.UNSPECIFIED.);
#2142=B_SPLINE_CURVE_WITH_KNOTS('',3,(#18403,#18404,#18405,#18406,#18407,
#18408,#18409,#18410,#18411,#18412,#18413,#18414,#18415,#18416),
 .UNSPECIFIED.,.F.,.F.,(4,2,2,2,2,2,4),(-0.129888666319633,-0.110958901973454,
-0.0925929637960144,-0.0673725322659813,-0.0429943158352172,-0.0236944798609603,
-0.000230509019371229),.UNSPECIFIED.);
#2143=B_SPLINE_CURVE_WITH_KNOTS('',3,(#18417,#18418,#18419,#18420,#18421,
#18422,#18423,#18424,#18425,#18426,#18427,#18428,#18429,#18430,#18431,#18432,
#18433,#18434,#18435,#18436,#18437,#18438,#18439,#18440,#18441,#18442,#18443,
#18444,#18445,#18446,#18447,#18448,#18449,#18450,#18451,#18452,#18453,#18454,
#18455,#18456,#18457,#18458,#18459,#18460,#18461,#18462,#18463,#18464,#18465,
#18466,#18467,#18468,#18469,#18470,#18471,#18472,#18473,#18474,#18475,#18476,
#18477,#18478,#18479,#18480,#18481,#18482,#18483,#18484,#18485,#18486,#18487,
#18488,#18489,#18490,#18491,#18492,#18493,#18494,#18495,#18496,#18497,#18498,
#18499,#18500,#18501,#18502,#18503,#18504,#18505,#18506,#18507,#18508,#18509,
#18510,#18511,#18512,#18513,#18514,#18515,#18516,#18517,#18518,#18519,#18520,
#18521,#18522,#18523,#18524,#18525,#18526,#18527,#18528,#18529,#18530,#18531,
#18532,#18533,#18534,#18535,#18536,#18537,#18538,#18539,#18540,#18541,#18542,
#18543,#18544,#18545,#18546,#18547,#18548,#18549,#18550,#18551,#18552,#18553,
#18554,#18555,#18556,#18557,#18558,#18559,#18560),.UNSPECIFIED.,.F.,.F.,
(4,2,2,2,2,2,2,2,2,2,2,2,2,2,2,2,2,2,2,2,2,2,2,2,2,2,2,2,2,2,2,2,2,2,2,
2,2,2,2,2,2,2,2,2,2,2,2,2,2,2,2,2,2,2,2,2,2,2,2,2,2,2,2,2,2,2,2,2,2,2,2,
4),(5.26474022382527E-5,0.0318393369807604,0.0592980128182023,0.0792979431064048,
0.0957672433172796,0.118106620244403,0.138323222401668,0.159239151214813,
0.181746335419478,0.203560881592912,0.214840885573553,0.232910739511272,
0.244852133659171,0.266091583097692,0.28355229855556,0.302089976658252,
0.3294942454828,0.366122471577819,0.415668980781027,0.44123794526359,0.492927603854394,
0.517600256378281,0.568883400921198,0.605742580438842,0.635198909934618,
0.64697236331899,0.661501095163747,0.679780743311896,0.700525486353231,
0.711127765381697,0.725195329375971,0.73194061555702,0.737998800367963,
0.743454178372273,0.749017259543572,0.755225752700343,0.761418999200457,
0.77459256360018,0.795106074764413,0.815670757121667,0.826809833565304,
0.837650332183119,0.858417228122364,0.880166564725393,0.900193699045498,
0.909908247699591,0.919128297180291,0.928151730327303,0.935176718718845,
0.949204304985769,0.955159083922506,0.962270981377388,0.971310099577727,
0.9783604628954,0.985155774681686,0.992653618211583,1.0012163312926,1.01209394806449,
1.0197719145481,1.02746363271032,1.04274408783163,1.06201238916331,1.07561766958023,
1.09557471449015,1.11100247230759,1.11680896979578,1.12470779989893,1.13261955506168,
1.14211456831916,1.1509639127575,1.15980968395025,1.16911313657596),
 .UNSPECIFIED.);
#2144=B_SPLINE_CURVE_WITH_KNOTS('',3,(#18561,#18562,#18563,#18564,#18565,
#18566,#18567,#18568,#18569,#18570,#18571,#18572,#18573,#18574,#18575,#18576,
#18577,#18578),.UNSPECIFIED.,.F.,.F.,(4,2,2,2,2,2,2,2,4),(2.08074705752938E-5,
0.0299251342462279,0.0593388741588997,0.0818316849232177,0.12040051455881,
0.158340949255542,0.182369650545949,0.211471464162904,0.240621100987305),
 .UNSPECIFIED.);
#2145=B_SPLINE_CURVE_WITH_KNOTS('',3,(#18583,#18584,#18585,#18586,#18587,
#18588,#18589,#18590,#18591,#18592,#18593,#18594,#18595,#18596,#18597,#18598,
#18599,#18600,#18601,#18602,#18603,#18604,#18605,#18606,#18607,#18608,#18609,
#18610,#18611,#18612,#18613,#18614,#18615,#18616,#18617,#18618,#18619,#18620,
#18621,#18622,#18623,#18624,#18625,#18626,#18627,#18628,#18629,#18630,#18631,
#18632,#18633,#18634,#18635,#18636,#18637,#18638,#18639,#18640,#18641,#18642,
#18643,#18644,#18645,#18646,#18647,#18648,#18649,#18650,#18651,#18652,#18653,
#18654,#18655,#18656,#18657,#18658,#18659,#18660,#18661,#18662,#18663,#18664,
#18665,#18666,#18667,#18668,#18669,#18670,#18671,#18672,#18673,#18674,#18675,
#18676,#18677,#18678,#18679),.UNSPECIFIED.,.F.,.F.,(4,3,3,3,3,3,3,3,3,3,
3,3,3,3,3,3,3,3,3,3,3,3,3,3,3,3,3,3,3,3,3,3,4),(0.,0.0258201387254787,0.0629152472513321,
0.0875674000511779,0.113912785737008,0.153702165597873,0.188336926200019,
0.224722540734876,0.260495064077292,0.28070605024531,0.322581006932306,
0.358158673070872,0.383171365469391,0.419466953457704,0.445774356425421,
0.469641907940648,0.520771786653062,0.545004609088268,0.57335363416754,
0.607202336040835,0.630053107004349,0.649602042372964,0.691474446019008,
0.724334403640295,0.779068317023684,0.809490011109605,0.830155841963515,
0.866649489803741,0.891096251784872,0.910952203144824,0.944692325772077,
0.978832779385412,0.999625753900943),.UNSPECIFIED.);
#2146=B_SPLINE_CURVE_WITH_KNOTS('',3,(#18680,#18681,#18682,#18683),
 .UNSPECIFIED.,.F.,.F.,(4,4),(0.,0.000550666282709742),.UNSPECIFIED.);
#2147=B_SPLINE_CURVE_WITH_KNOTS('',3,(#19464,#19465,#19466,#19467,#19468,
#19469,#19470,#19471,#19472,#19473),.UNSPECIFIED.,.F.,.F.,(4,2,2,2,4),(-0.780748364966661,
-0.707409389000496,-0.630972271764003,-0.554535154527511,-0.481196178561345),
 .UNSPECIFIED.);
#2148=B_SPLINE_CURVE_WITH_KNOTS('',3,(#19480,#19481,#19482,#19483,#19484,
#19485,#19486,#19487,#19488,#19489,#19490,#19491,#19492,#19493),
 .UNSPECIFIED.,.F.,.F.,(4,2,2,2,2,2,4),(0.798464089801492,0.826141341365589,
0.886335543523062,0.946529745680534,1.00672394783801,1.06691814999548,1.09459540155958),
 .UNSPECIFIED.);
#2149=B_SPLINE_CURVE_WITH_KNOTS('',3,(#19507,#19508,#19509,#19510,#19511,
#19512,#19513,#19514,#19515,#19516,#19517),.UNSPECIFIED.,.F.,.F.,(4,2,3,
2,4),(-0.149776093202627,-0.0764371172364887,0.,0.0764371172364886,0.149776093202627),
 .UNSPECIFIED.);
#2150=B_SPLINE_CURVE_WITH_KNOTS('',3,(#19523,#19524,#19525,#19526,#19527,
#19528,#19529,#19530,#19531,#19532,#19533,#19534,#19535,#19536),
 .UNSPECIFIED.,.F.,.F.,(4,2,2,2,2,2,4),(0.167444259347822,0.195121510911858,
0.255315713069315,0.315509915226771,0.375704117384228,0.435898319541684,
0.463575571105721),.UNSPECIFIED.);
#2151=B_SPLINE_CURVE_WITH_KNOTS('',3,(#19551,#19552,#19553,#19554,#19555,
#19556,#19557,#19558,#19559,#19560),.UNSPECIFIED.,.F.,.F.,(4,2,2,2,4),(-0.780748364966754,
-0.707409389000602,-0.630972271764099,-0.554535154527595,-0.481196178561443),
 .UNSPECIFIED.);
#2152=B_SPLINE_CURVE_WITH_KNOTS('',3,(#19567,#19568,#19569,#19570,#19571,
#19572,#19573,#19574,#19575,#19576,#19577,#19578,#19579,#19580),
 .UNSPECIFIED.,.F.,.F.,(4,2,2,2,2,2,4),(0.798464089801529,0.826141341365567,
0.886335543523037,0.946529745680508,1.00672394783798,1.06691814999545,1.09459540155949),
 .UNSPECIFIED.);
#2153=B_SPLINE_CURVE_WITH_KNOTS('',3,(#19594,#19595,#19596,#19597,#19598,
#19599,#19600,#19601,#19602,#19603),.UNSPECIFIED.,.F.,.F.,(4,2,2,2,4),(-0.780748364966882,
-0.707409389000658,-0.630972271764149,-0.55453515452764,-0.481196178561416),
 .UNSPECIFIED.);
#2154=B_SPLINE_CURVE_WITH_KNOTS('',3,(#19610,#19611,#19612,#19613,#19614,
#19615,#19616,#19617,#19618,#19619,#19620,#19621,#19622,#19623),
 .UNSPECIFIED.,.F.,.F.,(4,2,2,2,2,2,4),(0.798464089801425,0.826141341365486,
0.886335543522949,0.946529745680413,1.00672394783788,1.06691814999534,1.0945954015594),
 .UNSPECIFIED.);
#2155=B_SPLINE_CURVE_WITH_KNOTS('',3,(#19637,#19638,#19639,#19640,#19641,
#19642,#19643,#19644,#19645,#19646),.UNSPECIFIED.,.F.,.F.,(4,2,2,2,4),(-0.780748364966597,
-0.707409389000458,-0.63097227176397,-0.554535154527481,-0.481196178561343),
 .UNSPECIFIED.);
#2156=B_SPLINE_CURVE_WITH_KNOTS('',3,(#19653,#19654,#19655,#19656,#19657,
#19658,#19659,#19660,#19661,#19662,#19663,#19664,#19665,#19666),
 .UNSPECIFIED.,.F.,.F.,(4,2,2,2,2,2,4),(-0.463575571105721,-0.435898319541684,
-0.375704117384228,-0.315509915226771,-0.255315713069315,-0.195121510911858,
-0.167444259347822),.UNSPECIFIED.);
#2157=B_SPLINE_CURVE_WITH_KNOTS('',3,(#19680,#19681,#19682,#19683,#19684,
#19685,#19686,#19687,#19688,#19689),.UNSPECIFIED.,.F.,.F.,(4,2,2,2,4),(-0.780748364966661,
-0.707409389000496,-0.630972271764003,-0.554535154527511,-0.481196178561345),
 .UNSPECIFIED.);
#2158=B_SPLINE_CURVE_WITH_KNOTS('',3,(#19696,#19697,#19698,#19699,#19700,
#19701,#19702,#19703,#19704,#19705,#19706,#19707,#19708,#19709),
 .UNSPECIFIED.,.F.,.F.,(4,2,2,2,2,2,4),(0.798464089801492,0.826141341365589,
0.886335543523062,0.946529745680534,1.00672394783801,1.06691814999548,1.09459540155958),
 .UNSPECIFIED.);
#2159=B_SPLINE_CURVE_WITH_KNOTS('',3,(#19723,#19724,#19725,#19726,#19727,
#19728,#19729,#19730,#19731,#19732),.UNSPECIFIED.,.F.,.F.,(4,2,2,2,4),(-0.780748364966754,
-0.707409389000602,-0.630972271764099,-0.554535154527595,-0.481196178561443),
 .UNSPECIFIED.);
#2160=B_SPLINE_CURVE_WITH_KNOTS('',3,(#19739,#19740,#19741,#19742,#19743,
#19744,#19745,#19746,#19747,#19748,#19749,#19750,#19751,#19752),
 .UNSPECIFIED.,.F.,.F.,(4,2,2,2,2,2,4),(0.798464089801529,0.826141341365567,
0.886335543523037,0.946529745680508,1.00672394783798,1.06691814999545,1.09459540155949),
 .UNSPECIFIED.);
#2161=B_SPLINE_CURVE_WITH_KNOTS('',3,(#19766,#19767,#19768,#19769,#19770,
#19771,#19772,#19773,#19774,#19775),.UNSPECIFIED.,.F.,.F.,(4,2,2,2,4),(-0.780748364966882,
-0.707409389000658,-0.630972271764149,-0.55453515452764,-0.481196178561416),
 .UNSPECIFIED.);
#2162=B_SPLINE_CURVE_WITH_KNOTS('',3,(#19782,#19783,#19784,#19785,#19786,
#19787,#19788,#19789,#19790,#19791,#19792,#19793,#19794,#19795),
 .UNSPECIFIED.,.F.,.F.,(4,2,2,2,2,2,4),(0.798464089801425,0.826141341365486,
0.886335543522949,0.946529745680413,1.00672394783788,1.06691814999534,1.0945954015594),
 .UNSPECIFIED.);
#2163=B_SPLINE_CURVE_WITH_KNOTS('',3,(#19809,#19810,#19811,#19812,#19813,
#19814,#19815,#19816,#19817,#19818),.UNSPECIFIED.,.F.,.F.,(4,2,2,2,4),(-0.780748364966597,
-0.707409389000458,-0.63097227176397,-0.554535154527481,-0.481196178561343),
 .UNSPECIFIED.);
#2164=B_SPLINE_CURVE_WITH_KNOTS('',3,(#19825,#19826,#19827,#19828,#19829,
#19830,#19831,#19832,#19833,#19834,#19835,#19836,#19837,#19838),
 .UNSPECIFIED.,.F.,.F.,(4,2,2,2,2,2,4),(-0.463575571105721,-0.435898319541684,
-0.375704117384228,-0.315509915226771,-0.255315713069315,-0.195121510911858,
-0.167444259347822),.UNSPECIFIED.);
#2165=B_SPLINE_CURVE_WITH_KNOTS('',3,(#19852,#19853,#19854,#19855,#19856,
#19857,#19858,#19859,#19860,#19861),.UNSPECIFIED.,.F.,.F.,(4,2,2,2,4),(-0.780748364966661,
-0.707409389000496,-0.630972271764003,-0.554535154527511,-0.481196178561345),
 .UNSPECIFIED.);
#2166=B_SPLINE_CURVE_WITH_KNOTS('',3,(#19868,#19869,#19870,#19871,#19872,
#19873,#19874,#19875,#19876,#19877,#19878,#19879,#19880,#19881),
 .UNSPECIFIED.,.F.,.F.,(4,2,2,2,2,2,4),(0.798464089801492,0.826141341365589,
0.886335543523062,0.946529745680534,1.00672394783801,1.06691814999548,1.09459540155958),
 .UNSPECIFIED.);
#2167=B_SPLINE_CURVE_WITH_KNOTS('',3,(#19895,#19896,#19897,#19898,#19899,
#19900,#19901,#19902,#19903,#19904),.UNSPECIFIED.,.F.,.F.,(4,2,2,2,4),(-0.780748364966754,
-0.707409389000602,-0.630972271764099,-0.554535154527595,-0.481196178561443),
 .UNSPECIFIED.);
#2168=B_SPLINE_CURVE_WITH_KNOTS('',3,(#19911,#19912,#19913,#19914,#19915,
#19916,#19917,#19918,#19919,#19920,#19921,#19922,#19923,#19924),
 .UNSPECIFIED.,.F.,.F.,(4,2,2,2,2,2,4),(0.798464089801529,0.826141341365567,
0.886335543523037,0.946529745680508,1.00672394783798,1.06691814999545,1.09459540155949),
 .UNSPECIFIED.);
#2169=B_SPLINE_CURVE_WITH_KNOTS('',3,(#19938,#19939,#19940,#19941,#19942,
#19943,#19944,#19945,#19946,#19947),.UNSPECIFIED.,.F.,.F.,(4,2,2,2,4),(-0.780748364966882,
-0.707409389000658,-0.630972271764149,-0.55453515452764,-0.481196178561416),
 .UNSPECIFIED.);
#2170=B_SPLINE_CURVE_WITH_KNOTS('',3,(#19954,#19955,#19956,#19957,#19958,
#19959,#19960,#19961,#19962,#19963,#19964,#19965,#19966,#19967),
 .UNSPECIFIED.,.F.,.F.,(4,2,2,2,2,2,4),(0.798464089801425,0.826141341365486,
0.886335543522949,0.946529745680413,1.00672394783788,1.06691814999534,1.0945954015594),
 .UNSPECIFIED.);
#2171=B_SPLINE_CURVE_WITH_KNOTS('',3,(#19981,#19982,#19983,#19984,#19985,
#19986,#19987,#19988,#19989,#19990),.UNSPECIFIED.,.F.,.F.,(4,2,2,2,4),(-0.780748364966597,
-0.707409389000458,-0.63097227176397,-0.554535154527481,-0.481196178561343),
 .UNSPECIFIED.);
#2172=B_SPLINE_CURVE_WITH_KNOTS('',3,(#19997,#19998,#19999,#20000,#20001,
#20002,#20003,#20004,#20005,#20006,#20007,#20008,#20009,#20010),
 .UNSPECIFIED.,.F.,.F.,(4,2,2,2,2,2,4),(-0.463575571105721,-0.435898319541684,
-0.375704117384228,-0.315509915226771,-0.255315713069315,-0.195121510911858,
-0.167444259347822),.UNSPECIFIED.);
#2173=B_SPLINE_CURVE_WITH_KNOTS('',3,(#20024,#20025,#20026,#20027,#20028,
#20029,#20030,#20031,#20032,#20033),.UNSPECIFIED.,.F.,.F.,(4,2,2,2,4),(-0.780748364966661,
-0.707409389000496,-0.630972271764003,-0.554535154527511,-0.481196178561345),
 .UNSPECIFIED.);
#2174=B_SPLINE_CURVE_WITH_KNOTS('',3,(#20040,#20041,#20042,#20043,#20044,
#20045,#20046,#20047,#20048,#20049,#20050,#20051,#20052,#20053),
 .UNSPECIFIED.,.F.,.F.,(4,2,2,2,2,2,4),(0.798464089801492,0.826141341365589,
0.886335543523062,0.946529745680534,1.00672394783801,1.06691814999548,1.09459540155958),
 .UNSPECIFIED.);
#2175=B_SPLINE_CURVE_WITH_KNOTS('',3,(#20067,#20068,#20069,#20070,#20071,
#20072,#20073,#20074,#20075,#20076),.UNSPECIFIED.,.F.,.F.,(4,2,2,2,4),(-0.780748364966754,
-0.707409389000602,-0.630972271764099,-0.554535154527595,-0.481196178561443),
 .UNSPECIFIED.);
#2176=B_SPLINE_CURVE_WITH_KNOTS('',3,(#20083,#20084,#20085,#20086,#20087,
#20088,#20089,#20090,#20091,#20092,#20093,#20094,#20095,#20096),
 .UNSPECIFIED.,.F.,.F.,(4,2,2,2,2,2,4),(0.798464089801529,0.826141341365567,
0.886335543523037,0.946529745680508,1.00672394783798,1.06691814999545,1.09459540155949),
 .UNSPECIFIED.);
#2177=B_SPLINE_CURVE_WITH_KNOTS('',3,(#20110,#20111,#20112,#20113,#20114,
#20115,#20116,#20117,#20118,#20119,#20120),.UNSPECIFIED.,.F.,.F.,(4,2,3,
2,4),(-0.149776093202667,-0.0764371172364962,0.,0.0764371172364962,0.149776093202667),
 .UNSPECIFIED.);
#2178=B_SPLINE_CURVE_WITH_KNOTS('',3,(#20126,#20127,#20128,#20129,#20130,
#20131,#20132,#20133,#20134,#20135,#20136,#20137,#20138,#20139),
 .UNSPECIFIED.,.F.,.F.,(4,2,2,2,2,2,4),(0.16744425934781,0.195121510911909,
0.255315713069385,0.315509915226861,0.375704117384337,0.435898319541812,
0.463575571105912),.UNSPECIFIED.);
#2179=B_SPLINE_CURVE_WITH_KNOTS('',3,(#20178,#20179,#20180,#20181,#20182,
#20183,#20184,#20185,#20186,#20187,#20188,#20189,#20190,#20191,#20192,#20193,
#20194,#20195,#20196,#20197,#20198,#20199,#20200,#20201,#20202,#20203,#20204,
#20205,#20206,#20207,#20208,#20209,#20210,#20211,#20212,#20213,#20214,#20215,
#20216,#20217,#20218,#20219,#20220,#20221,#20222,#20223),.UNSPECIFIED.,
 .T.,.F.,(4,2,2,2,2,2,2,2,2,2,2,2,2,2,2,2,2,2,2,2,2,2,4),(0.,0.0303279803851074,
0.0648320646553547,0.102562075792128,0.126671294216712,0.141186647288206,
0.154035410358203,0.170137123542524,0.200563378583841,0.234595595843345,
0.269428299352715,0.300434782253784,0.331382982474387,0.368306307376294,
0.405848054427407,0.42449623685392,0.437619477079292,0.451067252290898,
0.470635743932431,0.508603340981971,0.544438969378365,0.563834514230334,
0.582682105035748),.UNSPECIFIED.);
#2180=B_SPLINE_CURVE_WITH_KNOTS('',3,(#20226,#20227,#20228,#20229,#20230,
#20231,#20232,#20233,#20234,#20235,#20236,#20237,#20238,#20239,#20240,#20241,
#20242,#20243,#20244,#20245,#20246,#20247,#20248,#20249,#20250,#20251,#20252,
#20253,#20254),.UNSPECIFIED.,.F.,.F.,(4,2,2,2,2,2,2,3,2,2,2,2,2,4),(0.437146516074455,
0.437619477079327,0.451067252290927,0.470635743932452,0.508603340981988,
0.544438969378375,0.563834514230342,0.582682105035755,0.613010085420863,
0.647514169691112,0.685244180827893,0.709353399252473,0.723868752323962,
0.728371798153077),.UNSPECIFIED.);
#2181=B_SPLINE_CURVE_WITH_KNOTS('',3,(#20255,#20256,#20257,#20258,#20259,
#20260,#20261,#20262,#20263,#20264,#20265,#20266,#20267,#20268,#20269,#20270,
#20271,#20272,#20273,#20274,#20275,#20276,#20277,#20278),.UNSPECIFIED.,
 .F.,.F.,(4,2,2,2,2,2,2,2,2,2,2,4),(0.728371798153077,0.736717515393956,
0.752819228578281,0.783245483619599,0.817277700879103,0.852110404388476,
0.883116887289549,0.914065087510156,0.95098841241207,0.988530159463189,
1.00717834188971,1.01982862111021),.UNSPECIFIED.);
#2182=B_SPLINE_CURVE_WITH_KNOTS('',3,(#20311,#20312,#20313,#20314),
 .UNSPECIFIED.,.F.,.F.,(4,4),(0.,0.00439307035085368),.UNSPECIFIED.);
#2183=B_SPLINE_CURVE_WITH_KNOTS('',3,(#20320,#20321,#20322,#20323,#20324,
#20325,#20326,#20327,#20328,#20329),.UNSPECIFIED.,.F.,.F.,(4,2,2,2,4),(5.13627280805781E-5,
0.0320258340472732,0.0612702767974556,0.0930309669729081,0.134040491070964),
 .UNSPECIFIED.);
#2184=B_SPLINE_CURVE_WITH_KNOTS('',3,(#20331,#20332,#20333,#20334,#20335,
#20336,#20337,#20338,#20339,#20340,#20341,#20342,#20343,#20344,#20345,#20346,
#20347,#20348,#20349,#20350,#20351,#20352,#20353,#20354,#20355,#20356,#20357,
#20358,#20359,#20360,#20361,#20362,#20363,#20364,#20365,#20366,#20367,#20368,
#20369,#20370,#20371,#20372,#20373,#20374,#20375,#20376,#20377,#20378,#20379,
#20380,#20381,#20382),.UNSPECIFIED.,.F.,.F.,(4,3,3,3,3,3,3,3,3,3,3,3,3,
3,3,3,3,4),(0.000145335606066559,0.0558438614877374,0.112231630436153,0.148456034280231,
0.227748495028953,0.282789424752488,0.337741461975064,0.401442660385716,
0.446139981200921,0.53876827776481,0.628638367340173,0.701989458203041,
0.775601617992821,0.816653167456479,0.865359231836614,0.925223109102549,
0.98460838252849,1.),.UNSPECIFIED.);
#2185=B_SPLINE_CURVE_WITH_KNOTS('',3,(#20383,#20384,#20385,#20386,#20387,
#20388,#20389,#20390,#20391,#20392,#20393,#20394,#20395,#20396,#20397,#20398),
 .UNSPECIFIED.,.F.,.F.,(4,2,2,2,2,2,2,4),(0.,0.0366659264051676,0.0723720753432845,
0.124708624882515,0.177690395521786,0.229019615948737,0.276645523150972,
0.335263057882293),.UNSPECIFIED.);
#2186=B_SPLINE_CURVE_WITH_KNOTS('',3,(#20401,#20402,#20403,#20404,#20405,
#20406,#20407,#20408,#20409,#20410,#20411,#20412),.UNSPECIFIED.,.F.,.F.,
(4,2,2,2,2,4),(3.49458439059213E-5,0.0453289864597133,0.0881005201250716,
0.109209349263548,0.131675926651336,0.173631899173032),.UNSPECIFIED.);
#2187=B_SPLINE_CURVE_WITH_KNOTS('',3,(#20555,#20556,#20557,#20558,#20559,
#20560,#20561,#20562,#20563,#20564,#20565,#20566,#20567,#20568,#20569,#20570,
#20571,#20572,#20573,#20574,#20575,#20576,#20577,#20578,#20579,#20580,#20581,
#20582,#20583,#20584,#20585,#20586,#20587,#20588,#20589,#20590,#20591,#20592,
#20593,#20594,#20595,#20596,#20597,#20598,#20599,#20600,#20601,#20602,#20603,
#20604,#20605,#20606,#20607,#20608,#20609,#20610,#20611,#20612,#20613,#20614,
#20615,#20616,#20617,#20618,#20619,#20620,#20621,#20622,#20623,#20624,#20625,
#20626,#20627,#20628,#20629,#20630,#20631,#20632,#20633,#20634,#20635,#20636,
#20637,#20638,#20639,#20640,#20641,#20642,#20643,#20644,#20645,#20646,#20647,
#20648,#20649,#20650,#20651,#20652,#20653,#20654,#20655,#20656,#20657,#20658,
#20659,#20660,#20661,#20662,#20663,#20664,#20665,#20666,#20667,#20668,#20669,
#20670,#20671,#20672,#20673,#20674,#20675,#20676,#20677,#20678,#20679,#20680,
#20681,#20682,#20683,#20684,#20685,#20686,#20687,#20688,#20689,#20690,#20691,
#20692,#20693,#20694,#20695,#20696,#20697,#20698,#20699,#20700,#20701,#20702,
#20703,#20704,#20705,#20706,#20707,#20708,#20709,#20710,#20711,#20712,#20713,
#20714,#20715,#20716,#20717,#20718,#20719,#20720,#20721,#20722,#20723,#20724,
#20725,#20726,#20727,#20728,#20729,#20730,#20731,#20732,#20733,#20734,#20735,
#20736,#20737,#20738,#20739,#20740,#20741,#20742,#20743,#20744,#20745,#20746,
#20747,#20748,#20749,#20750,#20751,#20752,#20753,#20754),.UNSPECIFIED.,
 .F.,.F.,(4,2,2,2,2,2,2,2,2,2,2,2,2,2,2,2,2,2,2,2,2,2,2,2,2,2,2,2,2,2,2,
2,2,2,2,2,2,2,2,2,2,2,2,2,2,2,2,2,2,2,2,2,2,2,2,2,2,2,2,2,2,2,2,2,2,2,2,
2,2,2,2,2,2,2,2,2,2,2,2,2,2,2,2,2,2,2,2,2,2,2,2,2,2,2,2,2,2,2,2,4),(7.45212108627149E-5,
0.0390859205350479,0.0725343883639714,0.0923685642265828,0.10913469384073,
0.129155095331907,0.162486409684089,0.180608217655252,0.197291535945613,
0.206770940019813,0.225188684952061,0.243528078049337,0.256462991620191,
0.264518834073687,0.280147599046037,0.296305916680565,0.308456488246771,
0.318005525489979,0.326611674502013,0.343989855479804,0.352023793262373,
0.368259649578705,0.379849408566588,0.394029573187565,0.407680306645622,
0.424415770043147,0.43678227704562,0.450244531707888,0.463053111242432,
0.477324221391811,0.492271306083695,0.509239387041698,0.517031504020095,
0.539706652015012,0.549548685711017,0.563677913026186,0.572928012382314,
0.589291627420903,0.604168007251376,0.616383894352015,0.627484328862961,
0.655655883221415,0.66902740806289,0.683521944564165,0.715231655167139,
0.748094638169843,0.78081393145294,0.820255058267261,0.86511658506511,0.8872313920142,
0.93278922862096,0.970291556017733,1.01383492275163,1.03578068793651,1.05134433691653,
1.07348802880114,1.09404302061058,1.10953987000782,1.12475427757661,1.1409239918375,
1.16865195202472,1.18227448258818,1.20307890941387,1.22478565953238,1.24693285450956,
1.25844545792802,1.2837125731859,1.29455662461225,1.31868739711981,1.33090099941074,
1.34615816441378,1.36164027989683,1.3801960490241,1.40077714225269,1.42078748038377,
1.44154422431501,1.45889752043253,1.47881011912306,1.48990219432189,1.51418923130129,
1.52701547654404,1.53949488816994,1.55641883911018,1.57834720388455,1.60230105640136,
1.6148609138865,1.63693381184042,1.65424351253927,1.68439231036836,1.69912008127496,
1.71980420571561,1.7480963978574,1.79484207024713,1.82938593412522,1.87669821849617,
1.92347052961058,1.97673507695957,2.02673097417545,2.05162657191679,2.07670782789279),
 .UNSPECIFIED.);
#2188=B_SPLINE_CURVE_WITH_KNOTS('',3,(#20757,#20758,#20759,#20760,#20761,
#20762,#20763,#20764,#20765,#20766,#20767,#20768,#20769,#20770,#20771,#20772,
#20773,#20774,#20775,#20776,#20777,#20778,#20779,#20780,#20781,#20782,#20783,
#20784,#20785,#20786,#20787,#20788,#20789,#20790,#20791,#20792,#20793,#20794,
#20795,#20796,#20797,#20798,#20799,#20800,#20801,#20802,#20803,#20804,#20805,
#20806,#20807,#20808,#20809,#20810,#20811,#20812,#20813,#20814,#20815,#20816,
#20817,#20818,#20819,#20820,#20821,#20822,#20823,#20824,#20825,#20826,#20827,
#20828,#20829,#20830,#20831,#20832,#20833,#20834,#20835,#20836,#20837,#20838,
#20839,#20840,#20841,#20842,#20843,#20844,#20845,#20846,#20847,#20848,#20849,
#20850,#20851,#20852,#20853,#20854,#20855,#20856,#20857,#20858,#20859,#20860,
#20861,#20862,#20863,#20864,#20865,#20866,#20867,#20868,#20869,#20870,#20871,
#20872,#20873,#20874),.UNSPECIFIED.,.F.,.F.,(4,2,2,2,2,2,2,2,2,2,2,2,2,
2,2,2,2,2,2,2,2,2,2,2,2,2,2,2,2,2,2,2,2,2,2,2,2,2,2,2,2,2,2,2,2,2,2,2,2,
2,2,2,2,2,2,2,2,2,4),(-1.76933842521691,-1.75674576879776,-1.74490053734257,
-1.73208561542255,-1.72272120633228,-1.70518992653856,-1.69490789137764,
-1.67805988019643,-1.66693268245685,-1.65308325501219,-1.64232441419012,
-1.62057361832964,-1.59364721685683,-1.56003185692642,-1.54329842415155,
-1.52594121987271,-1.49668326282551,-1.46639000558743,-1.44829465608857,
-1.43030111448265,-1.40351884475363,-1.3794702173695,-1.347081159001,-1.33381533931789,
-1.31924278076883,-1.30492051384824,-1.28667377582415,-1.25919462303656,
-1.23249275230696,-1.20410316074078,-1.16947353335439,-1.12643013051659,
-1.10551542910693,-1.06375425104976,-1.02128477547816,-0.980831861829275,
-0.957773368677078,-0.933456655940948,-0.916552189219702,-0.886703502045147,
-0.838519038842251,-0.816226780787853,-0.779667415609276,-0.750538622619109,
-0.722803539353438,-0.684732734627719,-0.63056648173689,-0.582545875778306,
-0.526120615833343,-0.469754166438239,-0.405799756718641,-0.366097308625937,
-0.288199258420126,-0.212956502445796,-0.174214028651596,-0.130497935980871,
-0.0721693074289823,-0.0379539402192462,-3.50852568431468E-5),
 .UNSPECIFIED.);
#2189=B_SPLINE_CURVE_WITH_KNOTS('',3,(#21015,#21016,#21017,#21018,#21019,
#21020),.UNSPECIFIED.,.F.,.F.,(4,2,4),(-0.0184844970402346,-0.00927720086146568,
0.),.UNSPECIFIED.);
#2190=B_SPLINE_CURVE_WITH_KNOTS('',3,(#21022,#21023,#21024,#21025,#21026,
#21027,#21028,#21029,#21030,#21031,#21032,#21033,#21034,#21035,#21036,#21037,
#21038,#21039,#21040,#21041,#21042,#21043,#21044,#21045,#21046,#21047,#21048,
#21049,#21050,#21051,#21052,#21053,#21054,#21055,#21056,#21057,#21058,#21059,
#21060,#21061,#21062,#21063,#21064,#21065,#21066,#21067,#21068,#21069,#21070,
#21071,#21072,#21073),.UNSPECIFIED.,.F.,.F.,(4,2,2,2,2,2,2,2,2,2,2,2,2,
2,2,2,2,2,2,2,2,2,2,2,2,4),(-1.09405986636961,-1.03730632127397,-0.984374802569,
-0.948133535627927,-0.91402589190069,-0.850789144110965,-0.814114574656998,
-0.780501482328998,-0.716513557400044,-0.679267127882597,-0.643435469696746,
-0.583663696479992,-0.54471419772387,-0.506138779451838,-0.461835275143851,
-0.39250853791068,-0.355884669271099,-0.316987624288024,-0.259015545363003,
-0.231144290960428,-0.199057203738863,-0.150397488973068,-0.120980335034911,
-0.0899477105086688,-0.0466030340969419,-5.56419646036315E-5),
 .UNSPECIFIED.);
#2191=B_SPLINE_CURVE_WITH_KNOTS('',3,(#21076,#21077,#21078,#21079,#21080,
#21081,#21082,#21083,#21084,#21085,#21086,#21087,#21088,#21089,#21090,#21091,
#21092,#21093,#21094,#21095,#21096,#21097,#21098,#21099,#21100,#21101,#21102,
#21103,#21104,#21105,#21106,#21107,#21108,#21109,#21110,#21111,#21112,#21113,
#21114,#21115,#21116,#21117,#21118,#21119,#21120,#21121,#21122,#21123,#21124,
#21125,#21126,#21127,#21128,#21129,#21130,#21131,#21132,#21133,#21134,#21135,
#21136,#21137,#21138,#21139,#21140,#21141,#21142,#21143,#21144,#21145,#21146,
#21147,#21148,#21149,#21150,#21151,#21152,#21153,#21154,#21155,#21156,#21157,
#21158,#21159,#21160,#21161,#21162,#21163,#21164,#21165,#21166,#21167,#21168,
#21169,#21170,#21171,#21172,#21173,#21174,#21175,#21176,#21177,#21178,#21179,
#21180,#21181,#21182,#21183,#21184,#21185,#21186,#21187,#21188,#21189,#21190,
#21191,#21192,#21193,#21194,#21195,#21196,#21197,#21198,#21199,#21200,#21201,
#21202,#21203,#21204,#21205,#21206,#21207,#21208,#21209,#21210,#21211,#21212,
#21213,#21214,#21215,#21216,#21217,#21218,#21219,#21220,#21221,#21222,#21223,
#21224,#21225,#21226,#21227,#21228,#21229,#21230,#21231,#21232,#21233,#21234,
#21235,#21236,#21237,#21238,#21239,#21240,#21241,#21242,#21243,#21244,#21245,
#21246,#21247,#21248,#21249,#21250,#21251,#21252,#21253,#21254,#21255,#21256,
#21257,#21258,#21259,#21260,#21261,#21262,#21263,#21264,#21265,#21266,#21267,
#21268,#21269,#21270,#21271,#21272,#21273,#21274,#21275,#21276,#21277,#21278,
#21279,#21280,#21281,#21282,#21283,#21284,#21285,#21286,#21287,#21288,#21289,
#21290,#21291,#21292,#21293,#21294,#21295,#21296,#21297,#21298,#21299,#21300,
#21301,#21302,#21303,#21304,#21305,#21306,#21307,#21308,#21309,#21310,#21311,
#21312,#21313,#21314,#21315,#21316,#21317,#21318,#21319,#21320,#21321,#21322,
#21323,#21324,#21325,#21326,#21327,#21328,#21329),.UNSPECIFIED.,.F.,.F.,
(4,2,2,2,2,2,2,2,2,2,2,2,2,2,2,2,2,2,2,2,2,2,2,2,2,2,2,2,2,2,2,2,2,2,2,
2,2,2,2,2,2,2,2,2,2,2,2,2,2,2,2,2,2,2,2,2,2,2,2,2,2,2,2,2,2,2,2,2,2,2,2,
2,2,2,2,2,2,2,2,2,2,2,2,2,2,2,2,2,2,2,2,2,2,2,2,2,2,2,2,2,2,2,2,2,2,2,2,
2,2,2,2,2,2,2,2,2,2,2,2,2,2,2,2,2,2,2,4),(-2.31862914046342,-2.30598459560142,
-2.29322331448155,-2.26919964602539,-2.23871046157128,-2.20609463722988,
-2.17715977999077,-2.14857178018608,-2.12800173401574,-2.10976412741253,
-2.09678253199906,-2.06436414565108,-2.05021195659004,-2.03710558827847,
-2.02490475911032,-2.01275974712957,-1.98702230972913,-1.97538681221731,
-1.95227026199713,-1.94055624090361,-1.91498597580451,-1.90307437360638,
-1.89286574714465,-1.87531068965113,-1.86433811381829,-1.85060718835371,
-1.83345320402823,-1.82220775146935,-1.80786671595337,-1.79551979175111,
-1.78621940477618,-1.77205815369256,-1.75736766324443,-1.74722923140104,
-1.73487864132895,-1.72037909406407,-1.71062825530799,-1.69720351050645,
-1.68276010187228,-1.6728467018132,-1.65468232035854,-1.64247978973589,
-1.63324908992537,-1.61865169207853,-1.60287432863603,-1.59272290269745,
-1.57124401799536,-1.55901554706166,-1.53874326856615,-1.52983643237255,
-1.51914916776934,-1.49583562913336,-1.48234772897258,-1.46493554956798,
-1.45513129319181,-1.44234818132605,-1.41884037090298,-1.40791211922436,
-1.39089691669365,-1.37873487026916,-1.34705513798498,-1.33325150317816,
-1.31752727667309,-1.29910947364165,-1.26674177398155,-1.24752045398081,
-1.23764981543001,-1.20676151180157,-1.18595570121478,-1.14928178402936,
-1.10487254736548,-1.05929884339584,-1.01376099768513,-0.991553150184975,
-0.94723622571489,-0.901647859959443,-0.863968021765192,-0.823058375200254,
-0.802486538092744,-0.766643131386914,-0.750637145057582,-0.73409787754341,
-0.714972538383972,-0.687593860600446,-0.674119836891209,-0.65541070815958,
-0.642501778422718,-0.616363274107068,-0.602275722486382,-0.591795878439827,
-0.571857089189573,-0.554787342092337,-0.523577187953407,-0.507577460823363,
-0.488587404355769,-0.475906376724585,-0.457344106224095,-0.441767668728689,
-0.429619159785518,-0.409110064596727,-0.398911849538941,-0.388838821593165,
-0.366526384232034,-0.355541293851422,-0.337324434191078,-0.31779737053968,
-0.306781814244162,-0.290837862688885,-0.276447811819492,-0.264989855802201,
-0.24860774289435,-0.233365138216303,-0.223005678297635,-0.208979820090255,
-0.193064202825831,-0.180273554774194,-0.16105706518809,-0.147432461814324,
-0.136032304756679,-0.117900485873948,-0.106267693488742,-0.0858274261946478,
-0.0626305750766336,-0.0507041395934779,-0.0300644165754477,-0.0158174060505365,
-5.54591562635499E-5),.UNSPECIFIED.);
#2192=B_SPLINE_CURVE_WITH_KNOTS('',3,(#21614,#21615,#21616,#21617,#21618,
#21619,#21620,#21621,#21622,#21623,#21624,#21625,#21626,#21627,#21628,#21629,
#21630,#21631,#21632,#21633,#21634,#21635,#21636,#21637,#21638,#21639,#21640,
#21641,#21642,#21643,#21644,#21645,#21646,#21647,#21648,#21649,#21650,#21651,
#21652,#21653,#21654,#21655,#21656,#21657,#21658,#21659,#21660,#21661,#21662,
#21663,#21664,#21665,#21666,#21667,#21668,#21669,#21670,#21671,#21672,#21673,
#21674,#21675,#21676,#21677,#21678,#21679,#21680,#21681,#21682,#21683,#21684,
#21685,#21686,#21687,#21688,#21689,#21690,#21691,#21692,#21693,#21694,#21695,
#21696,#21697,#21698,#21699,#21700,#21701,#21702,#21703,#21704,#21705,#21706,
#21707,#21708,#21709,#21710,#21711,#21712,#21713,#21714,#21715,#21716,#21717,
#21718,#21719,#21720,#21721,#21722,#21723,#21724,#21725,#21726,#21727,#21728,
#21729,#21730,#21731,#21732,#21733,#21734,#21735),.UNSPECIFIED.,.F.,.F.,
(4,2,2,2,2,2,2,2,2,2,2,2,2,2,2,2,2,2,2,2,2,2,2,2,2,2,2,2,2,2,2,2,2,2,2,
2,2,2,2,2,2,2,2,2,2,2,2,2,2,2,2,2,2,2,2,2,2,2,2,2,4),(8.30537880068429E-5,
0.0254958373655499,0.0511669758667031,0.0975715295513944,0.144549119666171,
0.190555985985661,0.237173157637105,0.28220739695801,0.33535113383606,0.396327999244979,
0.470573317964654,0.557317906359429,0.662806278007236,0.782445093948236,
0.910467302271474,1.00941636377096,1.09790968723056,1.1703108289258,1.23501882107797,
1.3004731712299,1.36686574863236,1.43393918358028,1.4996857682952,1.56559133213915,
1.62879053162939,1.703133303482,1.788306343389,1.89158296556634,2.0119211065547,
2.17079601025095,2.38272456897449,2.59465312769801,2.75352803139522,2.87386617238471,
2.97714279456311,3.06231583447097,3.13665860632426,3.19985780581505,3.2657633696595,
3.33150995437481,3.39858338932318,3.46497596672612,3.53043031687846,3.59513830903091,
3.66753945072645,3.75603277418654,3.85498183568668,3.98300404401062,4.10264285995221,
4.20813123160079,4.29487581999634,4.36912113871677,4.4300980041263,4.48324174100491,
4.52827598032626,4.57489315197818,4.62090001829821,4.6678776084135,4.71428216209869,
4.73994899132534,4.76536580002195),.UNSPECIFIED.);
#2193=B_SPLINE_CURVE_WITH_KNOTS('',3,(#21736,#21737,#21738,#21739,#21740,
#21741,#21742,#21743,#21744,#21745,#21746,#21747,#21748,#21749,#21750,#21751,
#21752,#21753,#21754,#21755,#21756,#21757,#21758,#21759,#21760,#21761,#21762,
#21763,#21764,#21765,#21766,#21767,#21768,#21769,#21770,#21771,#21772,#21773,
#21774,#21775,#21776,#21777,#21778,#21779,#21780,#21781,#21782,#21783,#21784,
#21785,#21786,#21787,#21788,#21789,#21790,#21791,#21792,#21793,#21794,#21795,
#21796,#21797,#21798,#21799,#21800,#21801,#21802,#21803,#21804,#21805,#21806,
#21807,#21808,#21809,#21810,#21811,#21812,#21813,#21814,#21815,#21816,#21817,
#21818,#21819,#21820,#21821,#21822,#21823,#21824,#21825,#21826,#21827,#21828,
#21829,#21830,#21831,#21832,#21833,#21834,#21835,#21836,#21837,#21838,#21839,
#21840,#21841,#21842,#21843,#21844,#21845,#21846,#21847,#21848,#21849,#21850,
#21851,#21852,#21853,#21854,#21855,#21856,#21857),.UNSPECIFIED.,.F.,.F.,
(4,2,2,2,2,2,2,2,2,2,2,2,2,2,2,2,2,2,2,2,2,2,2,2,2,2,2,2,2,2,2,2,2,2,2,
2,2,2,2,2,2,2,2,2,2,2,2,2,2,2,2,2,2,2,2,2,2,2,2,2,4),(-4.76536595170222,
-4.73995314110334,-4.71428195744723,-4.66787732213782,-4.62089964939037,
-4.57489270214569,-4.52827544849554,-4.48324112996028,-4.43009729960343,
-4.36912032693738,-4.29487487762162,-4.20813013664478,-4.10264157944498,
-3.98300255306166,-3.85498011954989,-3.75603088400096,-3.66753740488334,
-3.59513613583592,-3.53042802986368,-3.46497356457885,-3.39858087039315,
-3.33150731746439,-3.26576061710252,-3.19985493733199,-3.13665562667562,
-3.06231272405554,-2.97713953433084,-2.87386273049197,-2.75352437783121,
-2.59464919467714,-2.38272026317545,-2.17079133167378,-2.0119161485187,
-1.89157779585674,-1.78830099201675,-1.70312780229116,-1.62878489967036,
-1.5655855890134,-1.49967990924233,-1.43393320888005,-1.3668596559508,-1.3004669617646,
-1.23501249647932,-1.17030439050675,-1.09790312145899,-1.00940964234083,
-0.910460406791192,-0.782437973278634,-0.662798946894652,-0.55731038969403,
-0.470565648716402,-0.396320199399856,-0.335343226733173,-0.282199396375739,
-0.237165077840018,-0.190547824189379,-0.144540876944152,-0.097563204196169,
-0.0511585688862554,-0.0254916578336772,-7.48059887998284E-5),
 .UNSPECIFIED.);
#2194=B_SPLINE_CURVE_WITH_KNOTS('',3,(#22001,#22002,#22003,#22004,#22005,
#22006,#22007,#22008,#22009,#22010,#22011,#22012,#22013,#22014,#22015,#22016,
#22017,#22018,#22019,#22020,#22021,#22022,#22023,#22024,#22025,#22026,#22027,
#22028,#22029,#22030,#22031,#22032,#22033,#22034,#22035,#22036,#22037,#22038,
#22039,#22040,#22041,#22042,#22043,#22044,#22045,#22046,#22047,#22048,#22049,
#22050,#22051,#22052,#22053,#22054,#22055,#22056,#22057,#22058,#22059,#22060,
#22061,#22062,#22063,#22064,#22065,#22066,#22067,#22068,#22069,#22070,#22071,
#22072,#22073,#22074,#22075,#22076,#22077,#22078,#22079,#22080,#22081,#22082,
#22083,#22084,#22085,#22086,#22087,#22088,#22089,#22090,#22091,#22092,#22093,
#22094,#22095,#22096,#22097,#22098,#22099,#22100,#22101,#22102,#22103,#22104,
#22105,#22106,#22107,#22108,#22109,#22110,#22111,#22112,#22113,#22114,#22115,
#22116,#22117,#22118,#22119,#22120,#22121,#22122),.UNSPECIFIED.,.F.,.F.,
(4,2,2,2,2,2,2,2,2,2,2,2,2,2,2,2,2,2,2,2,2,2,2,2,2,2,2,2,2,2,2,2,2,2,2,
2,2,2,2,2,2,2,2,2,2,2,2,2,2,2,2,2,2,2,2,2,2,2,2,2,4),(8.30537880068975E-5,
0.025495837365562,0.0511669758667308,0.0975715295513951,0.144549119666162,
0.190555985985693,0.237173157637078,0.282207396957804,0.33535113383566,
0.396327999244494,0.470573317964095,0.557317906358615,0.662806278005663,
0.782445093944814,0.910467302266539,1.00941636376502,1.09790968722332,1.17031082891732,
1.23501882106856,1.30047317121971,1.36686574862139,1.43393918356847,1.49968576828256,
1.56559133212574,1.62879053161532,1.70313330346716,1.78830634337317,1.89158296554934,
2.01192110653645,2.17079601023056,2.38272456894982,2.59465312766908,2.75352803136314,
2.8738661723502,2.97714279452633,3.0623158344323,3.1366586062841,3.19985780577366,
3.26576336961681,3.33150995433086,3.39858338927791,3.46497596667956,3.53043031683068,
3.59513830898189,3.66753945067584,3.75603277413411,3.85498183563256,3.98300404395421,
4.10264285989329,4.20813123154037,4.29487581993493,4.36912113865456,4.43009800406343,
4.48324174094132,4.52827598026207,4.57489315191348,4.62090001823304,4.66787760834784,
4.71428216203254,4.73995330053361,4.76536606643197),.UNSPECIFIED.);
#2195=B_SPLINE_CURVE_WITH_KNOTS('',3,(#22123,#22124,#22125,#22126,#22127,
#22128,#22129,#22130,#22131,#22132,#22133,#22134,#22135,#22136,#22137,#22138,
#22139,#22140,#22141,#22142,#22143,#22144,#22145,#22146,#22147,#22148,#22149,
#22150,#22151,#22152,#22153,#22154,#22155,#22156,#22157,#22158,#22159,#22160,
#22161,#22162,#22163,#22164,#22165,#22166,#22167,#22168,#22169,#22170,#22171,
#22172,#22173,#22174,#22175,#22176,#22177,#22178,#22179,#22180,#22181,#22182,
#22183,#22184,#22185,#22186,#22187,#22188,#22189,#22190,#22191,#22192,#22193,
#22194,#22195,#22196,#22197,#22198,#22199,#22200,#22201,#22202,#22203,#22204,
#22205,#22206,#22207,#22208,#22209,#22210,#22211,#22212,#22213,#22214,#22215,
#22216,#22217,#22218,#22219,#22220,#22221,#22222,#22223,#22224,#22225,#22226,
#22227,#22228,#22229,#22230,#22231,#22232,#22233,#22234,#22235,#22236,#22237,
#22238,#22239,#22240,#22241,#22242,#22243,#22244),.UNSPECIFIED.,.F.,.F.,
(4,2,2,2,2,2,2,2,2,2,2,2,2,2,2,2,2,2,2,2,2,2,2,2,2,2,2,2,2,2,2,2,2,2,2,
2,2,2,2,2,2,2,2,2,2,2,2,2,2,2,2,2,2,2,2,2,2,2,2,2,4),(-4.76536606643129,
-4.73995330053298,-4.71428216203189,-4.66787760834723,-4.62090001823246,
-4.57489315191293,-4.52827598026155,-4.48324174094082,-4.43009800406296,
-4.36912113865412,-4.29487581993452,-4.20813123154001,-4.10264285989297,
-3.98300404395383,-3.85498183563211,-3.75603277413363,-3.66753945067534,
-3.59513830898134,-3.53043031683011,-3.46497596667895,-3.39858338927727,
-3.33150995433019,-3.26576336961609,-3.19985780577291,-3.13665860628333,
-3.06231583443149,-2.97714279452547,-2.8738661723493,-2.75352803136218,
-2.59465312766806,-2.38272456894879,-2.17079601022952,-2.01192110653546,
-1.89158296554841,-1.78830634337229,-1.70313330346632,-1.62879053161452,
-1.56559133212497,-1.49968576828183,-1.43393918356779,-1.36686574862076,
-1.30047317121913,-1.23501882106803,-1.17031082891684,-1.09790968722292,
-1.00941636376468,-0.910467302266278,-0.782445093944685,-0.662806278005648,
-0.557317906358621,-0.470573317964106,-0.396327999244519,-0.33535113383569,
-0.282207396957838,-0.237173157637114,-0.190555985985732,-0.144549119666206,
-0.0975715295514422,-0.05116697586678,-0.0254958373655863,-8.30537880621146E-5),
 .UNSPECIFIED.);
#2196=B_SPLINE_CURVE_WITH_KNOTS('',3,(#22388,#22389,#22390,#22391,#22392,
#22393,#22394,#22395,#22396,#22397,#22398,#22399,#22400,#22401,#22402,#22403,
#22404,#22405,#22406,#22407,#22408,#22409,#22410,#22411,#22412,#22413,#22414,
#22415,#22416,#22417,#22418,#22419,#22420,#22421,#22422,#22423,#22424,#22425,
#22426,#22427,#22428,#22429,#22430,#22431,#22432,#22433,#22434,#22435,#22436,
#22437,#22438,#22439,#22440,#22441,#22442,#22443,#22444,#22445,#22446,#22447,
#22448,#22449,#22450,#22451,#22452,#22453,#22454,#22455,#22456,#22457,#22458,
#22459,#22460,#22461,#22462,#22463,#22464,#22465,#22466,#22467,#22468,#22469,
#22470,#22471,#22472,#22473,#22474,#22475,#22476,#22477,#22478,#22479,#22480,
#22481,#22482,#22483,#22484,#22485,#22486,#22487,#22488,#22489,#22490,#22491,
#22492,#22493,#22494,#22495,#22496,#22497,#22498,#22499,#22500,#22501,#22502,
#22503,#22504,#22505,#22506,#22507,#22508,#22509),.UNSPECIFIED.,.F.,.F.,
(4,2,2,2,2,2,2,2,2,2,2,2,2,2,2,2,2,2,2,2,2,2,2,2,2,2,2,2,2,2,2,2,2,2,2,
2,2,2,2,2,2,2,2,2,2,2,2,2,2,2,2,2,2,2,2,2,2,2,2,2,4),(8.30537880269274E-5,
0.0254958373655947,0.0511669758667937,0.0975715295514548,0.14454911966622,
0.190555985985725,0.237173157637119,0.28220739695796,0.335351133835972,
0.396327999244821,0.470573317964426,0.557317906358994,0.662806278006377,
0.782445093946579,0.910467302269029,1.00941636376802,1.09790968722708,1.17031082892178,
1.23501882107348,1.30047317122506,1.36686574862723,1.43393918357483,1.49968576828938,
1.56559133213308,1.62879053162317,1.70313330347564,1.78830634338255,1.89158296555981,
2.01192110654796,2.17079601024335,2.38272456896422,2.59465312768512,2.75352803137944,
2.87386617236633,2.97714279454242,3.06231583444839,3.1366586063001,3.19985780578957,
3.26576336963271,3.33150995434681,3.3985833892939,3.46497596669554,3.53043031684666,
3.59513830899801,3.66753945069234,3.75603277415084,3.85498183564909,3.9830040439707,
4.1026428599102,4.20813123155683,4.29487581995069,4.36912113866951,4.43009800407772,
4.48324174095536,4.52827598027589,4.57489315192683,4.62090001824586,4.66787760836021,
4.71428216204449,4.73995330054531,4.76536606644342),.UNSPECIFIED.);
#2197=B_SPLINE_CURVE_WITH_KNOTS('',3,(#22510,#22511,#22512,#22513,#22514,
#22515,#22516,#22517,#22518,#22519,#22520,#22521,#22522,#22523,#22524,#22525,
#22526,#22527,#22528,#22529,#22530,#22531,#22532,#22533,#22534,#22535,#22536,
#22537,#22538,#22539,#22540,#22541,#22542,#22543,#22544,#22545,#22546,#22547,
#22548,#22549,#22550,#22551,#22552,#22553,#22554,#22555,#22556,#22557,#22558,
#22559,#22560,#22561,#22562,#22563,#22564,#22565,#22566,#22567,#22568,#22569,
#22570,#22571,#22572,#22573,#22574,#22575,#22576,#22577,#22578,#22579,#22580,
#22581,#22582,#22583,#22584,#22585,#22586,#22587,#22588,#22589,#22590,#22591,
#22592,#22593,#22594,#22595,#22596,#22597,#22598,#22599,#22600,#22601,#22602,
#22603,#22604,#22605,#22606,#22607,#22608,#22609,#22610,#22611,#22612,#22613,
#22614,#22615,#22616,#22617,#22618,#22619,#22620,#22621,#22622,#22623,#22624,
#22625,#22626,#22627,#22628,#22629,#22630,#22631),.UNSPECIFIED.,.F.,.F.,
(4,2,2,2,2,2,2,2,2,2,2,2,2,2,2,2,2,2,2,2,2,2,2,2,2,2,2,2,2,2,2,2,2,2,2,
2,2,2,2,2,2,2,2,2,2,2,2,2,2,2,2,2,2,2,2,2,2,2,2,2,4),(-4.76536606648679,
-4.73995330058825,-4.71428216208692,-4.66787760840187,-4.62090001828672,
-4.57489315196683,-4.52827598031504,-4.48324174099382,-4.43009800411536,
-4.369121138706,-4.29487581998578,-4.20813123159048,-4.10264285994218,-3.98300404400089,
-3.85498183567728,-3.75603277417739,-3.66753945071753,-3.59513830902217,
-3.53043031686988,-3.46497596671772,-3.39858338931495,-3.33150995436675,
-3.26576336965161,-3.19985780580732,-3.13665860631666,-3.06231583446353,
-2.97714279455585,-2.87386617237767,-2.75352803138844,-2.59465312769161,
-2.38272456896879,-2.17079601024594,-2.01192110655013,-1.8915829655621,
-1.78830634338503,-1.70313330347825,-1.62879053162583,-1.56559133213577,
-1.499685768292,-1.43393918357727,-1.36686574862954,-1.30047317122726,-1.23501882107553,
-1.17031082892357,-1.09790968722854,-1.00941636376919,-0.910467302270004,
-0.78244509394716,-0.662806278006525,-0.557317906358945,-0.470573317964312,
-0.396327999244839,-0.335351133836078,-0.282207396957964,-0.237173157637031,
-0.19055598598568,-0.144549119666231,-0.0975715295514552,-0.0511669758667642,
-0.0254958373655805,-8.30537880556699E-5),.UNSPECIFIED.);
#2198=B_SPLINE_CURVE_WITH_KNOTS('',3,(#22774,#22775,#22776,#22777,#22778,
#22779),.UNSPECIFIED.,.F.,.F.,(4,2,4),(-0.0116317960480669,-0.00585615791721894,
-8.47905377083857E-5),.UNSPECIFIED.);
#2199=B_SPLINE_CURVE_WITH_KNOTS('',3,(#22780,#22781,#22782,#22783,#22784,
#22785,#22786,#22787,#22788,#22789,#22790,#22791,#22792,#22793,#22794,#22795,
#22796,#22797,#22798,#22799,#22800,#22801,#22802,#22803,#22804,#22805,#22806,
#22807,#22808,#22809,#22810,#22811,#22812,#22813,#22814,#22815,#22816,#22817,
#22818,#22819,#22820,#22821,#22822,#22823,#22824,#22825,#22826,#22827,#22828,
#22829,#22830,#22831,#22832,#22833,#22834,#22835,#22836,#22837,#22838,#22839,
#22840,#22841,#22842,#22843,#22844,#22845,#22846,#22847,#22848,#22849,#22850,
#22851,#22852,#22853,#22854,#22855,#22856,#22857,#22858,#22859,#22860,#22861,
#22862,#22863,#22864,#22865,#22866,#22867,#22868,#22869,#22870,#22871,#22872,
#22873,#22874,#22875,#22876,#22877,#22878,#22879,#22880,#22881,#22882,#22883,
#22884,#22885,#22886,#22887,#22888,#22889,#22890,#22891,#22892,#22893,#22894,
#22895,#22896,#22897,#22898,#22899,#22900,#22901),.UNSPECIFIED.,.F.,.F.,
(4,2,2,2,2,2,2,2,2,2,2,2,2,2,2,2,2,2,2,2,2,2,2,2,2,2,2,2,2,2,2,2,2,2,2,
2,2,2,2,2,2,2,2,2,2,2,2,2,2,2,2,2,2,2,2,2,2,2,2,2,4),(8.23445128364946E-5,
0.0254955919483662,0.0511664822196668,0.097571040701871,0.144548635673389,
0.190555506749416,0.237172683220333,0.282206927196841,0.335350669568886,
0.396327541281621,0.470572867676824,0.557317465039227,0.662805847592082,
0.782444675900308,0.910466897457627,1.00941596918587,1.0979093017932,1.17031045097264,
1.23501844981379,1.30047280673184,1.36686539099743,1.43393883287884,1.49968542438998,
1.56559099504675,1.62879020107028,1.70313298060813,1.78830602931986,1.89158266217341,
2.0119208156019,2.17079573572116,2.3827243163491,2.59465289697705,2.75352781709642,
2.87386597052503,2.97714260337883,3.06231565209077,3.13665843162885,3.19985763765255,
3.26576320830941,3.33150979982066,3.39858324170221,3.46497582596794,3.53043018288608,
3.59513818172725,3.66753933090672,3.75603266351411,3.85498173524235,3.98300395679958,
4.10264278510785,4.20813116766099,4.2948757650237,4.36912109141912,4.43009796313204,
4.48324170550436,4.5282759494811,4.57489312595195,4.6208999970278,4.6678775919993,
4.71428215048147,4.73995329163655,4.76536606016219),.UNSPECIFIED.);
#2200=B_SPLINE_CURVE_WITH_KNOTS('',3,(#22902,#22903,#22904,#22905,#22906,
#22907,#22908,#22909,#22910,#22911,#22912,#22913,#22914,#22915,#22916,#22917,
#22918,#22919,#22920,#22921,#22922,#22923,#22924,#22925,#22926,#22927,#22928,
#22929,#22930,#22931,#22932,#22933,#22934,#22935,#22936,#22937,#22938,#22939,
#22940,#22941,#22942,#22943,#22944,#22945,#22946,#22947,#22948,#22949,#22950,
#22951,#22952,#22953,#22954,#22955,#22956,#22957,#22958,#22959,#22960,#22961,
#22962,#22963,#22964,#22965,#22966,#22967,#22968,#22969,#22970,#22971,#22972,
#22973,#22974,#22975,#22976,#22977,#22978,#22979,#22980,#22981,#22982,#22983,
#22984,#22985,#22986,#22987,#22988,#22989,#22990,#22991,#22992,#22993,#22994,
#22995,#22996,#22997,#22998,#22999,#23000,#23001,#23002,#23003,#23004,#23005,
#23006,#23007,#23008,#23009,#23010,#23011,#23012,#23013,#23014,#23015,#23016,
#23017,#23018,#23019,#23020,#23021,#23022,#23023),.UNSPECIFIED.,.F.,.F.,
(4,2,2,2,2,2,2,2,2,2,2,2,2,2,2,2,2,2,2,2,2,2,2,2,2,2,2,2,2,2,2,2,2,2,2,
2,2,2,2,2,2,2,2,2,2,2,2,2,2,2,2,2,2,2,2,2,2,2,2,2,4),(-4.76536629622447,
-4.73995309969356,-4.71428216203548,-4.66787760835079,-4.62090001823604,
-4.57489315191641,-4.528275980265,-4.48324174094435,-4.43009800406656,-4.36912113865791,
-4.29487581993855,-4.20813123154422,-4.10264285989725,-3.98300404395784,
-3.85498183563605,-3.75603277413762,-3.66753945067915,-3.59513830898487,
-3.53043031683354,-3.46497596668246,-3.39858338928084,-3.3315099543338,
-3.26576336961984,-3.19985780577669,-3.136658606287,-3.06231583443505,-2.97714279452891,
-2.87386617235258,-2.75352803136521,-2.59465312767118,-2.3827245689534,
-2.17079601023561,-2.01192110654139,-1.89158296555381,-1.78830634337716,
-1.70313330347075,-1.62879053161852,-1.56559133212861,-1.49968576828534,
-1.43393918357123,-1.36686574862399,-1.30047317122219,-1.23501882107098,
-1.17031082891958,-1.09790968722523,-1.00941636376664,-0.91046730226815,
-0.782445093946358,-0.662806278006812,-0.557317906359464,-0.470573317964745,
-0.396327999245099,-0.335351133836203,-0.282207396958087,-0.237173157637164,
-0.190555985985781,-0.144549119666305,-0.0975715295515277,-0.0511669758668496,
-0.0254958373656227,-8.30537880558869E-5),.UNSPECIFIED.);
#2201=B_SPLINE_CURVE_WITH_KNOTS('',3,(#23030,#23031,#23032,#23033,#23034,
#23035),.UNSPECIFIED.,.F.,.F.,(4,2,4),(-0.0385635633195077,-0.0192648014145305,
-5.6512677524232E-5),.UNSPECIFIED.);
#2202=B_SPLINE_CURVE_WITH_KNOTS('',3,(#23036,#23037,#23038,#23039,#23040,
#23041),.UNSPECIFIED.,.F.,.F.,(4,2,4),(-0.020013276506786,-0.010090500778054,
-1.26246806509996E-5),.UNSPECIFIED.);
#2203=B_SPLINE_CURVE_WITH_KNOTS('',3,(#23044,#23045,#23046,#23047,#23048,
#23049,#23050,#23051,#23052,#23053),.UNSPECIFIED.,.F.,.F.,(4,2,2,2,4),(-0.164908287572566,
-0.122123473574902,-0.0806835746227668,-0.039806081275496,-5.30404670007887E-5),
 .UNSPECIFIED.);
#2204=B_SPLINE_CURVE_WITH_KNOTS('',3,(#23055,#23056,#23057,#23058),
 .UNSPECIFIED.,.F.,.F.,(4,4),(-0.00327039655086957,0.),.UNSPECIFIED.);
#2205=B_SPLINE_CURVE_WITH_KNOTS('',3,(#23202,#23203,#23204,#23205,#23206,
#23207,#23208,#23209,#23210,#23211,#23212,#23213,#23214,#23215,#23216,#23217,
#23218,#23219,#23220,#23221,#23222,#23223,#23224,#23225,#23226,#23227,#23228,
#23229,#23230,#23231,#23232,#23233,#23234,#23235,#23236,#23237,#23238,#23239,
#23240,#23241,#23242,#23243,#23244,#23245,#23246,#23247,#23248,#23249,#23250,
#23251,#23252,#23253,#23254,#23255,#23256,#23257,#23258,#23259,#23260,#23261,
#23262,#23263,#23264,#23265,#23266,#23267,#23268,#23269,#23270,#23271,#23272,
#23273,#23274,#23275,#23276,#23277,#23278,#23279,#23280,#23281,#23282,#23283,
#23284,#23285,#23286,#23287,#23288,#23289,#23290,#23291,#23292,#23293,#23294,
#23295,#23296,#23297,#23298,#23299,#23300,#23301,#23302,#23303,#23304,#23305,
#23306,#23307,#23308,#23309,#23310,#23311,#23312,#23313,#23314,#23315,#23316,
#23317,#23318,#23319,#23320,#23321,#23322,#23323,#23324,#23325,#23326,#23327,
#23328,#23329,#23330,#23331,#23332,#23333,#23334,#23335,#23336,#23337,#23338,
#23339,#23340,#23341,#23342,#23343,#23344,#23345,#23346,#23347,#23348,#23349,
#23350,#23351,#23352,#23353,#23354,#23355,#23356,#23357,#23358,#23359,#23360,
#23361,#23362,#23363,#23364,#23365,#23366,#23367,#23368,#23369,#23370,#23371,
#23372,#23373,#23374,#23375,#23376,#23377,#23378,#23379,#23380,#23381,#23382,
#23383),.UNSPECIFIED.,.F.,.F.,(4,2,2,2,2,2,2,2,2,2,2,2,2,2,2,2,2,2,2,2,
2,2,2,2,2,2,2,2,2,2,2,2,2,2,2,2,2,2,2,2,2,2,2,2,2,2,2,2,2,2,2,2,2,2,2,2,
2,2,2,2,2,2,2,2,2,2,2,2,2,2,2,2,2,2,2,2,2,2,2,2,2,2,2,2,2,2,2,2,2,2,4),
(-2.59382312359622,-2.56809909206607,-2.54791923390964,-2.51910185607888,
-2.50034924577938,-2.46359383453845,-2.44228542443783,-2.40669510295705,
-2.38725922606837,-2.35093961748984,-2.32890149074397,-2.29239847801421,
-2.27292633852247,-2.23609702873241,-2.21402640049839,-2.17733101201315,
-2.15768968532709,-2.12058782546055,-2.09831665072369,-2.06132017512561,
-2.04151153117669,-2.00410711813897,-1.98164874928756,-1.94433785593902,
-1.92436895247648,-1.88665456227707,-1.86401301910331,-1.82639412910864,
-1.80626110387503,-1.76824586383648,-1.7454134243349,-1.70746632183097,
-1.68717332827363,-1.64888670526784,-1.62585024949674,-1.58750854158364,
-1.56707629965118,-1.52867376524863,-1.50537210168194,-1.46632826658595,
-1.44585935678816,-1.40809290140965,-1.3842352254204,-1.34299194673546,
-1.32298293946475,-1.29075419136106,-1.25234706644214,-1.23077326808129,
-1.19286916386442,-1.16895424934302,-1.13063711273809,-1.10923927510981,
-1.07184448765126,-1.04819507852277,-1.0102014896849,-0.989011098243588,
-0.952022048741237,-0.928617115515581,-0.890994268266284,-0.870016399552206,
-0.833407705734039,-0.810240713299895,-0.772995938467394,-0.752229959132093,
-0.715993811809521,-0.693062394391416,-0.65619295215658,-0.635637857528421,
-0.599765415733702,-0.577063393911802,-0.540570727917672,-0.520220615948578,
-0.484721518808244,-0.46225404518635,-0.426125838650698,-0.405988720282876,
-0.370840574739169,-0.34861332772549,-0.312828499163541,-0.29289941060862,
-0.258015550215702,-0.235878653318305,-0.200645947107353,-0.18079872486045,
-0.14688892260254,-0.125531840866317,-0.0899005543185674,-0.0708164474537418,
-0.0422875992108556,-0.0109151062078881,-4.06978878030363E-5),
 .UNSPECIFIED.);
#2206=B_SPLINE_CURVE_WITH_KNOTS('',3,(#23384,#23385,#23386,#23387,#23388,
#23389,#23390,#23391,#23392,#23393,#23394,#23395,#23396,#23397,#23398,#23399,
#23400,#23401,#23402,#23403,#23404,#23405,#23406,#23407,#23408,#23409,#23410,
#23411,#23412,#23413,#23414,#23415,#23416,#23417,#23418,#23419,#23420,#23421,
#23422,#23423,#23424,#23425,#23426,#23427,#23428,#23429,#23430,#23431,#23432,
#23433,#23434,#23435,#23436,#23437,#23438,#23439,#23440,#23441,#23442,#23443,
#23444,#23445),.UNSPECIFIED.,.F.,.F.,(4,2,2,2,2,2,2,2,2,2,2,2,2,2,2,2,2,
2,2,2,2,2,2,2,2,2,2,2,2,2,4),(3.71452156639363E-5,0.018383146637255,0.0405642397108187,
0.0668325597898111,0.111436908431686,0.126394165236214,0.15274397121657,
0.178584594200384,0.215756491831179,0.233810618177999,0.252791145534099,
0.282553240098289,0.311403566815716,0.338930071939597,0.357138036654115,
0.385287554485539,0.412804972902094,0.43983249965415,0.4635752087772,0.479766666968338,
0.500014603141655,0.528593762245753,0.559905689917596,0.578104831901803,
0.599380635704931,0.630875077930314,0.656634519607673,0.683634545887361,
0.699020384949516,0.735639212358386,0.769952845650509),.UNSPECIFIED.);
#2207=B_SPLINE_CURVE_WITH_KNOTS('',3,(#23588,#23589,#23590,#23591,#23592,
#23593,#23594,#23595,#23596,#23597,#23598,#23599,#23600,#23601,#23602,#23603,
#23604,#23605,#23606,#23607,#23608,#23609,#23610,#23611,#23612,#23613,#23614,
#23615,#23616,#23617,#23618,#23619,#23620,#23621,#23622,#23623,#23624,#23625,
#23626,#23627,#23628,#23629,#23630,#23631,#23632,#23633,#23634,#23635,#23636,
#23637,#23638,#23639),.UNSPECIFIED.,.F.,.F.,(4,2,2,2,2,2,2,2,2,2,2,2,2,
2,2,2,2,2,2,2,2,2,2,2,2,4),(-0.949553103265687,-0.906923078453489,-0.866427431983837,
-0.832934013363288,-0.799266013989078,-0.750746029004779,-0.70890633730406,
-0.678129159719416,-0.648036604752675,-0.612823612183411,-0.578073771721634,
-0.53409955835586,-0.500240107263163,-0.466498951022295,-0.429736799555293,
-0.373388222676778,-0.338335060909048,-0.302283409606239,-0.272030647531648,
-0.24247187701457,-0.198686709372544,-0.149970580195427,-0.114177073472312,
-0.0775700325473158,-0.0396702823667157,-5.56419586003635E-5),
 .UNSPECIFIED.);
#2208=B_SPLINE_CURVE_WITH_KNOTS('',3,(#23782,#23783,#23784,#23785,#23786,
#23787,#23788,#23789,#23790,#23791,#23792,#23793,#23794,#23795,#23796,#23797,
#23798,#23799,#23800,#23801,#23802,#23803,#23804,#23805,#23806,#23807,#23808,
#23809,#23810,#23811,#23812,#23813,#23814,#23815,#23816,#23817,#23818,#23819,
#23820,#23821,#23822,#23823,#23824,#23825,#23826,#23827,#23828,#23829,#23830,
#23831,#23832,#23833,#23834,#23835,#23836,#23837,#23838,#23839,#23840,#23841,
#23842,#23843,#23844,#23845,#23846,#23847,#23848,#23849,#23850,#23851,#23852,
#23853,#23854,#23855,#23856,#23857,#23858,#23859,#23860,#23861,#23862,#23863,
#23864,#23865,#23866,#23867,#23868,#23869,#23870,#23871,#23872,#23873,#23874,
#23875,#23876,#23877,#23878,#23879,#23880,#23881,#23882,#23883,#23884,#23885,
#23886,#23887,#23888,#23889,#23890,#23891,#23892,#23893,#23894,#23895,#23896,
#23897,#23898,#23899,#23900,#23901,#23902,#23903,#23904,#23905,#23906,#23907,
#23908,#23909,#23910,#23911,#23912,#23913,#23914,#23915,#23916,#23917,#23918,
#23919,#23920,#23921,#23922,#23923,#23924,#23925,#23926,#23927,#23928,#23929,
#23930,#23931,#23932,#23933,#23934,#23935,#23936,#23937,#23938,#23939,#23940,
#23941,#23942,#23943,#23944,#23945,#23946,#23947,#23948,#23949,#23950,#23951,
#23952,#23953,#23954,#23955,#23956,#23957,#23958,#23959,#23960,#23961,#23962,
#23963,#23964,#23965),.UNSPECIFIED.,.F.,.F.,(4,2,2,2,2,2,2,2,2,2,2,2,2,
2,2,2,2,2,2,2,2,2,2,2,2,2,2,2,2,2,2,2,2,2,2,2,2,2,2,2,2,2,2,2,2,2,2,2,2,
2,2,2,2,2,2,2,2,2,2,2,2,2,2,2,2,2,2,2,2,2,2,2,2,2,2,2,2,2,2,2,2,2,2,2,2,
2,2,2,2,2,2,4),(-2.59123053346005,-2.56554791306885,-2.5453719157918,-2.51664536202888,
-2.4979272184796,-2.46123935800588,-2.4399701154689,-2.40444522219546,-2.38504506442642,
-2.34879218067922,-2.32679457228015,-2.29035871364016,-2.27092234335711,
-2.23416057794242,-2.21213057161506,-2.17550291691656,-2.15589759275248,
-2.11886322652973,-2.09663324953121,-2.05970612839742,-2.03993342751461,
-2.00259445787734,-1.98017860959789,-1.94294268966605,-1.92300829110486,
-1.88534761025334,-1.86275354289858,-1.82523398778967,-1.80512758745354,
-1.7671085292704,-1.74434570998078,-1.70661417579985,-1.68630796422811,
-1.6477334822438,-1.62487351397267,-1.58731784522435,-1.56667351509398,
-1.52656870737691,-1.50396763108559,-1.46858519930174,-1.44687021778233,
-1.41609830641339,-1.38781739596686,-1.36318087074456,-1.3319839559769,
-1.30633301324762,-1.27148566807694,-1.24636686706974,-1.21848731795896,
-1.19235118508901,-1.16802264402101,-1.13083394326271,-1.10959551436729,
-1.07173452508517,-1.04799931079223,-1.0102484851039,-0.989093753270532,
-0.95200616560291,-0.928584032070876,-0.891015553096991,-0.87004651572887,
-0.833418504136608,-0.810249040962625,-0.773017999631342,-0.752255039993863,
-0.716016661261408,-0.693085938451044,-0.656221436670924,-0.635668095014566,
-0.599797092346128,-0.577096436314295,-0.540606791511633,-0.520258147978269,
-0.484761262636764,-0.462295287128823,-0.426169667909789,-0.406033944974079,
-0.370888159493564,-0.348662426167541,-0.312880073138577,-0.292952353160038,
-0.258070871960243,-0.235935489472284,-0.200705201839718,-0.180859339822398,
-0.146951858120951,-0.125596238893428,-0.0899673941394749,-0.0708845946511137,
-0.0423960687609541,-0.0111460198812575,-0.000107286410718428),
 .UNSPECIFIED.);
#2209=B_SPLINE_CURVE_WITH_KNOTS('',3,(#23967,#23968,#23969,#23970,#23971,
#23972,#23973,#23974,#23975,#23976,#23977,#23978,#23979,#23980,#23981,#23982,
#23983,#23984,#23985,#23986,#23987,#23988,#23989,#23990,#23991,#23992,#23993,
#23994,#23995,#23996,#23997,#23998,#23999,#24000,#24001,#24002,#24003,#24004,
#24005,#24006,#24007,#24008,#24009,#24010,#24011,#24012,#24013,#24014,#24015,
#24016),.UNSPECIFIED.,.F.,.F.,(4,2,2,2,2,2,2,2,2,2,2,2,2,2,2,2,2,2,2,2,
2,2,2,2,4),(-0.956982439280623,-0.903526122456605,-0.854507497013016,-0.826934563946404,
-0.799146057249082,-0.74241914188856,-0.714801687201639,-0.686583728369467,
-0.629857984674878,-0.602328820691834,-0.574130057528638,-0.517525223454158,
-0.478071053229473,-0.434312794595821,-0.37788167184512,-0.351722969094686,
-0.322816305907384,-0.266404182629574,-0.239982209276222,-0.194476830584044,
-0.150231700054167,-0.115576342024155,-0.0803424134121,-0.0412201593161153,
-5.56420009251838E-5),.UNSPECIFIED.);
#2210=B_SPLINE_CURVE_WITH_KNOTS('',3,(#24301,#24302,#24303,#24304,#24305,
#24306,#24307,#24308,#24309,#24310,#24311,#24312,#24313,#24314,#24315,#24316,
#24317,#24318,#24319,#24320,#24321,#24322,#24323,#24324,#24325,#24326,#24327,
#24328,#24329,#24330,#24331,#24332,#24333,#24334,#24335,#24336,#24337,#24338,
#24339,#24340,#24341,#24342,#24343,#24344,#24345,#24346,#24347,#24348,#24349,
#24350,#24351,#24352,#24353,#24354,#24355,#24356,#24357,#24358,#24359,#24360,
#24361,#24362,#24363,#24364,#24365,#24366,#24367,#24368,#24369,#24370,#24371,
#24372,#24373,#24374,#24375,#24376,#24377,#24378,#24379,#24380,#24381,#24382,
#24383,#24384,#24385,#24386,#24387,#24388,#24389,#24390,#24391,#24392,#24393,
#24394,#24395,#24396,#24397,#24398,#24399,#24400,#24401,#24402,#24403,#24404,
#24405,#24406,#24407,#24408,#24409,#24410,#24411,#24412,#24413,#24414,#24415,
#24416,#24417,#24418,#24419,#24420,#24421,#24422,#24423,#24424,#24425,#24426,
#24427,#24428,#24429,#24430,#24431,#24432,#24433,#24434,#24435,#24436,#24437,
#24438,#24439,#24440,#24441,#24442,#24443,#24444,#24445,#24446,#24447,#24448,
#24449,#24450,#24451,#24452,#24453,#24454,#24455,#24456,#24457,#24458,#24459,
#24460,#24461,#24462,#24463,#24464,#24465,#24466,#24467,#24468,#24469,#24470,
#24471,#24472,#24473,#24474,#24475,#24476,#24477,#24478,#24479,#24480,#24481,
#24482,#24483,#24484),.UNSPECIFIED.,.F.,.F.,(4,2,2,2,2,2,2,2,2,2,2,2,2,
2,2,2,2,2,2,2,2,2,2,2,2,2,2,2,2,2,2,2,2,2,2,2,2,2,2,2,2,2,2,2,2,2,2,2,2,
2,2,2,2,2,2,2,2,2,2,2,2,2,2,2,2,2,2,2,2,2,2,2,2,2,2,2,2,2,2,2,2,2,2,2,2,
2,2,2,2,2,2,4),(-2.59926568599725,-2.57341790284738,-2.55311215565756,-2.52420086050638,
-2.50536234343823,-2.46843855566556,-2.44703252902056,-2.4112791597983,
-2.391754247624,-2.35526827028152,-2.33312917976257,-2.29645891621898,-2.27689758284438,
-2.23989962259838,-2.21772786179071,-2.18086423847728,-2.16113297812973,
-2.12386146986842,-2.10148814969433,-2.06432157510582,-2.04442239771826,
-2.00684813433544,-1.98428631780977,-1.94680159503098,-1.92674221101307,
-1.88886214023063,-1.86611421132941,-1.82830927241362,-1.80808872880043,
-1.76993282004507,-1.74698320390566,-1.70879753274252,-1.68843379724343,
-1.65012993509938,-1.62692839119727,-1.58810546149191,-1.56768405599013,
-1.52985794423679,-1.50616290607375,-1.47839724920395,-1.45176005974334,
-1.42617681964575,-1.39187166363256,-1.36625834747285,-1.33310974750308,
-1.307442980506,-1.27425765223016,-1.24797027958099,-1.2221641264784,-1.19225399591173,
-1.16784392150644,-1.13087222960183,-1.10966347390913,-1.07171391025553,
-1.04796213922683,-1.01025663207545,-0.989108333184153,-0.952001711293397,
-0.928576033211906,-0.891017281638817,-0.870049615157352,-0.833417556059424,
-0.81024734024633,-0.773018372760037,-0.752255709310832,-0.71601645648305,
-0.693085571189003,-0.656221517262033,-0.635668239582674,-0.599797048122477,
-0.577096356996304,-0.540606808908221,-0.520258179190347,-0.484761253088374,
-0.46229527000396,-0.426169671671616,-0.406033951720906,-0.370888157427394,
-0.348662422463881,-0.312880073953667,-0.292952354619784,-0.258070871518592,
-0.235935488676309,-0.200705202010143,-0.180859340129984,-0.14695185802523,
-0.125596238723843,-0.0899673941804166,-0.0708845947225205,-0.0423960687560085,
-0.011146019861744,-0.000107286410493566),.UNSPECIFIED.);
#2211=B_SPLINE_CURVE_WITH_KNOTS('',3,(#24626,#24627,#24628,#24629,#24630,
#24631,#24632,#24633,#24634,#24635,#24636,#24637,#24638,#24639,#24640,#24641,
#24642,#24643,#24644,#24645,#24646,#24647,#24648,#24649,#24650,#24651,#24652,
#24653,#24654,#24655,#24656,#24657,#24658,#24659,#24660,#24661,#24662,#24663,
#24664,#24665,#24666,#24667,#24668,#24669,#24670,#24671,#24672,#24673),
 .UNSPECIFIED.,.F.,.F.,(4,2,2,2,2,2,2,2,2,2,2,2,2,2,2,2,2,2,2,2,2,2,2,4),
(-1.10411146984742,-1.03533191665006,-0.976118742178351,-0.919309605921176,
-0.852147695059822,-0.818850329922423,-0.78710553631429,-0.719605202451663,
-0.685897537282491,-0.653720218096601,-0.58591693177771,-0.533253067073543,
-0.48048894685478,-0.412938810261147,-0.380861562376602,-0.345537529156284,
-0.278404282958939,-0.244685076002604,-0.208482114930744,-0.147691075996069,
-0.119500524352719,-0.0875443739883855,-0.0452588878587829,-5.56419715291266E-5),
 .UNSPECIFIED.);
#2212=B_SPLINE_CURVE_WITH_KNOTS('',3,(#24815,#24816,#24817,#24818,#24819,
#24820,#24821,#24822,#24823,#24824,#24825,#24826,#24827,#24828,#24829,#24830,
#24831,#24832,#24833,#24834,#24835,#24836,#24837,#24838,#24839,#24840,#24841,
#24842,#24843,#24844,#24845,#24846,#24847,#24848,#24849,#24850,#24851,#24852,
#24853,#24854,#24855,#24856,#24857,#24858,#24859,#24860,#24861,#24862,#24863,
#24864,#24865,#24866,#24867,#24868,#24869,#24870,#24871,#24872,#24873,#24874,
#24875,#24876,#24877,#24878,#24879,#24880,#24881,#24882,#24883,#24884,#24885,
#24886,#24887,#24888,#24889,#24890,#24891,#24892,#24893,#24894,#24895,#24896,
#24897,#24898,#24899,#24900,#24901,#24902,#24903,#24904,#24905,#24906,#24907,
#24908,#24909,#24910,#24911,#24912,#24913,#24914,#24915,#24916,#24917,#24918,
#24919,#24920,#24921,#24922,#24923,#24924,#24925,#24926,#24927,#24928,#24929,
#24930,#24931,#24932,#24933,#24934,#24935,#24936,#24937,#24938,#24939,#24940,
#24941,#24942,#24943,#24944,#24945,#24946,#24947,#24948,#24949,#24950,#24951,
#24952,#24953,#24954,#24955,#24956,#24957,#24958,#24959,#24960,#24961,#24962,
#24963,#24964,#24965,#24966,#24967,#24968,#24969,#24970,#24971,#24972,#24973,
#24974,#24975,#24976,#24977,#24978,#24979,#24980,#24981,#24982,#24983,#24984,
#24985,#24986,#24987,#24988,#24989,#24990,#24991,#24992,#24993,#24994,#24995,
#24996),.UNSPECIFIED.,.F.,.F.,(4,2,2,2,2,2,2,2,2,2,2,2,2,2,2,2,2,2,2,2,
2,2,2,2,2,2,2,2,2,2,2,2,2,2,2,2,2,2,2,2,2,2,2,2,2,2,2,2,2,2,2,2,2,2,2,2,
2,2,2,2,2,2,2,2,2,2,2,2,2,2,2,2,2,2,2,2,2,2,2,2,2,2,2,2,2,2,2,2,2,2,4),
(-2.59260712215313,-2.56690100601658,-2.54670662204792,-2.51795361125489,
-2.49921831040747,-2.46249682575997,-2.44120808436947,-2.40565061488907,
-2.38623267798292,-2.34994659263002,-2.32792880857738,-2.2914594924406,
-2.27200532567065,-2.23521000439549,-2.21315975079308,-2.17649824646819,
-2.15687504523822,-2.1198074010745,-2.09755679524307,-2.06059452890559,
-2.04080414862994,-2.0034341153344,-1.98099653145175,-1.94372036045755,
-1.92376979199521,-1.88608952366635,-1.86346913878391,-1.825886307371,-1.80577140708762,
-1.7677879985442,-1.74497785805425,-1.70707208286967,-1.68679565593267,
-1.64852898921098,-1.62551957915289,-1.58724299799866,-1.5668194156521,
-1.52837962022198,-1.50512689617436,-1.46625959367599,-1.445761725099,-1.4076809055734,
-1.38397962847684,-1.34347567036628,-1.32325230788248,-1.28842096624431,
-1.25281821723327,-1.23161829626377,-1.19259825825371,-1.16847365331844,
-1.13073625058469,-1.10942156761083,-1.07178747146495,-1.04809462598784,
-1.01022758913448,-0.989056327476576,-0.952017607520454,-0.928604568917411,
-0.891011047611388,-0.870038435830354,-0.833420975844612,-0.810253474529773,
-0.773017026933345,-0.75225329511157,-0.716017195124668,-0.693086895893007,
-0.656221226579299,-0.635667718134776,-0.599797207642169,-0.577096643100117,
-0.540606746163167,-0.520258066612007,-0.48476128753358,-0.462295331776445,
-0.42616965811013,-0.406033927396684,-0.370888164878453,-0.34866243581743,
-0.312880071015608,-0.292952349354644,-0.25807087311542,-0.235935491552819,
-0.200705201394322,-0.18085933901615,-0.146951858374274,-0.125596239341413,
-0.0899673940341012,-0.0708845944680406,-0.0423960687726755,-0.0111460199290559,
-0.000107286410655352),.UNSPECIFIED.);
#2213=B_SPLINE_CURVE_WITH_KNOTS('',3,(#25159,#25160,#25161,#25162,#25163,
#25164,#25165,#25166,#25167,#25168,#25169,#25170,#25171,#25172,#25173,#25174),
 .UNSPECIFIED.,.F.,.F.,(4,2,2,2,2,2,2,4),(-0.997882818540195,-0.95890297017825,
-0.915601512736776,-0.890692190934456,-0.842383484706287,-0.788483554860223,
-0.738305310250689,-0.724835095226849),.UNSPECIFIED.);
#2214=B_SPLINE_CURVE_WITH_KNOTS('',3,(#25180,#25181,#25182,#25183,#25184,
#25185,#25186,#25187,#25188,#25189,#25190,#25191,#25192,#25193,#25194,#25195,
#25196,#25197,#25198),.UNSPECIFIED.,.F.,.F.,(4,3,3,3,3,3,4),(2.30639007129119E-6,
0.168219155399412,0.242220953770006,0.434178569252148,0.633536045455965,
0.816764967682345,0.999993889908724),.UNSPECIFIED.);
#2215=B_SPLINE_CURVE_WITH_KNOTS('',3,(#25205,#25206,#25207,#25208),
 .UNSPECIFIED.,.F.,.F.,(4,4),(-0.00458558691821468,0.),.UNSPECIFIED.);
#2216=B_SPLINE_CURVE_WITH_KNOTS('',3,(#25209,#25210,#25211,#25212,#25213,
#25214,#25215,#25216,#25217,#25218,#25219,#25220,#25221),.UNSPECIFIED.,
 .F.,.F.,(4,3,3,3,4),(0.,0.3333333333333,0.569543342469847,0.6666666666667,
0.99998534170567),.UNSPECIFIED.);
#2217=B_SPLINE_CURVE_WITH_KNOTS('',3,(#25363,#25364,#25365,#25366,#25367,
#25368,#25369,#25370,#25371,#25372,#25373,#25374,#25375,#25376,#25377,#25378,
#25379,#25380,#25381,#25382,#25383,#25384,#25385,#25386,#25387,#25388,#25389,
#25390,#25391,#25392,#25393,#25394,#25395,#25396,#25397,#25398,#25399,#25400,
#25401,#25402,#25403,#25404,#25405,#25406,#25407,#25408,#25409,#25410,#25411,
#25412,#25413,#25414,#25415,#25416,#25417,#25418,#25419,#25420,#25421,#25422,
#25423,#25424,#25425,#25426,#25427,#25428,#25429,#25430,#25431,#25432,#25433,
#25434,#25435,#25436,#25437,#25438,#25439,#25440,#25441,#25442,#25443,#25444,
#25445,#25446,#25447,#25448,#25449,#25450,#25451,#25452,#25453,#25454,#25455,
#25456,#25457,#25458,#25459,#25460,#25461,#25462,#25463,#25464,#25465,#25466,
#25467,#25468,#25469,#25470,#25471,#25472,#25473,#25474,#25475,#25476,#25477,
#25478,#25479,#25480,#25481,#25482,#25483,#25484,#25485,#25486,#25487,#25488,
#25489,#25490,#25491,#25492,#25493,#25494,#25495,#25496,#25497,#25498,#25499,
#25500,#25501,#25502,#25503,#25504,#25505,#25506,#25507,#25508,#25509,#25510,
#25511,#25512,#25513,#25514,#25515,#25516,#25517,#25518,#25519,#25520,#25521,
#25522,#25523,#25524,#25525,#25526,#25527,#25528,#25529,#25530,#25531,#25532,
#25533,#25534,#25535,#25536,#25537,#25538,#25539,#25540,#25541,#25542,#25543,
#25544,#25545,#25546,#25547,#25548,#25549,#25550,#25551,#25552,#25553,#25554,
#25555,#25556,#25557,#25558,#25559,#25560,#25561,#25562,#25563,#25564,#25565,
#25566,#25567,#25568,#25569,#25570,#25571,#25572,#25573,#25574,#25575,#25576,
#25577,#25578,#25579,#25580,#25581,#25582,#25583,#25584,#25585,#25586,#25587,
#25588,#25589,#25590,#25591,#25592,#25593,#25594,#25595,#25596,#25597,#25598,
#25599,#25600,#25601,#25602,#25603,#25604,#25605,#25606,#25607,#25608,#25609,
#25610,#25611,#25612,#25613,#25614,#25615,#25616,#25617,#25618,#25619,#25620,
#25621,#25622,#25623,#25624,#25625,#25626,#25627,#25628,#25629,#25630,#25631,
#25632,#25633,#25634,#25635,#25636,#25637,#25638,#25639,#25640,#25641,#25642,
#25643,#25644,#25645,#25646,#25647,#25648,#25649,#25650,#25651,#25652,#25653,
#25654,#25655,#25656,#25657,#25658,#25659,#25660,#25661,#25662,#25663,#25664,
#25665,#25666,#25667,#25668,#25669,#25670,#25671,#25672,#25673,#25674,#25675,
#25676,#25677,#25678,#25679,#25680,#25681,#25682,#25683,#25684,#25685,#25686,
#25687,#25688,#25689,#25690,#25691,#25692,#25693,#25694,#25695,#25696,#25697,
#25698,#25699,#25700,#25701,#25702,#25703,#25704,#25705,#25706,#25707,#25708,
#25709,#25710,#25711,#25712,#25713,#25714,#25715,#25716,#25717,#25718,#25719,
#25720,#25721,#25722,#25723,#25724,#25725,#25726,#25727,#25728,#25729,#25730,
#25731,#25732,#25733,#25734,#25735,#25736,#25737,#25738,#25739,#25740,#25741,
#25742,#25743,#25744,#25745,#25746,#25747,#25748,#25749,#25750,#25751,#25752,
#25753,#25754,#25755,#25756,#25757,#25758,#25759,#25760),.UNSPECIFIED.,
 .F.,.F.,(4,2,2,2,2,2,2,2,2,2,2,2,2,2,2,2,2,2,2,2,2,2,2,2,2,2,2,2,2,2,2,
2,2,2,2,2,2,2,2,2,2,2,2,2,2,2,2,2,2,2,2,2,2,2,2,2,2,2,2,2,2,2,2,2,2,2,2,
2,2,2,2,2,2,2,2,2,2,2,2,2,2,2,2,2,2,2,2,2,2,2,2,2,2,2,2,2,2,2,2,2,2,2,2,
2,2,2,2,2,2,2,2,2,2,2,2,2,2,2,2,2,2,2,2,2,2,2,2,2,2,2,2,2,2,2,2,2,2,2,2,
2,2,2,2,2,2,2,2,2,2,2,2,2,2,2,2,2,2,2,2,2,2,2,2,2,2,2,2,2,2,2,2,2,2,2,2,
2,2,2,2,2,2,2,2,2,2,2,2,2,2,2,2,2,2,2,2,2,2,2,4),(-2.36492523745759,-2.34255296682852,
-2.3199656508682,-2.27585417903727,-2.25354275255567,-2.21054282254419,
-2.18644688059544,-2.17004409694976,-2.13488673135029,-2.11668240985326,
-2.10027976460783,-2.08774450478953,-2.05477340268109,-2.03507134009305,
-2.01951470315281,-2.00996653487751,-1.99755255991591,-1.97234100153057,
-1.95774451386731,-1.9481161572119,-1.93420090833259,-1.92534809472293,
-1.89682963918897,-1.88594722890426,-1.87680322226878,-1.86124282768097,
-1.85436376885839,-1.84672198839416,-1.83490432477196,-1.81557320818878,
-1.80683548582628,-1.79915234399613,-1.79070246008438,-1.77651955263018,
-1.76981925147615,-1.76127412212674,-1.7392331290447,-1.72754921515706,
-1.72102908066663,-1.71232177348829,-1.69956321522094,-1.69317593387435,
-1.68647055161581,-1.66712747464848,-1.65622744096082,-1.64814547719462,
-1.64243757267111,-1.62899360781887,-1.61728109210313,-1.61175268037231,
-1.60417666831167,-1.58353889221248,-1.57580174480183,-1.56938458299859,
-1.56423392904341,-1.54116632969256,-1.53581047383477,-1.53012761438281,
-1.51835316704718,-1.50377957088101,-1.49486795150478,-1.48978962379479,
-1.48382162476493,-1.46785015792272,-1.46210900183348,-1.45710386272981,
-1.45172301747603,-1.42952426827573,-1.42161170300879,-1.41537759326571,
-1.41082162980847,-1.40247391369265,-1.38876003207578,-1.38323377596955,
-1.37845252841154,-1.37334193458513,-1.3626827351202,-1.3483496471966,-1.34212107811774,
-1.33685971551491,-1.33230430814372,-1.3216514476077,-1.30967694883718,
-1.30435959610382,-1.29975527169422,-1.29481794690037,-1.2842053260138,
-1.27046886466486,-1.26230124198716,-1.25791300532331,-1.25246407651647,
-1.24245049601483,-1.23109500981515,-1.22581569534866,-1.22127092577752,
-1.21649755031245,-1.20597673592743,-1.19276104990642,-1.18699793818544,
-1.18214792478359,-1.17754136916297,-1.16646900262159,-1.14704014866058,
-1.14261167216771,-1.1377750265953,-1.13209365258579,-1.11948644571785,
-1.10919367696915,-1.10462395084307,-1.09968366141108,-1.08517547188672,
-1.06997765473393,-1.06510120098665,-1.0606500005824,-1.04935850990902,
-1.03150359941975,-1.02700605695584,-1.02160217029774,-1.01522712964587,
-1.00046230866128,-0.990911070885307,-0.986158745480183,-0.98139507987467,
-0.975719480081178,-0.962083468164042,-0.953955001953389,-0.949319869462239,
-0.94342315872656,-0.92738731581423,-0.91368226802068,-0.908353529354358,
-0.903742287718806,-0.898596623649472,-0.887515002696023,-0.877130058730485,
-0.872195218684388,-0.866145181709486,-0.851040400037946,-0.835407299386497,
-0.829790394065256,-0.824959791337494,-0.813731759798563,-0.799566971887483,
-0.794271584240714,-0.787490397253317,-0.779183255750064,-0.760336475939653,
-0.753074670747068,-0.748025261177741,-0.739172294288363,-0.724810587804851,
-0.718786017632848,-0.712382003253458,-0.694981768167063,-0.678671288174418,
-0.672343519043225,-0.666675285513522,-0.651141806748008,-0.643185979594139,
-0.636589194049217,-0.625072717792037,-0.60409709119821,-0.595806831686027,
-0.58981951476737,-0.5843561154383,-0.569891543895224,-0.562747028476868,
-0.553956616726265,-0.542955873544897,-0.520207904882434,-0.51313018313803,
-0.501814099198623,-0.489317266067134,-0.480801531073975,-0.461865586957671,
-0.441772150354699,-0.433644352633433,-0.423367939937679,-0.411008574535974,
-0.400547184327938,-0.388296277949455,-0.359851495711931,-0.35084867425318,
-0.342376920864329,-0.330234453560913,-0.314445598905012,-0.289223046175026,
-0.275676731870157,-0.265710680204558,-0.249661255292412,-0.223368235202192,
-0.198086384719217,-0.184067733214858,-0.159711123721348,-0.115000186891252,
-0.0973065370727581,-0.0573775607030809,-0.0287912440975278,-7.10237341792967E-5),
 .UNSPECIFIED.);
#2218=B_SPLINE_CURVE_WITH_KNOTS('',3,(#25763,#25764,#25765,#25766,#25767,
#25768,#25769,#25770,#25771,#25772,#25773,#25774,#25775,#25776,#25777,#25778,
#25779,#25780,#25781,#25782,#25783,#25784,#25785,#25786,#25787,#25788,#25789,
#25790,#25791,#25792,#25793,#25794,#25795,#25796,#25797,#25798,#25799,#25800,
#25801,#25802,#25803,#25804,#25805,#25806,#25807,#25808,#25809,#25810,#25811,
#25812,#25813,#25814,#25815,#25816,#25817,#25818,#25819,#25820,#25821,#25822,
#25823,#25824,#25825,#25826,#25827,#25828,#25829,#25830,#25831,#25832,#25833,
#25834,#25835,#25836,#25837,#25838,#25839,#25840,#25841,#25842,#25843,#25844,
#25845,#25846,#25847,#25848,#25849,#25850,#25851,#25852,#25853,#25854,#25855,
#25856,#25857,#25858,#25859,#25860,#25861,#25862,#25863,#25864,#25865,#25866,
#25867,#25868,#25869,#25870,#25871,#25872,#25873,#25874,#25875,#25876,#25877,
#25878,#25879,#25880),.UNSPECIFIED.,.F.,.F.,(4,2,2,2,2,2,2,2,2,2,2,2,2,
2,2,2,2,2,2,2,2,2,2,2,2,2,2,2,2,2,2,2,2,2,2,2,2,2,2,2,2,2,2,2,2,2,2,2,2,
2,2,2,2,2,2,2,2,2,4),(3.16667141335679E-5,0.0284893424911215,0.0571031677616148,
0.100536752903684,0.152083753002382,0.211276158594342,0.292188579082734,
0.399230061028865,0.503318852891491,0.587315507677329,0.66191283307897,
0.716273687751307,0.75975594936003,0.814048448551261,0.886012735934177,
0.971046167155236,1.06848597901879,1.19863510422438,1.37984377711638,1.57239515517755,
1.72626212591233,1.86298572050433,1.96198100642033,2.04139080933292,2.1368540562863,
2.25441211833114,2.39263076571147,2.55067957440204,2.74511452244579,2.97317398670225,
3.2012334509587,3.39566839900244,3.553717207693,3.69193585507333,3.80949391711816,
3.90495716407152,3.98436696698408,4.08336225290006,4.22008584749205,4.37395281822682,
4.56650419628796,4.74771286917995,4.87786199438553,4.97530180624906,5.0603352374701,
5.132299524853,5.18659202404421,5.23007428565291,5.28443514032522,5.35903246572685,
5.44302912051267,5.54711791237526,5.65415939432137,5.73507181480991,5.79426422040202,
5.84581122050084,5.88924480564302,5.91787547025432,5.9463098192052),
 .UNSPECIFIED.);
#2219=B_SPLINE_CURVE_WITH_KNOTS('',3,(#26026,#26027,#26028,#26029,#26030,
#26031,#26032,#26033,#26034,#26035,#26036,#26037,#26038,#26039,#26040,#26041,
#26042,#26043,#26044,#26045,#26046,#26047,#26048,#26049,#26050,#26051,#26052,
#26053,#26054,#26055,#26056,#26057,#26058,#26059,#26060,#26061,#26062,#26063,
#26064,#26065,#26066,#26067),.UNSPECIFIED.,.F.,.F.,(4,2,2,2,2,2,2,2,2,2,
2,2,2,2,2,2,2,2,2,2,4),(9.56954942354073E-5,0.0404351915602284,0.0809863227547807,
0.138729359916234,0.168045397626004,0.227812484620681,0.28784359795065,
0.346677928601178,0.375266441944433,0.434868223533285,0.464254085500563,
0.4930185317878,0.551407924605979,0.611332955424245,0.67040124768131,0.729413323150459,
0.788742910316018,0.817389104247561,0.87571192621649,0.91217639806824,0.948381630678781),
 .UNSPECIFIED.);
#2220=B_SPLINE_CURVE_WITH_KNOTS('',3,(#26069,#26070,#26071,#26072,#26073,
#26074,#26075,#26076,#26077,#26078,#26079,#26080,#26081,#26082,#26083,#26084,
#26085,#26086,#26087,#26088,#26089,#26090,#26091,#26092,#26093,#26094,#26095,
#26096,#26097,#26098,#26099,#26100,#26101,#26102,#26103,#26104,#26105,#26106,
#26107,#26108,#26109,#26110,#26111,#26112,#26113,#26114,#26115,#26116,#26117,
#26118,#26119,#26120,#26121,#26122,#26123,#26124,#26125,#26126,#26127,#26128,
#26129,#26130,#26131,#26132,#26133,#26134,#26135,#26136,#26137,#26138,#26139,
#26140,#26141,#26142,#26143,#26144,#26145,#26146,#26147,#26148,#26149,#26150,
#26151,#26152,#26153,#26154,#26155,#26156,#26157,#26158,#26159,#26160,#26161,
#26162,#26163,#26164,#26165,#26166,#26167,#26168,#26169,#26170),
 .UNSPECIFIED.,.F.,.F.,(4,2,2,2,2,2,2,2,2,2,2,2,2,2,2,2,2,2,2,2,2,2,2,2,
2,2,2,2,2,2,2,2,2,2,2,2,2,2,2,2,2,2,2,2,2,2,2,2,2,2,4),(-7.78033786116235,
-7.63085234138336,-7.49045462844376,-7.20406581382073,-6.99070882568832,
-6.77843585057195,-6.60078812217249,-6.41801603037867,-6.25219399969925,
-5.88201230226676,-5.68258509740488,-5.46562698484506,-5.09957693944957,
-4.89523762533434,-4.61995314186142,-4.25199639905186,-3.99742607058464,
-3.76323524666776,-3.42400292432898,-3.16991835794728,-2.92737133189385,
-2.63147231877444,-2.3304031238569,-1.91401229014332,-1.67248413718354,
-1.47051455546473,-1.31855523977063,-1.16408569562622,-1.10125811890718,
-1.01972820676982,-0.927975008243967,-0.813026949460111,-0.714310817432307,
-0.680192283916462,-0.640249373549641,-0.578742392923274,-0.539156183889252,
-0.507633333247703,-0.467186258890576,-0.428733937720528,-0.394809054534059,
-0.363669767787403,-0.33739791138586,-0.278612503104019,-0.24018447220225,
-0.20459026029123,-0.160285767953291,-0.0967339395859139,-0.07327066611358,
-0.0366392212630044,-1.00000000013978E-6),.UNSPECIFIED.);
#2221=B_SPLINE_CURVE_WITH_KNOTS('',3,(#26171,#26172,#26173,#26174,#26175,
#26176,#26177,#26178,#26179,#26180,#26181,#26182,#26183,#26184,#26185,#26186,
#26187,#26188,#26189,#26190,#26191,#26192,#26193,#26194,#26195,#26196,#26197,
#26198),.UNSPECIFIED.,.F.,.F.,(4,2,2,2,2,2,2,2,2,2,2,2,2,4),(6.03863816781982E-5,
0.0235321054586779,0.0469894124433013,0.0625955451438476,0.120830736051024,
0.148200482152788,0.177426809763754,0.234689944472845,0.262841817837877,
0.31782697095527,0.362416306428818,0.390301942764782,0.40453484142027,0.418742436141258),
 .UNSPECIFIED.);
#2222=B_SPLINE_CURVE_WITH_KNOTS('',3,(#26200,#26201,#26202,#26203,#26204,
#26205,#26206,#26207,#26208,#26209,#26210,#26211,#26212,#26213,#26214,#26215,
#26216,#26217,#26218,#26219,#26220,#26221,#26222,#26223,#26224,#26225,#26226,
#26227,#26228,#26229,#26230,#26231,#26232,#26233,#26234,#26235),
 .UNSPECIFIED.,.F.,.F.,(4,2,2,2,2,2,2,2,2,2,2,2,2,2,2,2,2,4),(-1.03451909507685,
-0.985628237457854,-0.936696563950415,-0.861017278353068,-0.772400298280665,
-0.674466741047526,-0.58240655627606,-0.502283935464647,-0.434648703401253,
-0.399451972244463,-0.330651356045544,-0.267309498328652,-0.211812516712395,
-0.183464606668581,-0.124444898378072,-0.0613612600492961,-0.0312461969758679,
-7.37969285442371E-5),.UNSPECIFIED.);
#2223=B_SPLINE_CURVE_WITH_KNOTS('',3,(#26518,#26519,#26520,#26521,#26522,
#26523,#26524,#26525,#26526,#26527,#26528,#26529,#26530,#26531,#26532,#26533,
#26534,#26535,#26536,#26537,#26538,#26539,#26540,#26541,#26542,#26543,#26544,
#26545,#26546,#26547,#26548,#26549,#26550,#26551,#26552,#26553,#26554,#26555,
#26556,#26557,#26558,#26559,#26560,#26561,#26562,#26563,#26564,#26565,#26566,
#26567,#26568,#26569,#26570,#26571,#26572,#26573,#26574,#26575,#26576,#26577,
#26578,#26579,#26580,#26581,#26582,#26583,#26584,#26585,#26586,#26587,#26588,
#26589,#26590,#26591,#26592,#26593,#26594,#26595,#26596,#26597,#26598,#26599,
#26600,#26601,#26602,#26603,#26604,#26605,#26606,#26607,#26608,#26609,#26610,
#26611,#26612,#26613,#26614,#26615,#26616,#26617,#26618,#26619,#26620,#26621,
#26622,#26623,#26624,#26625,#26626,#26627,#26628,#26629,#26630,#26631,#26632,
#26633,#26634,#26635,#26636,#26637,#26638,#26639,#26640,#26641,#26642,#26643,
#26644,#26645,#26646,#26647),.UNSPECIFIED.,.F.,.F.,(4,2,2,2,2,2,2,2,2,2,
2,2,2,2,2,2,2,2,2,2,2,2,2,2,2,2,2,2,2,2,2,2,2,2,2,2,2,2,2,2,2,2,2,2,2,2,
2,2,2,2,2,2,2,2,2,2,2,2,2,2,2,2,2,2,4),(4.96401988677343E-5,0.0286909851214567,
0.0556526802951698,0.113832141356971,0.161351607238736,0.218507559614986,
0.258398640746192,0.306095729471452,0.362010325096549,0.401932827379239,
0.449679229549262,0.506640699165884,0.546568564241865,0.594128809564416,
0.649775741136893,0.689741624015701,0.737661250020149,0.79515538238638,
0.835112826235051,0.882602298743163,0.937613137963498,0.977626467674421,
1.02576982630798,1.08415873336359,1.12414091063929,1.17148371887183,1.22517859760727,
1.26524992889356,1.31382300234001,1.37387784361501,1.41387374553324,1.46091668317935,
1.50925514688824,1.58269800618146,1.65896058403542,1.71319604759754,1.75314524331709,
1.79263146105731,1.83759108160969,1.90438845857931,1.96972763829277,2.01044088449258,
2.06296596817368,2.10925651439416,2.14980073822217,2.2105683732106,2.25789865056263,
2.29847153891689,2.35552271586138,2.40210594727478,2.44260893906244,2.50196302289595,
2.54893131404076,2.5894265700774,2.64731488333339,2.69394136940077,2.73438961727687,
2.79305667135409,2.83992515335308,2.88034576054228,2.93909733066414,2.98576859062926,
3.04660814582191,3.07498707993905,3.10514224167434),.UNSPECIFIED.);
#2224=B_SPLINE_CURVE_WITH_KNOTS('',3,(#26650,#26651,#26652,#26653,#26654,
#26655,#26656,#26657,#26658,#26659,#26660,#26661,#26662,#26663,#26664,#26665,
#26666,#26667,#26668,#26669,#26670,#26671,#26672,#26673,#26674,#26675,#26676,
#26677,#26678,#26679,#26680,#26681,#26682,#26683,#26684,#26685,#26686,#26687,
#26688,#26689,#26690,#26691,#26692,#26693,#26694,#26695,#26696,#26697,#26698,
#26699,#26700,#26701,#26702,#26703,#26704,#26705,#26706,#26707,#26708,#26709,
#26710,#26711,#26712,#26713,#26714,#26715,#26716,#26717,#26718,#26719,#26720,
#26721,#26722,#26723,#26724,#26725,#26726,#26727,#26728,#26729,#26730,#26731,
#26732,#26733,#26734,#26735,#26736,#26737,#26738,#26739,#26740,#26741,#26742,
#26743,#26744,#26745,#26746,#26747,#26748,#26749,#26750,#26751,#26752,#26753,
#26754,#26755,#26756,#26757,#26758,#26759,#26760,#26761,#26762,#26763,#26764,
#26765,#26766,#26767),.UNSPECIFIED.,.F.,.F.,(4,2,2,2,2,2,2,2,2,2,2,2,2,
2,2,2,2,2,2,2,2,2,2,2,2,2,2,2,2,2,2,2,2,2,2,2,2,2,2,2,2,2,2,2,2,2,2,2,2,
2,2,2,2,2,2,2,2,2,4),(-5.94661143749944,-5.91817587231828,-5.88954389637305,
-5.84610834802751,-5.79455901799797,-5.73536393690187,-5.65444785916197,
-5.54740153892753,-5.44330804223854,-5.35930759079344,-5.2847068935834,
-5.23034358179366,-5.18685935478129,-5.13256440156231,-5.06059686138459,
-4.97555958664179,-4.87811537048653,-4.74796036252415,-4.56674349897742,
-4.37418341756985,-4.2203094920287,-4.08357971751308,-3.98457995699775,
-3.90516656475212,-3.80969900284799,-3.69213562716397,-3.55391073228339,
-3.3958547797668,-3.20141104323893,-2.97334127066598,-2.74527149809304,
-2.55082776156515,-2.39277180904853,-2.25454691416793,-2.13698353848388,
-2.04151597657974,-1.9621025843341,-1.86310282381876,-1.7263730493031,-1.57249912376192,
-1.37993904235428,-1.19872217880751,-1.06856717084512,-0.971122954689846,
-0.886085679947027,-0.814118139769293,-0.759823186550277,-0.716338959537862,
-0.661975647748049,-0.587374950537876,-0.50337449909263,-0.399281002403463,
-0.29223468216884,-0.211318604428868,-0.152123523332738,-0.100574193303159,
-0.0571386449575849,-0.0285066862366441,-7.10380286812318E-5),
 .UNSPECIFIED.);
#2225=B_SPLINE_CURVE_WITH_KNOTS('',3,(#26910,#26911,#26912,#26913,#26914,
#26915,#26916,#26917,#26918,#26919,#26920,#26921,#26922,#26923,#26924,#26925,
#26926,#26927,#26928,#26929,#26930,#26931,#26932,#26933,#26934,#26935,#26936,
#26937,#26938,#26939,#26940,#26941,#26942,#26943,#26944,#26945,#26946,#26947,
#26948,#26949,#26950,#26951,#26952,#26953,#26954,#26955,#26956,#26957,#26958,
#26959,#26960,#26961,#26962,#26963,#26964,#26965,#26966,#26967,#26968,#26969,
#26970,#26971,#26972,#26973,#26974,#26975,#26976,#26977,#26978,#26979,#26980,
#26981,#26982,#26983,#26984,#26985,#26986,#26987,#26988,#26989,#26990,#26991,
#26992,#26993,#26994,#26995,#26996,#26997,#26998,#26999,#27000,#27001,#27002,
#27003,#27004,#27005,#27006,#27007,#27008,#27009,#27010,#27011,#27012,#27013,
#27014,#27015,#27016,#27017,#27018,#27019,#27020,#27021,#27022,#27023,#27024,
#27025,#27026,#27027),.UNSPECIFIED.,.F.,.F.,(4,2,2,2,2,2,2,2,2,2,2,2,2,
2,2,2,2,2,2,2,2,2,2,2,2,2,2,2,2,2,2,2,2,2,2,2,2,2,2,2,2,2,2,2,2,2,2,2,2,
2,2,2,2,2,2,2,2,2,4),(7.10380286801851E-5,0.0285066862366488,0.0571386449575934,
0.100574193303156,0.15212352333273,0.211318604428867,0.292234682168843,
0.399281002403465,0.503374499092633,0.587374950537879,0.661975647748052,
0.716338959537883,0.759823186550319,0.814118139769361,0.886085679947134,
0.971122954689997,1.06856717084532,1.19872217880778,1.37993904235465,1.5724991237624,
1.72637304930366,1.86310282381939,1.9621025843348,2.0415159765805,2.1369835384847,
2.25454691416883,2.39277180904952,2.55082776156624,2.74527149809426,2.97334127066737,
3.20141104324048,3.3958547797685,3.55391073228522,3.69213562716592,3.80969900285004,
3.90516656475422,3.98457995699989,4.08357971751527,4.22030949203095,4.37418341757216,
4.56674349897983,4.74796036252663,4.87811537048906,4.97555958664437,5.06059686138721,
5.13256440156495,5.18685935478398,5.2303435817964,5.28470689358622,5.35930759079635,
5.44330804224156,5.54740153893068,5.65444785916525,5.73536393690522,5.79455901800137,
5.84610834803096,5.88954389637653,5.9181758550974,5.94661148928436),
 .UNSPECIFIED.);
#2226=B_SPLINE_CURVE_WITH_KNOTS('',3,(#27170,#27171,#27172,#27173,#27174,
#27175,#27176,#27177,#27178,#27179,#27180,#27181,#27182,#27183,#27184,#27185,
#27186,#27187,#27188,#27189,#27190,#27191,#27192,#27193,#27194,#27195,#27196,
#27197,#27198,#27199,#27200,#27201,#27202,#27203,#27204,#27205,#27206,#27207,
#27208,#27209,#27210,#27211),.UNSPECIFIED.,.F.,.F.,(4,2,2,2,2,2,2,2,2,2,
2,2,2,2,2,2,2,2,2,2,4),(9.56954942354455E-5,0.0404351999983261,0.0809863391999001,
0.138729373521468,0.168045411658336,0.227812497843943,0.287843613795308,
0.346677944888803,0.375266460404388,0.434868243739065,0.464254106674541,
0.49301855332279,0.551407950994098,0.611332985371951,0.670401283775956,
0.729413371370902,0.788742981688662,0.817389185685092,0.875712032112295,
0.912199298092506,0.948381011938093),.UNSPECIFIED.);
#2227=B_SPLINE_CURVE_WITH_KNOTS('',3,(#27353,#27354,#27355,#27356,#27357,
#27358,#27359,#27360,#27361,#27362,#27363,#27364,#27365,#27366,#27367,#27368,
#27369,#27370,#27371,#27372,#27373,#27374,#27375,#27376,#27377,#27378,#27379,
#27380,#27381,#27382,#27383,#27384,#27385,#27386,#27387,#27388,#27389,#27390,
#27391,#27392,#27393,#27394,#27395,#27396,#27397,#27398,#27399,#27400,#27401,
#27402,#27403,#27404,#27405,#27406,#27407,#27408,#27409,#27410,#27411,#27412,
#27413,#27414,#27415,#27416,#27417,#27418,#27419,#27420,#27421,#27422,#27423,
#27424,#27425,#27426,#27427,#27428,#27429,#27430,#27431,#27432,#27433,#27434,
#27435,#27436,#27437,#27438,#27439,#27440,#27441,#27442,#27443,#27444,#27445,
#27446,#27447,#27448,#27449,#27450,#27451,#27452,#27453,#27454,#27455,#27456,
#27457,#27458,#27459,#27460,#27461,#27462,#27463,#27464,#27465,#27466,#27467,
#27468,#27469,#27470,#27471,#27472,#27473,#27474,#27475,#27476,#27477,#27478,
#27479,#27480,#27481,#27482),.UNSPECIFIED.,.F.,.F.,(4,2,2,2,2,2,2,2,2,2,
2,2,2,2,2,2,2,2,2,2,2,2,2,2,2,2,2,2,2,2,2,2,2,2,2,2,2,2,2,2,2,2,2,2,2,2,
2,2,2,2,2,2,2,2,2,2,2,2,2,2,2,2,2,2,4),(4.96401988677452E-5,0.0286909851214136,
0.0556526802950926,0.113832141356949,0.161351607239005,0.218507559615801,
0.258398640747191,0.306095729472568,0.362010325097728,0.40193282738061,
0.449679229551041,0.506640699167879,0.546568564244047,0.594128809566736,
0.64977574113961,0.6897416240186,0.737661250023257,0.795155382389599,0.835112826238453,
0.882602298746813,0.937613137967583,0.977626467678681,1.02576982631241,
1.08415873336806,1.12414091064394,1.17148371887674,1.22517859761275,1.26524992889922,
1.31382300234579,1.3738778436207,1.41387374553911,1.46091668318551,1.509255146879,
1.582698006183,1.65896058405076,1.71319604762296,1.75314524334271,1.79263146107175,
1.83759108162834,1.904388458596,1.96972763830814,2.01044088450079,2.06296596815001,
2.10925651435982,2.14980073818021,2.2105683731605,2.25789865050626,2.29847153885315,
2.35552271578088,2.40210594718442,2.44260893896451,2.50196302279135,2.54893131392834,
2.58942656995753,2.64731488319995,2.69394136925823,2.73438961712682,2.79305667119477,
2.83992515318539,2.88034576036712,2.93909733047707,2.98576859043333,3.04660814561508,
3.07498707972723,3.10514224145725),.UNSPECIFIED.);
#2228=B_SPLINE_CURVE_WITH_KNOTS('',3,(#27485,#27486,#27487,#27488,#27489,
#27490,#27491,#27492,#27493,#27494,#27495,#27496,#27497,#27498,#27499,#27500,
#27501,#27502,#27503,#27504,#27505,#27506,#27507,#27508,#27509,#27510,#27511,
#27512,#27513,#27514,#27515,#27516,#27517,#27518,#27519,#27520,#27521,#27522,
#27523,#27524,#27525,#27526,#27527,#27528,#27529,#27530,#27531,#27532,#27533,
#27534,#27535,#27536,#27537,#27538,#27539,#27540,#27541,#27542,#27543,#27544,
#27545,#27546,#27547,#27548,#27549,#27550,#27551,#27552,#27553,#27554,#27555,
#27556,#27557,#27558,#27559,#27560,#27561,#27562,#27563,#27564,#27565,#27566,
#27567,#27568,#27569,#27570,#27571,#27572,#27573,#27574,#27575,#27576,#27577,
#27578,#27579,#27580,#27581,#27582,#27583,#27584,#27585,#27586,#27587,#27588,
#27589,#27590,#27591,#27592,#27593,#27594,#27595,#27596,#27597,#27598,#27599,
#27600,#27601,#27602),.UNSPECIFIED.,.F.,.F.,(4,2,2,2,2,2,2,2,2,2,2,2,2,
2,2,2,2,2,2,2,2,2,2,2,2,2,2,2,2,2,2,2,2,2,2,2,2,2,2,2,2,2,2,2,2,2,2,2,2,
2,2,2,2,2,2,2,2,2,4),(-5.9466114892713,-5.91817585508441,-5.88954389636361,
-5.84610834801816,-5.79455901798872,-5.73536393689273,-5.65444785915298,
-5.54740153891873,-5.44330804222993,-5.35930759078498,-5.28470689357507,
-5.23034358178543,-5.18685935477315,-5.13256440155427,-5.06059686137668,
-4.97555958663403,-4.87811537047895,-4.74796036251681,-4.56674349897041,
-4.37418341756319,-4.22030949202233,-4.08357971750696,-3.9845799569918,
-3.90516656474632,-3.80969900284236,-3.69213562715855,-3.55391073227822,
-3.39585477976192,-3.20141104323441,-2.97334127066188,-2.74527149808934,
-2.5508277615618,-2.39277180904547,-2.25454691416512,-2.13698353848128,
-2.04151597657729,-1.96210258433177,-1.86310282381656,-1.72637304930109,
-1.57249912376012,-1.37993904235275,-1.19872217880622,-1.06856717084401,
-0.971122954688863,-0.886085679946156,-0.814118139768516,-0.759823186549577,
-0.716338959537225,-0.661975647747492,-0.587374950537428,-0.503374499092306,
-0.399281002403298,-0.292234682168818,-0.211318604428862,-0.152123523332728,
-0.100574193303159,-0.0571386449575935,-0.0285066862366491,-7.10380286809763E-5),
 .UNSPECIFIED.);
#2229=B_SPLINE_CURVE_WITH_KNOTS('',3,(#27745,#27746,#27747,#27748,#27749,
#27750,#27751,#27752,#27753,#27754,#27755,#27756,#27757,#27758,#27759,#27760,
#27761,#27762,#27763,#27764,#27765,#27766,#27767,#27768,#27769,#27770,#27771,
#27772,#27773,#27774,#27775,#27776,#27777,#27778,#27779,#27780,#27781,#27782,
#27783,#27784,#27785,#27786,#27787,#27788,#27789,#27790,#27791,#27792,#27793,
#27794,#27795,#27796,#27797,#27798,#27799,#27800,#27801,#27802,#27803,#27804,
#27805,#27806,#27807,#27808,#27809,#27810,#27811,#27812,#27813,#27814,#27815,
#27816,#27817,#27818,#27819,#27820,#27821,#27822,#27823,#27824,#27825,#27826,
#27827,#27828,#27829,#27830,#27831,#27832,#27833,#27834,#27835,#27836,#27837,
#27838,#27839,#27840,#27841,#27842,#27843,#27844,#27845,#27846,#27847,#27848,
#27849,#27850,#27851,#27852,#27853,#27854,#27855,#27856,#27857,#27858,#27859,
#27860,#27861,#27862),.UNSPECIFIED.,.F.,.F.,(4,2,2,2,2,2,2,2,2,2,2,2,2,
2,2,2,2,2,2,2,2,2,2,2,2,2,2,2,2,2,2,2,2,2,2,2,2,2,2,2,2,2,2,2,2,2,2,2,2,
2,2,2,2,2,2,2,2,2,4),(7.1038028680126E-5,0.0285066862366493,0.0571386449575946,
0.100574193303158,0.152123523332732,0.21131860442887,0.292234682168858,
0.399281002403533,0.503374499092753,0.587374950538041,0.661975647748252,
0.716338959538097,0.75982318655054,0.814118139769595,0.886085679947392,
0.971122954690285,1.06856717084564,1.19872217880814,1.37993904235504,1.57249912376282,
1.72637304930411,1.86310282381987,1.9621025843353,2.04151597658101,2.13698353848521,
2.25454691416929,2.39277180904992,2.55082776156657,2.7452714980945,2.97334127066752,
3.20141104324053,3.39585477976846,3.55391073228511,3.69213562716574,3.80969900284981,
3.90516656475396,3.9845799569996,4.08357971751495,4.22030949203059,4.37418341757175,
4.56674349897935,4.74796036252611,4.87811537048849,4.97555958664375,5.06059686138656,
5.13256440156429,5.18685935478327,5.23034358179564,5.28470689358539,5.35930759079546,
5.44330804224058,5.54740153892958,5.65444785916408,5.73536393690415,5.7945590180004,
5.84610834803006,5.8895438963757,5.91817585509662,5.94661148928363),
 .UNSPECIFIED.);
#2230=B_SPLINE_CURVE_WITH_KNOTS('',3,(#28005,#28006,#28007,#28008,#28009,
#28010,#28011,#28012,#28013,#28014,#28015,#28016,#28017,#28018,#28019,#28020,
#28021,#28022,#28023,#28024,#28025,#28026,#28027,#28028,#28029,#28030,#28031,
#28032,#28033,#28034,#28035,#28036,#28037,#28038,#28039,#28040,#28041,#28042,
#28043,#28044,#28045,#28046),.UNSPECIFIED.,.F.,.F.,(4,2,2,2,2,2,2,2,2,2,
2,2,2,2,2,2,2,2,2,2,4),(4.96665808836377E-5,0.0404121485248788,0.0809389875253708,
0.138678740779869,0.167993113958696,0.227756805017511,0.287784512376069,
0.34661550188191,0.3752023945415,0.434800793278714,0.464184987531579,0.492947800522654,
0.551333883846547,0.611255516075695,0.670320462148153,0.729329203272392,
0.788655454004735,0.817300035390535,0.875619579999266,0.912104776589651,
0.948284438308318),.UNSPECIFIED.);
#2231=B_SPLINE_CURVE_WITH_KNOTS('',3,(#28188,#28189,#28190,#28191,#28192,
#28193,#28194,#28195,#28196,#28197,#28198,#28199,#28200,#28201,#28202,#28203,
#28204,#28205,#28206,#28207,#28208,#28209,#28210,#28211,#28212,#28213,#28214,
#28215,#28216,#28217,#28218,#28219,#28220,#28221,#28222,#28223,#28224,#28225,
#28226,#28227,#28228,#28229,#28230,#28231,#28232,#28233,#28234,#28235,#28236,
#28237,#28238,#28239,#28240,#28241,#28242,#28243,#28244,#28245,#28246,#28247,
#28248,#28249,#28250,#28251,#28252,#28253,#28254,#28255,#28256,#28257,#28258,
#28259,#28260,#28261,#28262,#28263,#28264,#28265,#28266,#28267,#28268,#28269,
#28270,#28271,#28272,#28273,#28274,#28275,#28276,#28277,#28278,#28279,#28280,
#28281,#28282,#28283,#28284,#28285,#28286,#28287,#28288,#28289,#28290,#28291,
#28292,#28293,#28294,#28295,#28296,#28297,#28298,#28299,#28300,#28301,#28302,
#28303),.UNSPECIFIED.,.F.,.F.,(4,2,2,2,2,2,2,2,2,2,2,2,2,2,2,2,2,2,2,2,
2,2,2,2,2,2,2,2,2,2,2,2,2,2,2,2,2,2,2,2,2,2,2,2,2,2,2,2,2,2,2,2,2,2,2,2,
2,4),(9.57215647317225E-5,0.028805838183546,0.0558568013553045,0.114080987998557,
0.161249463922362,0.217422313166586,0.257152574756385,0.304825366934254,
0.361477483325091,0.401213970266859,0.448514553663052,0.503904602332678,
0.543680699307756,0.591367734962095,0.648551016184757,0.688318941212196,
0.735595502996825,0.790419031076046,0.830240895728071,0.878133663029185,
0.936150773297636,0.97594415736791,1.02308308630774,1.07668824732422,1.11656640699563,
1.16485993428889,1.22443813629381,1.29181371179871,1.36063223184655,1.41041636122522,
1.45043902605067,1.49894607576938,1.54456678430888,1.58437861540954,1.64336805299861,
1.68967717074328,1.72949835552286,1.78598579990277,1.8317887234759,1.87155356665554,
1.92955337883068,1.97560054878039,2.01534998788364,2.07236198886952,2.11819652479389,
2.15790547535948,2.21546473932318,2.26137161495789,2.30105577117442,2.35820280734624,
2.40400591908383,2.44365534073145,2.50099895654661,2.54681681861997,2.58643864421989,
2.64357124839567,2.6892861687949,2.74198047995337),.UNSPECIFIED.);
#2232=B_SPLINE_CURVE_WITH_KNOTS('',3,(#28305,#28306,#28307,#28308),
 .UNSPECIFIED.,.F.,.F.,(4,4),(0.,0.0129000141117776),.UNSPECIFIED.);
#2233=B_SPLINE_CURVE_WITH_KNOTS('',3,(#28310,#28311,#28312,#28313,#28314,
#28315,#28316,#28317,#28318,#28319,#28320,#28321,#28322,#28323),
 .UNSPECIFIED.,.F.,.F.,(4,2,2,2,2,2,4),(6.18255457422751E-5,0.0445222550398773,
0.0815855333793703,0.138348319078884,0.188225454345152,0.235381542690196,
0.275928945498945),.UNSPECIFIED.);
#2234=B_SPLINE_CURVE_WITH_KNOTS('',3,(#28325,#28326,#28327,#28328,#28329,
#28330),.UNSPECIFIED.,.F.,.F.,(4,2,4),(-0.0363675439270173,-0.0181932738790337,
-8.99968048774418E-6),.UNSPECIFIED.);
#2235=B_SPLINE_CURVE_WITH_KNOTS('',3,(#28331,#28332,#28333,#28334,#28335,
#28336,#28337,#28338,#28339,#28340,#28341,#28342,#28343,#28344,#28345,#28346,
#28347,#28348,#28349,#28350,#28351,#28352,#28353,#28354,#28355,#28356,#28357,
#28358,#28359,#28360,#28361,#28362,#28363,#28364,#28365,#28366,#28367,#28368,
#28369,#28370,#28371,#28372,#28373,#28374,#28375,#28376,#28377,#28378,#28379,
#28380,#28381,#28382,#28383,#28384,#28385,#28386,#28387,#28388,#28389,#28390,
#28391,#28392,#28393,#28394,#28395,#28396,#28397,#28398,#28399,#28400,#28401,
#28402,#28403,#28404,#28405,#28406,#28407,#28408,#28409,#28410,#28411,#28412,
#28413,#28414,#28415,#28416,#28417,#28418,#28419,#28420,#28421,#28422,#28423,
#28424,#28425,#28426,#28427,#28428,#28429,#28430,#28431,#28432,#28433,#28434,
#28435,#28436,#28437,#28438,#28439,#28440,#28441,#28442,#28443,#28444,#28445,
#28446,#28447,#28448),.UNSPECIFIED.,.F.,.F.,(4,2,2,2,2,2,2,2,2,2,2,2,2,
2,2,2,2,2,2,2,2,2,2,2,2,2,2,2,2,2,2,2,2,2,2,2,2,2,2,2,2,2,2,2,2,2,2,2,2,
2,2,2,2,2,2,2,2,2,4),(-5.94660785390406,-5.91817223520138,-5.8895402920717,
-5.84610476737843,-5.79455546541942,-5.73536041655725,-5.65444438287918,
-5.5473981209355,-5.44330468092936,-5.35930427522568,-5.28470361863854,
-5.23034033645167,-5.18685613311811,-5.1325612094648,-5.06059370847615,
-4.97555648003939,-4.87811231694623,-4.74795737985823,-4.56674061499099,
-4.37418063843972,-4.2203067966888,-4.08357709662776,-3.98457739002157,
-3.90516404101956,-3.80969653110115,-3.69213321943482,-3.55390839982292,
-3.39585253337379,-3.2014089027279,-2.97333925434758,-2.74526960596726,
-2.55082597532136,-2.3927701088722,-2.2545452892603,-2.13698197759396,-2.04151446767552,
-1.96210111867348,-1.86310141206725,-1.72637171200613,-1.57249787025512,
-1.37993789370372,-1.1987211288364,-1.06856619174833,-0.971122028655101,
-0.886084800218291,-0.814117299229607,-0.759822375576234,-0.71633817224261,
-0.661974890055658,-0.587374233468364,-0.503373827764516,-0.399280387758161,
-0.292234125814284,-0.211318092136195,-0.152123043274046,-0.100573741315045,
-0.0571382166217848,-0.0285064768322595,-7.04304336443412E-5),
 .UNSPECIFIED.);
#2236=B_SPLINE_CURVE_WITH_KNOTS('',3,(#28591,#28592,#28593,#28594,#28595,
#28596,#28597,#28598,#28599,#28600),.UNSPECIFIED.,.F.,.F.,(4,2,2,2,4),(-0.148755444895566,
-0.114171890294938,-0.0747141917985825,-0.0422804484276971,-4.41324122456156E-5),
 .UNSPECIFIED.);
#2237=B_SPLINE_CURVE_WITH_KNOTS('',3,(#28601,#28602,#28603,#28604),
 .UNSPECIFIED.,.F.,.F.,(4,4),(-0.00253843258531285,0.),.UNSPECIFIED.);
#2238=B_SPLINE_CURVE_WITH_KNOTS('',3,(#28605,#28606,#28607,#28608,#28609,
#28610,#28611,#28612,#28613,#28614,#28615,#28616,#28617,#28618,#28619,#28620,
#28621,#28622,#28623,#28624,#28625,#28626,#28627,#28628,#28629,#28630,#28631,
#28632,#28633,#28634,#28635,#28636,#28637,#28638),.UNSPECIFIED.,.F.,.F.,
(4,2,2,2,2,2,2,2,2,2,2,2,2,2,2,2,4),(-0.724835095226849,-0.684778550647567,
-0.631527667737965,-0.579128159920059,-0.525654533425143,-0.499826397983904,
-0.443357906433312,-0.417075199883106,-0.362131833684399,-0.306553522094715,
-0.279403621248859,-0.221291231076379,-0.170661187182406,-0.111573179077511,
-0.0622487991085858,-0.031596946474214,-2.64178122616785E-5),
 .UNSPECIFIED.);
#2239=B_SPLINE_CURVE_WITH_KNOTS('',3,(#28640,#28641,#28642,#28643,#28644,
#28645,#28646,#28647,#28648,#28649,#28650,#28651,#28652,#28653,#28654,#28655,
#28656,#28657,#28658,#28659,#28660,#28661,#28662,#28663,#28664,#28665,#28666,
#28667,#28668,#28669,#28670,#28671,#28672,#28673,#28674,#28675,#28676,#28677,
#28678,#28679,#28680,#28681,#28682,#28683,#28684,#28685,#28686,#28687,#28688,
#28689,#28690,#28691,#28692,#28693,#28694,#28695,#28696,#28697,#28698,#28699,
#28700,#28701,#28702,#28703,#28704,#28705,#28706,#28707,#28708,#28709,#28710,
#28711,#28712,#28713,#28714,#28715,#28716,#28717,#28718,#28719,#28720,#28721,
#28722,#28723,#28724,#28725,#28726,#28727,#28728,#28729,#28730,#28731,#28732,
#28733,#28734,#28735,#28736,#28737,#28738,#28739,#28740,#28741,#28742,#28743,
#28744,#28745,#28746,#28747,#28748,#28749,#28750,#28751,#28752,#28753,#28754,
#28755,#28756,#28757),.UNSPECIFIED.,.F.,.F.,(4,2,2,2,2,2,2,2,2,2,2,2,2,
2,2,2,2,2,2,2,2,2,2,2,2,2,2,2,2,2,2,2,2,2,2,2,2,2,2,2,2,2,2,2,2,2,2,2,2,
2,2,2,2,2,2,2,2,2,4),(7.10380286804536E-5,0.0285066862366494,0.0571386449575948,
0.100574193303159,0.152123523332733,0.21131860442887,0.292234682168856,
0.399281002403517,0.503374499092718,0.58737495053799,0.661975647748188,
0.716338959538033,0.75982318655048,0.814118139769539,0.88608567994734,0.971122954690238,
1.0685671708456,1.19872217880811,1.37993904235503,1.57249912376283,1.72637304930414,
1.8631028238199,1.96210258433533,2.04151597658104,2.13698353848524,2.25454691416934,
2.39277180905,2.55082776156668,2.74527149809465,2.97334127066772,3.20141104324078,
3.39585477976875,3.55391073228543,3.69213562716609,3.80969900285018,3.90516656475433,
3.98457995699997,4.08357971751531,4.22030949203093,4.37418341757207,4.56674349897965,
4.74796036252637,4.87811537048874,4.975559586644,5.0605968613868,5.13256440156451,
5.18685935478351,5.23034358179591,5.28470689358571,5.35930759079585,5.44330804224105,
5.54740153893017,5.65444785916474,5.73536393690472,5.79455901800088,5.84610834803048,
5.88954389637607,5.91817569303648,5.94661170936932),.UNSPECIFIED.);
#2240=B_SPLINE_CURVE_WITH_KNOTS('',3,(#28758,#28759,#28760,#28761,#28762,
#28763),.UNSPECIFIED.,.F.,.F.,(4,2,4),(-0.0225817708757373,-0.0112843508253838,
-2.98243785195915E-5),.UNSPECIFIED.);
#2241=B_SPLINE_CURVE_WITH_KNOTS('',3,(#28774,#28775,#28776,#28777,#28778,
#28779),.UNSPECIFIED.,.F.,.F.,(4,2,4),(-0.00584242467456242,-0.00295752748558409,
-6.89218742153712E-5),.UNSPECIFIED.);
#2242=B_SPLINE_CURVE_WITH_KNOTS('',3,(#28958,#28959,#28960,#28961,#28962,
#28963),.UNSPECIFIED.,.F.,.F.,(4,2,4),(0.716974528647988,0.741226803621157,
0.765479078593388),.UNSPECIFIED.);
#2243=B_SPLINE_CURVE_WITH_KNOTS('',3,(#28965,#28966,#28967,#28968,#28969,
#28970,#28971,#28972,#28973,#28974,#28975,#28976,#28977,#28978,#28979),
 .UNSPECIFIED.,.F.,.F.,(4,3,2,2,2,2,4),(-0.00535406387047143,0.,0.00280519627261519,
0.0127729727608755,0.022681421764352,0.0323964936700699,0.0339100227105242),
 .UNSPECIFIED.);
#2244=B_SPLINE_CURVE_WITH_KNOTS('',3,(#28981,#28982,#28983,#28984),
 .UNSPECIFIED.,.F.,.F.,(4,4),(-0.907105856924628,-0.889730448331648),
 .UNSPECIFIED.);
#2245=B_SPLINE_CURVE_WITH_KNOTS('',3,(#28988,#28989,#28990,#28991),
 .UNSPECIFIED.,.F.,.F.,(4,4),(-0.70632843047102,-0.688953021878057),
 .UNSPECIFIED.);
#2246=B_SPLINE_CURVE_WITH_KNOTS('',3,(#28993,#28994,#28995,#28996,#28997,
#28998,#28999,#29000,#29001,#29002,#29003,#29004,#29005,#29006,#29007),
 .UNSPECIFIED.,.F.,.F.,(4,2,2,2,3,2,4),(-0.0339185312885629,-0.0292377700958602,
-0.0195230415801756,-0.00979953953065908,0.,0.00316958312039792,0.00534140243914174),
 .UNSPECIFIED.);
#2247=B_SPLINE_CURVE_WITH_KNOTS('',3,(#29016,#29017,#29018,#29019,#29020,
#29021,#29022,#29023,#29024,#29025,#29026,#29027,#29028,#29029,#29030),
 .UNSPECIFIED.,.F.,.F.,(4,3,2,2,2,2,4),(-0.00535406387034717,0.,0.00280519627249134,
0.0127729727607225,0.0226814217641763,0.0323964936698689,0.0339100227105453),
 .UNSPECIFIED.);
#2248=B_SPLINE_CURVE_WITH_KNOTS('',3,(#29032,#29033,#29034,#29035),
 .UNSPECIFIED.,.F.,.F.,(4,4),(-0.907105856925505,-0.889730448332538),
 .UNSPECIFIED.);
#2249=B_SPLINE_CURVE_WITH_KNOTS('',3,(#29039,#29040,#29041,#29042),
 .UNSPECIFIED.,.F.,.F.,(4,4),(-0.706328430471259,-0.688953021878271),
 .UNSPECIFIED.);
#2250=B_SPLINE_CURVE_WITH_KNOTS('',3,(#29044,#29045,#29046,#29047,#29048,
#29049,#29050,#29051,#29052,#29053,#29054,#29055,#29056,#29057,#29058),
 .UNSPECIFIED.,.F.,.F.,(4,2,2,2,3,2,4),(-0.0339185312884587,-0.0292377700958738,
-0.0195230415801824,-0.00979953953066153,0.,0.00316958312052598,0.00534140243929431),
 .UNSPECIFIED.);
#2251=B_SPLINE_CURVE_WITH_KNOTS('',3,(#29060,#29061,#29062,#29063,#29064,
#29065),.UNSPECIFIED.,.F.,.F.,(4,2,4),(-0.765479078594523,-0.74122680362135,
-0.716974528649115),.UNSPECIFIED.);
#2252=B_SPLINE_CURVE_WITH_KNOTS('',3,(#29067,#29068,#29069,#29070,#29071,
#29072,#29073,#29074,#29075,#29076,#29077,#29078,#29079,#29080,#29081),
 .UNSPECIFIED.,.F.,.F.,(4,3,2,2,2,2,4),(-0.0053540638702789,0.,0.00280519627268264,
0.0127729727609155,0.0226814217643626,0.0323964936700513,0.0339100227106541),
 .UNSPECIFIED.);
#2253=B_SPLINE_CURVE_WITH_KNOTS('',3,(#29083,#29084,#29085,#29086),
 .UNSPECIFIED.,.F.,.F.,(4,4),(0.688953021878874,0.706328430471897),
 .UNSPECIFIED.);
#2254=B_SPLINE_CURVE_WITH_KNOTS('',3,(#29090,#29091,#29092,#29093),
 .UNSPECIFIED.,.F.,.F.,(4,4),(-0.706328430472139,-0.688953021879099),
 .UNSPECIFIED.);
#2255=B_SPLINE_CURVE_WITH_KNOTS('',3,(#29095,#29096,#29097,#29098,#29099,
#29100,#29101,#29102,#29103,#29104,#29105,#29106,#29107,#29108,#29109),
 .UNSPECIFIED.,.F.,.F.,(4,2,2,2,3,2,4),(-0.0339185312885506,-0.0292377700958903,
-0.0195230415801947,-0.00979953953066585,0.,0.00316958312070759,0.00534140243922694),
 .UNSPECIFIED.);
#2256=B_SPLINE_CURVE_WITH_KNOTS('',3,(#29113,#29114,#29115,#29116,#29117,
#29118,#29119,#29120,#29121,#29122,#29123,#29124,#29125,#29126,#29127),
 .UNSPECIFIED.,.F.,.F.,(4,3,2,2,2,2,4),(-0.00535406387039295,0.,0.00280519627280415,
0.0127729727610477,0.0226814217644997,0.0323964936701972,0.0339100227105755),
 .UNSPECIFIED.);
#2257=B_SPLINE_CURVE_WITH_KNOTS('',3,(#29129,#29130,#29131,#29132),
 .UNSPECIFIED.,.F.,.F.,(4,4),(-0.907105856924454,-0.889730448331417),
 .UNSPECIFIED.);
#2258=B_SPLINE_CURVE_WITH_KNOTS('',3,(#29136,#29137,#29138,#29139),
 .UNSPECIFIED.,.F.,.F.,(4,4),(-0.706328430471901,-0.688953021878885),
 .UNSPECIFIED.);
#2259=B_SPLINE_CURVE_WITH_KNOTS('',3,(#29140,#29141,#29142,#29143,#29144,
#29145,#29146,#29147,#29148,#29149,#29150,#29151,#29152,#29153,#29154),
 .UNSPECIFIED.,.F.,.F.,(4,2,2,2,3,2,4),(-0.0339185312886601,-0.0292377700958805,
-0.0195230415801892,-0.00979953953066422,0.,0.00316958312058088,0.00534140243907669),
 .UNSPECIFIED.);
#2260=B_SPLINE_CURVE_WITH_KNOTS('',3,(#29282,#29283,#29284,#29285,#29286,
#29287,#29288,#29289,#29290,#29291,#29292,#29293,#29294,#29295,#29296,#29297,
#29298,#29299,#29300,#29301,#29302,#29303,#29304,#29305,#29306,#29307,#29308,
#29309,#29310,#29311,#29312),.UNSPECIFIED.,.F.,.F.,(4,3,3,3,3,3,3,3,3,3,
4),(5.17641734719844E-7,0.14139019525698,0.25,0.358065836273581,0.426319266401807,
0.5,0.614905428338237,0.713376508714083,0.75,0.93244192277557,1.),
 .UNSPECIFIED.);
#2261=B_SPLINE_CURVE_WITH_KNOTS('',3,(#29316,#29317,#29318,#29319,#29320,
#29321,#29322,#29323,#29324,#29325,#29326,#29327,#29328,#29329,#29330,#29331,
#29332,#29333,#29334,#29335,#29336,#29337,#29338,#29339,#29340,#29341,#29342,
#29343,#29344,#29345,#29346,#29347,#29348,#29349),.UNSPECIFIED.,.F.,.F.,
(4,3,3,3,3,3,3,3,3,3,3,4),(0.,0.128147294183543,0.25,0.279011458040339,
0.376318535302566,0.47243392503047,0.5,0.557339358509396,0.736991852961168,
0.75,0.835809619334612,1.),.UNSPECIFIED.);
#2262=B_SPLINE_CURVE_WITH_KNOTS('',3,(#29353,#29354,#29355,#29356,#29357,
#29358,#29359,#29360),.UNSPECIFIED.,.F.,.F.,(4,1,1,1,1,4),(0.,0.2,0.4,0.6,
0.8,0.999996095345817),.UNSPECIFIED.);
#2263=B_SPLINE_CURVE_WITH_KNOTS('',3,(#29364,#29365,#29366,#29367,#29368,
#29369),.UNSPECIFIED.,.F.,.F.,(4,1,1,4),(0.,0.3333333333333,0.6666666666667,
1.),.UNSPECIFIED.);
#2264=B_SPLINE_CURVE_WITH_KNOTS('',3,(#29371,#29372,#29373,#29374,#29375,
#29376),.UNSPECIFIED.,.F.,.F.,(4,1,1,4),(0.,0.3333333333333,0.6666666666667,
1.),.UNSPECIFIED.);
#2265=B_SPLINE_CURVE_WITH_KNOTS('',3,(#29379,#29380,#29381,#29382,#29383,
#29384,#29385),.UNSPECIFIED.,.F.,.F.,(4,1,1,1,4),(1.0492165877707E-5,0.25,
0.5,0.75,1.),.UNSPECIFIED.);
#2266=B_SPLINE_CURVE_WITH_KNOTS('',3,(#29468,#29469,#29470,#29471,#29472,
#29473,#29474,#29475,#29476,#29477,#29478,#29479,#29480,#29481,#29482,#29483,
#29484,#29485,#29486,#29487,#29488,#29489,#29490,#29491,#29492,#29493,#29494,
#29495,#29496,#29497,#29498,#29499,#29500,#29501,#29502,#29503,#29504),
 .UNSPECIFIED.,.F.,.F.,(4,3,3,3,3,3,3,3,3,3,3,3,4),(0.,0.1666666666667,
0.317615628299898,0.3333333333333,0.5,0.621047457925827,0.6666666666667,
0.768173703229194,0.8333333333333,0.833338977671904,0.909209388752102,0.977689001959099,
1.),.UNSPECIFIED.);
#2267=B_SPLINE_CURVE_WITH_KNOTS('',3,(#29506,#29507,#29508,#29509,#29510,
#29511,#29512,#29513,#29514),.UNSPECIFIED.,.F.,.F.,(4,1,1,1,1,1,4),(0.,
0.1666666666667,0.3333333333333,0.5,0.6666666666667,0.8333333333333,1.),
 .UNSPECIFIED.);
#2268=B_SPLINE_CURVE_WITH_KNOTS('',3,(#29559,#29560,#29561,#29562,#29563,
#29564,#29565,#29566,#29567,#29568,#29569,#29570,#29571,#29572,#29573,#29574,
#29575,#29576,#29577,#29578,#29579,#29580,#29581,#29582,#29583,#29584,#29585,
#29586,#29587,#29588,#29589),.UNSPECIFIED.,.F.,.F.,(4,3,3,3,3,3,3,3,3,3,
4),(1.57239443157975E-10,2.54069330995437E-6,0.15920203487198,0.25,0.376732535787111,
0.5,0.617341130244543,0.727443674691681,0.75,0.883645545754053,1.),
 .UNSPECIFIED.);
#2269=B_SPLINE_CURVE_WITH_KNOTS('',3,(#29591,#29592,#29593,#29594,#29595,
#29596,#29597,#29598,#29599,#29600,#29601,#29602,#29603,#29604,#29605,#29606,
#29607,#29608,#29609,#29610,#29611,#29612,#29613,#29614,#29615,#29616,#29617,
#29618,#29619,#29620,#29621),.UNSPECIFIED.,.F.,.F.,(4,3,3,3,3,3,3,3,3,3,
4),(3.44246750622568E-7,0.142587328061966,0.25,0.357451835441428,0.461548389909148,
0.5,0.597060204860859,0.688202468765424,0.75,0.874999999835037,0.999999999670074),
 .UNSPECIFIED.);
#2270=B_SPLINE_CURVE_WITH_KNOTS('',3,(#29704,#29705,#29706,#29707,#29708,
#29709,#29710,#29711,#29712,#29713,#29714,#29715,#29716,#29717,#29718,#29719,
#29720,#29721,#29722,#29723,#29724,#29725,#29726,#29727,#29728,#29729,#29730,
#29731,#29732,#29733,#29734,#29735,#29736,#29737),.UNSPECIFIED.,.F.,.F.,
(4,3,3,3,3,3,3,3,3,3,3,4),(5.14909641649198E-7,0.142170359375927,0.149743956654906,
0.25,0.357544559632778,0.431986036232602,0.5,0.614360513761462,0.716215156847761,
0.75,0.931218230535921,1.),.UNSPECIFIED.);
#2271=B_SPLINE_CURVE_WITH_KNOTS('',3,(#29740,#29741,#29742,#29743,#29744,
#29745,#29746,#29747,#29748,#29749,#29750,#29751,#29752,#29753,#29754,#29755,
#29756,#29757,#29758),.UNSPECIFIED.,.F.,.F.,(4,3,3,3,3,3,4),(1.66946584494145E-6,
0.1666666666667,0.3333333333333,0.5,0.6666666666667,0.8333333333333,1.),
 .UNSPECIFIED.);
#2272=B_SPLINE_CURVE_WITH_KNOTS('',3,(#29762,#29763,#29764,#29765,#29766,
#29767,#29768,#29769,#29770,#29771,#29772,#29773,#29774,#29775,#29776,#29777,
#29778,#29779,#29780,#29781,#29782,#29783,#29784,#29785,#29786,#29787,#29788,
#29789,#29790,#29791,#29792,#29793,#29794,#29795),.UNSPECIFIED.,.F.,.F.,
(4,3,3,3,3,3,3,3,3,3,3,4),(0.,0.128038283757864,0.25,0.277400491536672,
0.374623655828288,0.47065024139002,0.5,0.554195902331565,0.734425066600767,
0.75,0.831053386463994,1.),.UNSPECIFIED.);
#2273=B_SPLINE_CURVE_WITH_KNOTS('',3,(#29803,#29804,#29805,#29806,#29807,
#29808),.UNSPECIFIED.,.F.,.F.,(4,1,1,4),(0.,0.3333333333333,0.6666666666667,
1.),.UNSPECIFIED.);
#2274=B_SPLINE_CURVE_WITH_KNOTS('',3,(#29809,#29810,#29811,#29812,#29813,
#29814),.UNSPECIFIED.,.F.,.F.,(4,1,1,4),(0.,0.3333333333333,0.6666666666667,
1.),.UNSPECIFIED.);
#2275=B_SPLINE_CURVE_WITH_KNOTS('',3,(#29859,#29860,#29861,#29862,#29863,
#29864,#29865,#29866,#29867,#29868,#29869,#29870,#29871,#29872,#29873,#29874,
#29875,#29876,#29877,#29878,#29879,#29880,#29881,#29882,#29883,#29884,#29885,
#29886,#29887,#29888,#29889,#29890,#29891,#29892,#29893,#29894,#29895,#29896,
#29897,#29898,#29899,#29900,#29901,#29902,#29903,#29904),.UNSPECIFIED.,
 .F.,.F.,(4,3,3,3,3,3,3,3,3,3,3,3,3,3,3,4),(8.27094905990464E-7,3.66882272956542E-6,
0.0936078800827675,0.1666666666667,0.166676616624577,0.262875045155572,
0.3333333333333,0.4504794091647,0.499997157412759,0.5,0.610602034441991,
0.6666666666667,0.794049388469593,0.8333333333333,0.974910700247656,1.),
 .UNSPECIFIED.);
#2276=B_SPLINE_CURVE_WITH_KNOTS('',3,(#29935,#29936,#29937,#29938,#29939,
#29940),.UNSPECIFIED.,.F.,.F.,(4,1,1,4),(0.,0.3333333333333,0.6666666666667,
1.),.UNSPECIFIED.);
#2277=B_SPLINE_CURVE_WITH_KNOTS('',3,(#29944,#29945,#29946,#29947,#29948,
#29949,#29950,#29951,#29952,#29953,#29954,#29955,#29956,#29957,#29958,#29959,
#29960,#29961,#29962,#29963,#29964,#29965,#29966,#29967,#29968,#29969,#29970,
#29971,#29972,#29973,#29974,#29975,#29976,#29977,#29978,#29979,#29980,#29981,
#29982,#29983,#29984,#29985,#29986,#29987,#29988,#29989,#29990,#29991,#29992,
#29993,#29994,#29995,#29996,#29997,#29998,#29999,#30000,#30001,#30002,#30003,
#30004),.UNSPECIFIED.,.F.,.F.,(4,3,3,3,3,3,3,3,3,3,3,3,3,3,3,3,3,3,3,3,
4),(7.22383553753882E-7,0.07142857142857,0.130487248165375,0.1428571428571,
0.2142857142857,0.2857142857143,0.3571428571429,0.4285714285714,0.5,0.5714285714286,
0.6428571428571,0.704095964850392,0.7142857142857,0.771286832638653,0.7857142857143,
0.849372160563138,0.8571428571429,0.917671280130346,0.9285714285714,0.994058581712345,
0.999999942257354),.UNSPECIFIED.);
#2278=B_SPLINE_CURVE_WITH_KNOTS('',3,(#30006,#30007,#30008,#30009,#30010,
#30011,#30012,#30013,#30014,#30015,#30016,#30017,#30018,#30019,#30020,#30021,
#30022,#30023,#30024,#30025,#30026,#30027,#30028,#30029,#30030),
 .UNSPECIFIED.,.F.,.F.,(4,3,3,3,3,3,3,3,4),(0.,0.125,0.25,0.375,0.5,0.625,
0.75,0.875,0.999990443023589),.UNSPECIFIED.);
#2279=B_SPLINE_CURVE_WITH_KNOTS('',3,(#30032,#30033,#30034,#30035,#30036,
#30037,#30038,#30039,#30040,#30041,#30042,#30043,#30044,#30045,#30046,#30047,
#30048,#30049,#30050,#30051,#30052,#30053,#30054,#30055,#30056,#30057,#30058,
#30059,#30060,#30061,#30062,#30063,#30064,#30065,#30066,#30067,#30068,#30069,
#30070,#30071,#30072,#30073,#30074,#30075,#30076,#30077,#30078,#30079,#30080,
#30081,#30082,#30083,#30084,#30085,#30086,#30087,#30088,#30089,#30090,#30091,
#30092),.UNSPECIFIED.,.F.,.F.,(4,3,3,3,3,3,3,3,3,3,3,3,3,3,3,3,3,3,3,3,
4),(0.,0.0663146289378614,0.07692307692308,0.136515469134231,0.1538461538462,
0.211741372047688,0.2307692307692,0.290800694414924,0.3076923076923,0.379751797937426,
0.3846153846154,0.4615384615385,0.5384615384615,0.6153846153846,0.6923076923077,
0.7692307692308,0.828610667313207,0.8461538461538,0.906927705756478,0.9230769230769,
1.),.UNSPECIFIED.);
#2280=B_SPLINE_CURVE_WITH_KNOTS('',3,(#30094,#30095,#30096,#30097,#30098,
#30099,#30100,#30101,#30102,#30103,#30104,#30105,#30106,#30107,#30108,#30109,
#30110,#30111,#30112,#30113,#30114,#30115,#30116,#30117,#30118,#30119,#30120,
#30121),.UNSPECIFIED.,.F.,.F.,(4,3,3,3,3,3,3,3,3,4),(5.14241135831679E-7,
0.160029392004496,0.25,0.375,0.5,0.61640254692559,0.729407831456665,0.75,
0.909028757457081,0.999999999352541),.UNSPECIFIED.);
#2281=B_SPLINE_CURVE_WITH_KNOTS('',3,(#30124,#30125,#30126,#30127,#30128,
#30129,#30130,#30131,#30132,#30133,#30134,#30135,#30136,#30137,#30138,#30139,
#30140,#30141,#30142,#30143,#30144,#30145,#30146,#30147,#30148,#30149,#30150,
#30151),.UNSPECIFIED.,.F.,.F.,(4,3,3,3,3,3,3,3,3,4),(1.70307404208227E-6,
0.148032548383099,0.25,0.362172850239079,0.475120550633577,0.5,0.643652911896944,
0.75,0.936626754284207,1.),.UNSPECIFIED.);
#2282=B_SPLINE_CURVE_WITH_KNOTS('',3,(#30154,#30155,#30156,#30157,#30158,
#30159,#30160,#30161,#30162,#30163,#30164,#30165,#30166,#30167,#30168,#30169,
#30170,#30171,#30172,#30173,#30174,#30175,#30176,#30177,#30178,#30179,#30180,
#30181,#30182,#30183,#30184,#30185,#30186,#30187,#30188,#30189,#30190,#30191,
#30192,#30193,#30194,#30195,#30196,#30197,#30198,#30199,#30200,#30201,#30202,
#30203,#30204,#30205,#30206,#30207,#30208,#30209,#30210,#30211,#30212,#30213,
#30214),.UNSPECIFIED.,.F.,.F.,(4,3,3,3,3,3,3,3,3,3,3,3,3,3,3,3,3,3,3,3,
4),(0.,0.0663146233673017,0.07692307692308,0.136515470169846,0.1538461538462,
0.211741371816719,0.2307692307692,0.290800694481253,0.3076923076923,0.379751797892978,
0.3846153846154,0.4615384615385,0.5384615384615,0.6153846153846,0.6923076923077,
0.7692307692308,0.828610667312714,0.8461538461538,0.906927705758623,0.9230769230769,
1.),.UNSPECIFIED.);
#2283=B_SPLINE_CURVE_WITH_KNOTS('',3,(#30218,#30219,#30220,#30221,#30222,
#30223,#30224,#30225,#30226,#30227,#30228,#30229,#30230,#30231,#30232,#30233,
#30234,#30235,#30236,#30237,#30238,#30239,#30240,#30241,#30242,#30243,#30244,
#30245),.UNSPECIFIED.,.F.,.F.,(4,3,3,3,3,3,3,3,3,4),(1.70307636311285E-6,
0.148032548423123,0.25,0.362172850244707,0.475120550644421,0.5,0.643652911892531,
0.75,0.93662675425471,1.),.UNSPECIFIED.);
#2284=B_SPLINE_CURVE_WITH_KNOTS('',3,(#30247,#30248,#30249,#30250,#30251,
#30252,#30253,#30254,#30255,#30256,#30257,#30258,#30259,#30260,#30261,#30262,
#30263,#30264,#30265,#30266,#30267,#30268,#30269,#30270,#30271,#30272,#30273,
#30274,#30275,#30276,#30277,#30278,#30279,#30280,#30281,#30282,#30283,#30284,
#30285,#30286,#30287,#30288,#30289,#30290,#30291,#30292,#30293,#30294,#30295,
#30296,#30297,#30298,#30299,#30300,#30301,#30302,#30303,#30304,#30305,#30306,
#30307),.UNSPECIFIED.,.F.,.F.,(4,3,3,3,3,3,3,3,3,3,3,3,3,3,3,3,3,3,3,3,
4),(7.22383709612999E-7,0.07142857142857,0.130487248165143,0.1428571428571,
0.2142857142857,0.2857142857143,0.3571428571429,0.4285714285714,0.5,0.5714285714286,
0.6428571428571,0.704095964849231,0.7142857142857,0.77128683263805,0.7857142857143,
0.84937216056434,0.8571428571429,0.917671280131225,0.9285714285714,0.994058581660706,
0.999999946816668),.UNSPECIFIED.);
#2285=B_SPLINE_CURVE_WITH_KNOTS('',3,(#30308,#30309,#30310,#30311,#30312,
#30313,#30314,#30315,#30316,#30317,#30318,#30319,#30320,#30321,#30322,#30323,
#30324,#30325,#30326,#30327,#30328,#30329,#30330,#30331,#30332),
 .UNSPECIFIED.,.F.,.F.,(4,3,3,3,3,3,3,3,4),(0.,0.125,0.25,0.375,0.5,0.625,
0.75,0.875,0.999990443208001),.UNSPECIFIED.);
#2286=B_SPLINE_CURVE_WITH_KNOTS('',3,(#30337,#30338,#30339,#30340,#30341,
#30342,#30343,#30344,#30345,#30346,#30347,#30348,#30349,#30350,#30351,#30352,
#30353,#30354,#30355,#30356,#30357,#30358,#30359,#30360,#30361,#30362,#30363,
#30364,#30365,#30366,#30367),.UNSPECIFIED.,.F.,.F.,(4,3,3,3,3,3,3,3,3,3,
4),(0.,0.125954731287076,0.252411781724506,0.3333333333333,0.430346749055281,
0.526998647703799,0.621788354340608,0.6666666666667,0.794729988522482,0.918392607343539,
0.999999999718069),.UNSPECIFIED.);
#2287=B_SPLINE_CURVE_WITH_KNOTS('',3,(#30369,#30370,#30371,#30372,#30373,
#30374,#30375,#30376,#30377,#30378,#30379,#30380,#30381,#30382,#30383,#30384,
#30385,#30386,#30387,#30388,#30389,#30390,#30391,#30392,#30393,#30394,#30395,
#30396,#30397,#30398,#30399),.UNSPECIFIED.,.F.,.F.,(4,3,3,3,3,3,3,3,3,3,
4),(0.,0.130818468687397,0.261953697017434,0.3333333333333,0.434213916421035,
0.534690323235047,0.633387339807912,0.6666666666667,0.795921234651223,0.92144431339159,
1.),.UNSPECIFIED.);
#2288=B_SPLINE_CURVE_WITH_KNOTS('',3,(#30400,#30401,#30402,#30403,#30404,
#30405),.UNSPECIFIED.,.F.,.F.,(4,1,1,4),(3.63423291666588E-7,0.3333333333333,
0.6666666666667,1.),.UNSPECIFIED.);
#2289=B_SPLINE_CURVE_WITH_KNOTS('',3,(#30409,#30410,#30411,#30412,#30413,
#30414,#30415,#30416,#30417,#30418,#30419,#30420,#30421,#30422,#30423,#30424,
#30425,#30426,#30427,#30428,#30429,#30430,#30431,#30432,#30433,#30434,#30435,
#30436,#30437,#30438,#30439),.UNSPECIFIED.,.F.,.F.,(4,3,3,3,3,3,3,3,3,3,
4),(0.,0.130847171763814,0.262009658964655,0.3333333333333,0.434235825723054,
0.534733660584684,0.633452212258911,0.6666666666667,0.795945015121965,0.921493668359201,
1.),.UNSPECIFIED.);
#2290=B_SPLINE_CURVE_WITH_KNOTS('',3,(#30441,#30442,#30443,#30444,#30445,
#30446),.UNSPECIFIED.,.F.,.F.,(4,1,1,4),(3.63422558971584E-7,0.3333333333333,
0.6666666666667,0.999990003239561),.UNSPECIFIED.);
#2291=B_SPLINE_CURVE_WITH_KNOTS('',3,(#30452,#30453,#30454,#30455,#30456,
#30457),.UNSPECIFIED.,.F.,.F.,(4,1,1,4),(0.,0.3333333333333,0.6666666666667,
1.),.UNSPECIFIED.);
#2292=B_SPLINE_CURVE_WITH_KNOTS('',3,(#30458,#30459,#30460,#30461,#30462,
#30463,#30464,#30465,#30466,#30467,#30468,#30469,#30470,#30471,#30472,#30473,
#30474,#30475,#30476,#30477,#30478,#30479,#30480,#30481,#30482,#30483,#30484,
#30485,#30486,#30487,#30488),.UNSPECIFIED.,.F.,.F.,(4,3,3,3,3,3,3,3,3,3,
4),(0.,0.1259452709169,0.252394138339945,0.3333333333333,0.43034115248585,
0.526987994119367,0.621773123421767,0.6666666666667,0.794723073389028,0.918379100763244,
0.999999999718263),.UNSPECIFIED.);
#2293=B_SPLINE_CURVE_WITH_KNOTS('',3,(#30566,#30567,#30568,#30569,#30570,
#30571,#30572,#30573,#30574,#30575,#30576,#30577,#30578,#30579,#30580,#30581,
#30582,#30583,#30584,#30585,#30586,#30587,#30588,#30589,#30590,#30591,#30592,
#30593,#30594,#30595,#30596,#30597,#30598,#30599,#30600,#30601,#30602,#30603,
#30604,#30605,#30606,#30607,#30608,#30609,#30610,#30611,#30612,#30613,#30614,
#30615,#30616,#30617,#30618,#30619,#30620,#30621,#30622,#30623,#30624,#30625,
#30626,#30627,#30628,#30629,#30630,#30631,#30632,#30633,#30634,#30635,#30636,
#30637,#30638,#30639,#30640,#30641,#30642,#30643,#30644,#30645,#30646,#30647,
#30648,#30649,#30650,#30651,#30652,#30653,#30654,#30655,#30656,#30657,#30658,
#30659,#30660,#30661,#30662,#30663,#30664,#30665),.UNSPECIFIED.,.F.,.F.,
(4,3,3,3,3,3,3,3,3,3,3,3,3,3,3,3,3,3,3,3,3,3,3,3,3,3,3,3,3,3,3,3,3,4),(1.69542913732478E-6,
5.55774553963063E-6,0.0506373367285727,0.06666666666667,0.0714682425632464,
0.115276661695045,0.1333333333333,0.142868118980489,0.2,0.214286769582239,
0.2666666666667,0.28571683247243,0.3333333333333,0.357160916416442,0.4,
0.428567710291777,0.4666666666667,0.499988290679686,0.5333333333333,0.571448700847799,
0.6,0.642858260431062,0.6666666666667,0.714263915658083,0.7333333333333,
0.785692727180372,0.8,0.857135318884438,0.8666666666667,0.919354891573766,
0.928569821196086,0.9333333333333,0.978447646356298,0.999999941726635),
 .UNSPECIFIED.);
#2294=B_SPLINE_CURVE_WITH_KNOTS('',3,(#30710,#30711,#30712,#30713,#30714,
#30715,#30716,#30717,#30718),.UNSPECIFIED.,.F.,.F.,(4,1,1,1,1,1,4),(0.,
0.1666666666667,0.3333333333333,0.5,0.6666666666667,0.8333333333333,1.),
 .UNSPECIFIED.);
#2295=B_SPLINE_CURVE_WITH_KNOTS('',3,(#30769,#30770,#30771,#30772,#30773,
#30774,#30775,#30776,#30777,#30778,#30779,#30780,#30781,#30782,#30783,#30784,
#30785,#30786,#30787,#30788,#30789,#30790),.UNSPECIFIED.,.F.,.F.,(4,3,3,
3,3,3,3,4),(1.1084212699507E-8,0.1428571428571,0.2857142857143,0.4285714285714,
0.5714285714286,0.7142857142857,0.8571428571429,1.),.UNSPECIFIED.);
#2296=B_SPLINE_CURVE_WITH_KNOTS('',3,(#30833,#30834,#30835,#30836,#30837,
#30838,#30839,#30840,#30841,#30842,#30843,#30844,#30845,#30846,#30847,#30848,
#30849,#30850,#30851,#30852,#30853,#30854,#30855,#30856,#30857,#30858,#30859,
#30860,#30861,#30862,#30863,#30864,#30865,#30866,#30867,#30868,#30869,#30870,
#30871,#30872,#30873,#30874,#30875,#30876,#30877,#30878,#30879,#30880,#30881,
#30882,#30883,#30884,#30885,#30886,#30887,#30888,#30889,#30890,#30891,#30892,
#30893,#30894,#30895,#30896,#30897,#30898,#30899,#30900,#30901,#30902,#30903,
#30904,#30905,#30906,#30907,#30908),.UNSPECIFIED.,.F.,.F.,(4,3,3,3,3,3,
3,3,3,3,3,3,3,3,3,3,3,3,3,3,3,3,3,3,3,4),(0.,0.0592153996085023,0.07692307692308,
0.137971746780227,0.1538461538462,0.156168787894468,0.216720874791267,0.2307692307692,
0.298403926768459,0.3076923076923,0.331220102378383,0.3846153846154,0.4615384615385,
0.521400106932983,0.5384615384615,0.6153846153846,0.6923076923077,0.723395663582115,
0.7692307692308,0.816611805544586,0.8461538461538,0.884333781161934,0.9186849174366,
0.9230769230769,0.96998386836785,1.),.UNSPECIFIED.);
#2297=B_SPLINE_CURVE_WITH_KNOTS('',3,(#30910,#30911,#30912,#30913,#30914,
#30915,#30916,#30917,#30918),.UNSPECIFIED.,.F.,.F.,(4,1,1,1,1,1,4),(0.,
0.1666666666667,0.3333333333333,0.5,0.6666666666667,0.8333333333333,1.),
 .UNSPECIFIED.);
#2298=B_SPLINE_CURVE_WITH_KNOTS('',3,(#31029,#31030,#31031,#31032,#31033,
#31034,#31035,#31036,#31037,#31038,#31039,#31040,#31041,#31042,#31043,#31044,
#31045,#31046,#31047,#31048,#31049,#31050,#31051,#31052,#31053,#31054,#31055,
#31056,#31057,#31058,#31059),.UNSPECIFIED.,.F.,.F.,(4,3,3,3,3,3,3,3,3,3,
4),(1.57239599141992E-10,2.54069328459158E-6,0.159202034791914,0.25,0.376732535786759,
0.5,0.617341130243194,0.727443674690462,0.75,0.883645545812357,1.),
 .UNSPECIFIED.);
#2299=B_SPLINE_CURVE_WITH_KNOTS('',3,(#31180,#31181,#31182,#31183,#31184,
#31185,#31186,#31187,#31188,#31189,#31190,#31191,#31192,#31193,#31194,#31195,
#31196,#31197,#31198,#31199,#31200,#31201,#31202,#31203,#31204,#31205,#31206,
#31207,#31208,#31209,#31210,#31211,#31212,#31213,#31214,#31215,#31216,#31217,
#31218,#31219),.UNSPECIFIED.,.F.,.F.,(4,3,3,3,3,3,3,3,3,3,3,3,3,4),(2.2699531152341E-8,
0.103311520700458,0.2,0.286201587337603,0.372168890942023,0.4,0.476223324327245,
0.553399886495743,0.6,0.677580084830424,0.75318919947951,0.8,0.9,1.),
 .UNSPECIFIED.);
#2300=B_SPLINE_CURVE_WITH_KNOTS('',3,(#31221,#31222,#31223,#31224,#31225,
#31226,#31227,#31228,#31229,#31230,#31231,#31232,#31233,#31234,#31235,#31236),
 .UNSPECIFIED.,.F.,.F.,(4,3,3,3,3,4),(6.47517031980386E-8,0.2,0.4,0.6,0.8,
1.),.UNSPECIFIED.);
#2301=B_SPLINE_CURVE_WITH_KNOTS('',3,(#31240,#31241,#31242,#31243,#31244,
#31245,#31246,#31247,#31248,#31249,#31250,#31251,#31252,#31253,#31254,#31255,
#31256,#31257,#31258,#31259,#31260,#31261,#31262,#31263,#31264,#31265,#31266,
#31267,#31268,#31269,#31270,#31271,#31272,#31273,#31274,#31275,#31276,#31277,
#31278,#31279,#31280,#31281,#31282),.UNSPECIFIED.,.F.,.F.,(4,3,3,3,3,3,
3,3,3,3,3,3,3,3,4),(0.,0.13680594551161,0.2,0.285955328618731,0.372421439212899,
0.4,0.479957503419453,0.560598442976324,0.6,0.6842803069857,0.766645874408388,
0.8,0.892157249049824,0.983321048433859,1.),.UNSPECIFIED.);
#2302=B_SPLINE_CURVE_WITH_KNOTS('',3,(#31327,#31328,#31329,#31330,#31331,
#31332,#31333,#31334,#31335,#31336,#31337,#31338,#31339,#31340,#31341,#31342,
#31343,#31344,#31345,#31346,#31347,#31348,#31349,#31350,#31351,#31352,#31353,
#31354,#31355,#31356,#31357,#31358,#31359,#31360,#31361,#31362,#31363,#31364,
#31365,#31366),.UNSPECIFIED.,.F.,.F.,(4,3,3,3,3,3,3,3,3,3,3,3,3,4),(0.,
0.0880591607118253,0.178417667099241,0.2,0.3,0.4,0.489234741416802,0.579519070321251,
0.6,0.702140086482547,0.8,0.9,0.994158707978447,1.),.UNSPECIFIED.);
#2303=B_SPLINE_CURVE_WITH_KNOTS('',3,(#31460,#31461,#31462,#31463,#31464,
#31465,#31466,#31467,#31468,#31469,#31470,#31471,#31472,#31473,#31474,#31475,
#31476,#31477,#31478,#31479,#31480,#31481,#31482,#31483,#31484,#31485,#31486,
#31487),.UNSPECIFIED.,.F.,.F.,(4,3,3,3,3,3,3,3,3,4),(1.21821800129127E-6,
0.160266398966175,0.25,0.364545774686354,0.481323316787605,0.5,0.656740249234776,
0.75,0.933155046279077,1.),.UNSPECIFIED.);
#2304=B_SPLINE_CURVE_WITH_KNOTS('',3,(#31528,#31529,#31530,#31531,#31532,
#31533,#31534,#31535,#31536,#31537,#31538,#31539,#31540,#31541,#31542,#31543,
#31544,#31545,#31546,#31547,#31548,#31549,#31550,#31551,#31552,#31553,#31554,
#31555,#31556,#31557,#31558,#31559,#31560,#31561,#31562,#31563,#31564,#31565,
#31566,#31567),.UNSPECIFIED.,.F.,.F.,(4,3,3,3,3,3,3,3,3,3,3,3,3,4),(0.,
0.174080255493949,0.2,0.333088302546735,0.4,0.539879197218967,0.6,0.715691417056306,
0.8,0.800008541116262,0.881499130100446,0.954334364786703,0.999998056106661,
1.),.UNSPECIFIED.);
#2305=B_SPLINE_CURVE_WITH_KNOTS('',3,(#31648,#31649,#31650,#31651,#31652,
#31653,#31654,#31655,#31656,#31657,#31658,#31659,#31660,#31661,#31662,#31663,
#31664,#31665,#31666,#31667,#31668,#31669,#31670,#31671,#31672,#31673,#31674,
#31675,#31676,#31677,#31678,#31679,#31680,#31681,#31682,#31683,#31684),
 .UNSPECIFIED.,.F.,.F.,(4,3,3,3,3,3,3,3,3,3,3,3,4),(1.14108591780362E-6,
0.115739668942159,0.231444518862999,0.249995974733526,0.25,0.355385370734019,
0.467872041751315,0.5,0.500003046647521,0.684307366792377,0.75,0.933806640317145,
0.999999643059945),.UNSPECIFIED.);
#2306=B_SPLINE_CURVE_WITH_KNOTS('',3,(#31809,#31810,#31811,#31812,#31813,
#31814,#31815,#31816,#31817,#31818,#31819,#31820,#31821,#31822,#31823,#31824,
#31825,#31826,#31827,#31828,#31829,#31830,#31831,#31832,#31833,#31834,#31835,
#31836,#31837,#31838,#31839,#31840,#31841,#31842),.UNSPECIFIED.,.F.,.F.,
(4,3,3,3,3,3,3,3,3,3,3,4),(0.,0.1666666666667,0.3333333333333,0.457241527305633,
0.5,0.634566199399875,0.6666666666667,0.753406160986073,0.8333333333333,
0.842232829732858,0.93919897654023,1.),.UNSPECIFIED.);
#2307=B_SPLINE_CURVE_WITH_KNOTS('',3,(#31925,#31926,#31927,#31928,#31929,
#31930,#31931,#31932,#31933,#31934,#31935,#31936,#31937,#31938,#31939,#31940,
#31941,#31942,#31943,#31944,#31945,#31946,#31947,#31948,#31949,#31950,#31951,
#31952),.UNSPECIFIED.,.F.,.F.,(4,3,3,3,3,3,3,3,3,4),(2.03304784235694E-6,
0.143958436059573,0.24999198002735,0.25,0.428963387921959,0.5,0.674742399991522,
0.75,0.926384911213618,0.999999999165273),.UNSPECIFIED.);
#2308=B_SPLINE_CURVE_WITH_KNOTS('',3,(#31962,#31963,#31964,#31965,#31966,
#31967,#31968,#31969,#31970,#31971,#31972,#31973,#31974,#31975,#31976,#31977,
#31978,#31979,#31980,#31981,#31982,#31983,#31984,#31985,#31986,#31987,#31988,
#31989),.UNSPECIFIED.,.F.,.F.,(4,3,3,3,3,3,3,3,3,4),(8.41153876261982E-7,
0.139660100393563,0.1666666666667,0.3333333333333,0.5,0.644637832867149,
0.6666666666667,0.81340796009515,0.8333333333333,0.999999999532787),
 .UNSPECIFIED.);
#2309=B_SPLINE_CURVE_WITH_KNOTS('',3,(#32095,#32096,#32097,#32098,#32099,
#32100,#32101,#32102,#32103,#32104,#32105,#32106,#32107,#32108,#32109,#32110,
#32111,#32112,#32113,#32114,#32115,#32116,#32117,#32118,#32119,#32120,#32121,
#32122),.UNSPECIFIED.,.F.,.F.,(4,3,3,3,3,3,3,3,3,4),(1.21821525451887E-6,
0.160266398961143,0.25,0.364545774692073,0.481323316799271,0.5,0.656740249229234,
0.75,0.933155046291152,1.),.UNSPECIFIED.);
#2310=B_SPLINE_CURVE_WITH_KNOTS('',3,(#32163,#32164,#32165,#32166,#32167,
#32168,#32169,#32170,#32171,#32172,#32173,#32174,#32175,#32176,#32177,#32178,
#32179,#32180,#32181,#32182,#32183,#32184,#32185,#32186,#32187,#32188,#32189,
#32190,#32191,#32192,#32193,#32194,#32195,#32196,#32197,#32198,#32199,#32200,
#32201,#32202),.UNSPECIFIED.,.F.,.F.,(4,3,3,3,3,3,3,3,3,3,3,3,3,4),(0.,
0.0873072382834166,0.176851949375498,0.2,0.3,0.4,0.489488062363135,0.580299164992892,
0.6,0.7,0.8,0.9,0.994991847753164,1.),.UNSPECIFIED.);
#2311=B_SPLINE_CURVE_WITH_KNOTS('',3,(#32206,#32207,#32208,#32209,#32210,
#32211,#32212),.UNSPECIFIED.,.F.,.F.,(4,1,1,1,4),(4.6145470383373E-8,0.25,
0.5,0.75,1.),.UNSPECIFIED.);
#2312=B_SPLINE_CURVE_WITH_KNOTS('',3,(#32214,#32215,#32216,#32217,#32218,
#32219,#32220,#32221,#32222,#32223,#32224,#32225,#32226,#32227,#32228,#32229,
#32230,#32231,#32232,#32233,#32234,#32235,#32236,#32237,#32238,#32239,#32240,
#32241,#32242,#32243,#32244,#32245,#32246,#32247,#32248,#32249,#32250,#32251,
#32252,#32253,#32254,#32255,#32256,#32257,#32258,#32259,#32260,#32261,#32262,
#32263,#32264,#32265,#32266,#32267,#32268,#32269,#32270,#32271,#32272,#32273,
#32274,#32275,#32276,#32277,#32278,#32279,#32280,#32281,#32282,#32283,#32284,
#32285,#32286,#32287,#32288,#32289,#32290,#32291,#32292,#32293,#32294,#32295,
#32296,#32297,#32298,#32299,#32300,#32301,#32302,#32303,#32304,#32305,#32306,
#32307,#32308,#32309,#32310,#32311,#32312,#32313,#32314,#32315,#32316,#32317,
#32318,#32319,#32320,#32321,#32322,#32323,#32324,#32325,#32326,#32327,#32328,
#32329,#32330,#32331,#32332,#32333,#32334,#32335,#32336,#32337,#32338,#32339,
#32340,#32341,#32342,#32343,#32344,#32345,#32346,#32347,#32348,#32349,#32350,
#32351,#32352),.UNSPECIFIED.,.F.,.F.,(4,3,3,3,3,3,3,3,3,3,3,3,3,3,3,3,3,
3,3,3,3,3,3,3,3,3,3,3,3,3,3,3,3,3,3,3,3,3,3,3,3,3,3,3,3,3,4),(0.,0.0227804383416707,
0.03703703703704,0.07407407407407,0.105393757646733,0.1111111111111,0.1481481481481,
0.171652082563555,0.1851851851852,0.206342119921921,0.2222222222222,0.255267041242846,
0.2592592592593,0.283739101009767,0.2962962962963,0.3333333333333,0.3703703703704,
0.4074074074074,0.441759331394964,0.4444444444444,0.476437287297752,0.4814814814815,
0.5185185185185,0.5555555555556,0.579466611196372,0.5925925925926,0.615050887578397,
0.6296296296296,0.651825697816008,0.6666666666667,0.689429242643129,0.7037037037037,
0.733601140280399,0.7407407407407,0.775250041261276,0.7777777777778,0.811949750863182,
0.8148148148148,0.8518518518519,0.881392679271282,0.8888888888889,0.924034877764861,
0.9259259259259,0.96104211205333,0.962962962963,0.992579641396002,1.),
 .UNSPECIFIED.);
#2313=B_SPLINE_CURVE_WITH_KNOTS('',3,(#32354,#32355,#32356,#32357,#32358,
#32359,#32360,#32361,#32362,#32363,#32364,#32365,#32366),.UNSPECIFIED.,
 .F.,.F.,(4,3,3,3,4),(2.51811213932785E-8,0.25,0.5,0.75,1.),
 .UNSPECIFIED.);
#2314=B_SPLINE_CURVE_WITH_KNOTS('',3,(#32444,#32445,#32446,#32447,#32448,
#32449,#32450,#32451,#32452),.UNSPECIFIED.,.F.,.F.,(4,1,1,1,1,1,4),(0.,
0.1666666666667,0.3333333333333,0.5,0.6666666666667,0.8333333333333,1.),
 .UNSPECIFIED.);
#2315=B_SPLINE_CURVE_WITH_KNOTS('',3,(#32454,#32455,#32456,#32457,#32458,
#32459,#32460,#32461,#32462,#32463,#32464,#32465,#32466,#32467,#32468,#32469,
#32470,#32471,#32472,#32473,#32474,#32475),.UNSPECIFIED.,.F.,.F.,(4,3,3,
3,3,3,3,4),(1.10839718840703E-8,0.1428571428571,0.2857142857143,0.4285714285714,
0.5714285714286,0.7142857142857,0.8571428571429,1.),.UNSPECIFIED.);
#2316=B_SPLINE_CURVE_WITH_KNOTS('',3,(#32476,#32477,#32478,#32479,#32480,
#32481,#32482,#32483,#32484),.UNSPECIFIED.,.F.,.F.,(4,1,1,1,1,1,4),(0.,
0.1666666666667,0.3333333333333,0.5,0.6666666666667,0.8333333333333,1.),
 .UNSPECIFIED.);
#2317=B_SPLINE_CURVE_WITH_KNOTS('',3,(#32486,#32487,#32488,#32489,#32490,
#32491,#32492),.UNSPECIFIED.,.F.,.F.,(4,1,1,1,4),(5.24779788127142E-8,0.25,
0.5,0.75,1.),.UNSPECIFIED.);
#2318=B_SPLINE_CURVE_WITH_KNOTS('',3,(#32494,#32495,#32496,#32497,#32498,
#32499,#32500,#32501,#32502,#32503,#32504,#32505,#32506,#32507,#32508,#32509,
#32510,#32511,#32512,#32513,#32514,#32515,#32516,#32517,#32518,#32519,#32520,
#32521,#32522,#32523,#32524,#32525,#32526,#32527,#32528,#32529,#32530,#32531,
#32532,#32533,#32534,#32535,#32536,#32537,#32538,#32539,#32540,#32541,#32542,
#32543,#32544,#32545,#32546,#32547,#32548,#32549,#32550,#32551,#32552,#32553,
#32554,#32555,#32556,#32557,#32558,#32559,#32560,#32561,#32562,#32563,#32564,
#32565,#32566,#32567,#32568,#32569,#32570,#32571,#32572,#32573,#32574,#32575,
#32576,#32577,#32578,#32579,#32580,#32581,#32582,#32583,#32584,#32585,#32586,
#32587,#32588,#32589,#32590,#32591,#32592,#32593,#32594,#32595,#32596,#32597,
#32598,#32599,#32600,#32601,#32602,#32603,#32604,#32605,#32606,#32607,#32608,
#32609,#32610,#32611,#32612,#32613,#32614,#32615,#32616,#32617,#32618,#32619,
#32620,#32621,#32622,#32623,#32624,#32625,#32626,#32627,#32628,#32629,#32630,
#32631,#32632),.UNSPECIFIED.,.F.,.F.,(4,3,3,3,3,3,3,3,3,3,3,3,3,3,3,3,3,
3,3,3,3,3,3,3,3,3,3,3,3,3,3,3,3,3,3,3,3,3,3,3,3,3,3,3,3,3,4),(0.,0.0227845093839862,
0.03703703703704,0.07407407407407,0.105393728442604,0.1111111111111,0.1481481481481,
0.17169446631537,0.1851851851852,0.206344932871926,0.2222222222222,0.2557035750719,
0.2592592592593,0.283717132387724,0.2962962962963,0.3333333333333,0.3703703703704,
0.4074074074074,0.441952044037632,0.4444444444444,0.476531264648132,0.4814814814815,
0.5185185185185,0.5555555555556,0.579551235001554,0.5925925925926,0.614954621736422,
0.6296296296296,0.651869758798282,0.6666666666667,0.689384247655644,0.7037037037037,
0.733707164566707,0.7407407407407,0.775015711726731,0.7777777777778,0.811946415212526,
0.8148148148148,0.8518518518519,0.881398338187637,0.8888888888889,0.923946377325199,
0.9259259259259,0.96100223100447,0.962962962963,0.992566994343094,1.),
 .UNSPECIFIED.);
#2319=B_SPLINE_CURVE_WITH_KNOTS('',3,(#32634,#32635,#32636,#32637,#32638,
#32639,#32640,#32641,#32642,#32643,#32644,#32645,#32646),.UNSPECIFIED.,
 .F.,.F.,(4,3,3,3,4),(2.9457427153716E-8,0.25,0.5,0.75,1.),
 .UNSPECIFIED.);
#2320=B_SPLINE_CURVE_WITH_KNOTS('',3,(#32649,#32650,#32651,#32652,#32653,
#32654,#32655,#32656,#32657,#32658,#32659,#32660,#32661,#32662,#32663,#32664),
 .UNSPECIFIED.,.F.,.F.,(4,3,3,3,3,4),(7.06541338515659E-8,0.2,0.4,0.6,0.8,
1.),.UNSPECIFIED.);
#2321=B_SPLINE_CURVE_WITH_KNOTS('',3,(#32706,#32707,#32708,#32709,#32710,
#32711,#32712,#32713,#32714,#32715,#32716,#32717,#32718,#32719,#32720,#32721,
#32722,#32723,#32724,#32725,#32726,#32727,#32728,#32729,#32730,#32731,#32732,
#32733,#32734,#32735,#32736,#32737,#32738,#32739,#32740,#32741,#32742,#32743,
#32744,#32745),.UNSPECIFIED.,.F.,.F.,(4,3,3,3,3,3,3,3,3,3,3,3,3,4),(2.47725076196298E-8,
0.10534087193495,0.2,0.289177733415754,0.377970090718556,0.4,0.475948493762322,
0.552624124210195,0.6,0.681040095770149,0.75981969748944,0.8,0.9,1.),
 .UNSPECIFIED.);
#2322=B_SPLINE_CURVE_WITH_KNOTS('',3,(#32750,#32751,#32752,#32753,#32754,
#32755,#32756,#32757,#32758,#32759,#32760,#32761,#32762,#32763,#32764,#32765,
#32766,#32767,#32768,#32769,#32770,#32771,#32772,#32773,#32774,#32775,#32776,
#32777,#32778,#32779,#32780,#32781,#32782,#32783,#32784,#32785,#32786,#32787,
#32788,#32789,#32790,#32791,#32792),.UNSPECIFIED.,.F.,.F.,(4,3,3,3,3,3,
3,3,3,3,3,3,3,3,4),(0.,0.134788958835649,0.2,0.283389163058699,0.36731742804291,
0.4,0.480376948958258,0.561646740947815,0.6,0.680148416600893,0.758660279668076,
0.8,0.89004290129727,0.979061936724548,1.),.UNSPECIFIED.);
#2323=B_SPLINE_CURVE_WITH_KNOTS('',3,(#32976,#32977,#32978,#32979,#32980,
#32981,#32982,#32983,#32984,#32985,#32986,#32987,#32988,#32989,#32990,#32991,
#32992,#32993,#32994,#32995,#32996,#32997,#32998,#32999,#33000,#33001,#33002,
#33003),.UNSPECIFIED.,.F.,.F.,(4,3,3,3,3,3,3,3,3,4),(1.61555868942031E-8,
0.18960286946556,0.25,0.375,0.5,0.625,0.740175560169049,0.75,0.881701904926917,
1.),.UNSPECIFIED.);
#2324=B_SPLINE_CURVE_WITH_KNOTS('',3,(#33008,#33009,#33010,#33011,#33012,
#33013,#33014,#33015,#33016,#33017,#33018,#33019,#33020,#33021,#33022,#33023,
#33024,#33025,#33026,#33027,#33028,#33029,#33030,#33031,#33032),
 .UNSPECIFIED.,.F.,.F.,(4,3,3,3,3,3,3,3,4),(3.13800440150335E-8,0.148044836757143,
0.25,0.381998755728953,0.5,0.625,0.75,0.880006403819899,1.),
 .UNSPECIFIED.);
#2325=B_SPLINE_CURVE_WITH_KNOTS('',3,(#33199,#33200,#33201,#33202,#33203,
#33204,#33205,#33206,#33207,#33208,#33209,#33210,#33211,#33212,#33213,#33214,
#33215,#33216,#33217,#33218,#33219,#33220,#33221,#33222,#33223,#33224,#33225,
#33226,#33227,#33228,#33229,#33230,#33231,#33232,#33233,#33234,#33235,#33236,
#33237,#33238,#33239,#33240,#33241,#33242,#33243,#33244,#33245,#33246,#33247,
#33248,#33249,#33250,#33251,#33252,#33253,#33254,#33255,#33256,#33257,#33258,
#33259,#33260,#33261,#33262,#33263,#33264,#33265,#33266,#33267,#33268,#33269,
#33270,#33271,#33272,#33273,#33274,#33275,#33276,#33277,#33278,#33279,#33280,
#33281,#33282,#33283,#33284,#33285,#33286,#33287,#33288,#33289,#33290,#33291,
#33292,#33293,#33294,#33295,#33296,#33297,#33298,#33299,#33300,#33301,#33302,
#33303,#33304,#33305,#33306,#33307,#33308,#33309,#33310,#33311,#33312,#33313,
#33314,#33315,#33316,#33317,#33318,#33319,#33320,#33321,#33322,#33323,#33324,
#33325,#33326,#33327,#33328,#33329,#33330,#33331,#33332,#33333,#33334,#33335,
#33336,#33337,#33338,#33339,#33340,#33341,#33342,#33343,#33344,#33345,#33346,
#33347,#33348,#33349,#33350,#33351,#33352,#33353,#33354,#33355,#33356,#33357,
#33358,#33359,#33360,#33361,#33362,#33363,#33364,#33365,#33366,#33367,#33368,
#33369,#33370,#33371,#33372,#33373,#33374,#33375,#33376,#33377,#33378,#33379,
#33380,#33381,#33382,#33383,#33384,#33385,#33386,#33387,#33388,#33389,#33390,
#33391),.UNSPECIFIED.,.F.,.F.,(4,3,3,3,3,3,3,3,3,3,3,3,3,3,3,3,3,3,3,3,
3,3,3,3,3,3,3,3,3,3,3,3,3,3,3,3,3,3,3,3,3,3,3,3,3,3,3,3,3,3,3,3,3,3,3,3,
3,3,3,3,3,3,3,3,4),(0.,0.0158753989555512,0.0320140903722559,0.03703703703704,
0.0505952807113718,0.0645704283886565,0.07407407407407,0.092592592592585,
0.1111111111111,0.130016736639153,0.1481481481481,0.16230401228581,0.17679020103838,
0.1851851851852,0.198952837567042,0.212747578072399,0.2222222222222,0.24403267386365,
0.2592592592593,0.276080579509804,0.292869611775802,0.2962962962963,0.318799233780505,
0.3333333333333,0.358324870880841,0.3703703703704,0.4074074074074,0.433897901523346,
0.4444444444444,0.468170095258189,0.4814814814815,0.511388926566693,0.5185185185185,
0.542320497906127,0.5555555555556,0.57190664168362,0.588363012021197,0.5925925925926,
0.607301801204851,0.622385682318724,0.6296296296296,0.64442539279618,0.659647939515595,
0.6666666666667,0.681611773858689,0.696639654563951,0.7037037037037,0.723990226377065,
0.7407407407407,0.76341671663032,0.7777777777778,0.799246099943322,0.8148148148148,
0.841827649657547,0.8518518518519,0.869437743955809,0.886783138376001,0.8888888888889,
0.9074074074074,0.9259259259259,0.942545285990403,0.958686130318573,0.962962962963,
0.984332770802104,1.),.UNSPECIFIED.);
#2326=B_SPLINE_CURVE_WITH_KNOTS('',3,(#33395,#33396,#33397,#33398,#33399,
#33400,#33401,#33402,#33403,#33404,#33405,#33406,#33407,#33408,#33409,#33410,
#33411,#33412,#33413,#33414,#33415,#33416,#33417,#33418,#33419,#33420,#33421,
#33422,#33423,#33424,#33425,#33426,#33427,#33428,#33429,#33430,#33431,#33432,
#33433,#33434,#33435,#33436,#33437,#33438,#33439,#33440,#33441,#33442,#33443,
#33444,#33445,#33446,#33447,#33448,#33449,#33450,#33451,#33452,#33453,#33454,
#33455,#33456,#33457,#33458,#33459,#33460,#33461,#33462,#33463,#33464,#33465,
#33466,#33467,#33468,#33469,#33470,#33471,#33472,#33473,#33474,#33475,#33476,
#33477,#33478,#33479,#33480,#33481,#33482,#33483,#33484,#33485,#33486,#33487,
#33488,#33489,#33490,#33491,#33492,#33493,#33494,#33495,#33496,#33497,#33498,
#33499,#33500,#33501,#33502,#33503,#33504,#33505,#33506,#33507,#33508,#33509,
#33510,#33511,#33512,#33513,#33514,#33515,#33516,#33517,#33518,#33519,#33520,
#33521,#33522,#33523,#33524,#33525,#33526,#33527,#33528,#33529,#33530,#33531,
#33532,#33533,#33534,#33535,#33536,#33537,#33538,#33539,#33540,#33541,#33542,
#33543,#33544,#33545,#33546,#33547,#33548,#33549,#33550,#33551,#33552,#33553,
#33554,#33555,#33556,#33557,#33558,#33559,#33560,#33561,#33562,#33563,#33564,
#33565,#33566,#33567,#33568,#33569,#33570,#33571,#33572,#33573,#33574,#33575,
#33576,#33577,#33578,#33579,#33580,#33581,#33582,#33583,#33584,#33585,#33586,
#33587),.UNSPECIFIED.,.F.,.F.,(4,3,3,3,3,3,3,3,3,3,3,3,3,3,3,3,3,3,3,3,
3,3,3,3,3,3,3,3,3,3,3,3,3,3,3,3,3,3,3,3,3,3,3,3,3,3,3,3,3,3,3,3,3,3,3,3,
3,3,3,3,3,3,3,3,4),(0.,0.0165822562128935,0.0334988362068336,0.03703703703704,
0.0507053457331975,0.0647436237201557,0.07407407407407,0.092592592592585,
0.1111111111111,0.130277373557652,0.1481481481481,0.162380982922882,0.176941705207943,
0.1851851851852,0.199007952753526,0.212869450033032,0.2222222222222,0.243969810128695,
0.2592592592593,0.27600395361121,0.29272868746584,0.2962962962963,0.319534274545662,
0.3333333333333,0.359328590068892,0.3703703703704,0.4074074074074,0.43316432447304,
0.4444444444444,0.467750347323342,0.4814814814815,0.514386802020862,0.5185185185185,
0.54295337501735,0.5555555555556,0.571951925973206,0.588445780819957,0.5925925925926,
0.607248493950731,0.622273991910819,0.6296296296296,0.644556288294263,0.659893419231155,
0.6666666666667,0.681650482058062,0.696707258462661,0.7037037037037,0.724031178536157,
0.7407407407407,0.763131518114845,0.7777777777778,0.799393381195803,0.8148148148148,
0.842210623004667,0.8518518518519,0.8703703703704,0.88776312568209,0.8888888888889,
0.9074074074074,0.9259259259259,0.942566718460714,0.958758891551145,0.962962962963,
0.985139306031294,1.),.UNSPECIFIED.);
#2327=B_SPLINE_CURVE_WITH_KNOTS('',3,(#33591,#33592,#33593,#33594,#33595,
#33596,#33597,#33598,#33599,#33600,#33601,#33602,#33603,#33604),
 .UNSPECIFIED.,.F.,.F.,(4,2,2,2,2,2,4),(-1.42633728259246,-1.37599677975708,
-1.2777147925774,-1.17943280539771,-1.08115081821802,-0.982868831038335,
-0.932528328202956),.UNSPECIFIED.);
#2328=B_SPLINE_CURVE_WITH_KNOTS('',3,(#33606,#33607,#33608,#33609,#33610,
#33611,#33612,#33613,#33614,#33615),.UNSPECIFIED.,.F.,.F.,(4,2,2,2,4),(0.662602885754242,
0.706027743980102,0.805474923937918,0.904922103895734,0.948346962121595),
 .UNSPECIFIED.);
#2329=B_SPLINE_CURVE_WITH_KNOTS('',3,(#33617,#33618,#33619,#33620,#33621,
#33622,#33623,#33624,#33625,#33626,#33627,#33628,#33629,#33630),
 .UNSPECIFIED.,.F.,.F.,(4,2,2,2,2,2,4),(-0.640048745660657,-0.589708242825278,
-0.491426255645591,-0.393144268465903,-0.294862281286216,-0.196580294106529,
-0.146239791271149),.UNSPECIFIED.);
#2330=B_SPLINE_CURVE_WITH_KNOTS('',3,(#33631,#33632,#33633,#33634,#33635,
#33636,#33637,#33638,#33639,#33640,#33641),.UNSPECIFIED.,.F.,.F.,(4,2,3,
2,4),(1.46807780969216,1.51150266791802,1.61094984787584,1.71039702783365,
1.75382188605951),.UNSPECIFIED.);
#2331=B_SPLINE_CURVE_WITH_KNOTS('',3,(#33831,#33832,#33833,#33834,#33835,
#33836,#33837,#33838,#33839,#33840,#33841,#33842,#33843,#33844,#33845,#33846,
#33847,#33848,#33849,#33850,#33851,#33852,#33853,#33854,#33855,#33856,#33857,
#33858),.UNSPECIFIED.,.F.,.F.,(4,3,3,3,3,3,3,3,3,4),(3.56871364693513E-8,
0.189519225027544,0.25,0.375012101554345,0.5,0.625,0.741012963505921,0.75,
0.88392559174732,1.),.UNSPECIFIED.);
#2332=B_SPLINE_CURVE_WITH_KNOTS('',3,(#33860,#33861,#33862,#33863,#33864,
#33865,#33866,#33867,#33868,#33869,#33870,#33871,#33872,#33873,#33874,#33875,
#33876,#33877,#33878,#33879,#33880,#33881,#33882,#33883,#33884,#33885,#33886,
#33887),.UNSPECIFIED.,.F.,.F.,(4,3,3,3,3,3,3,3,3,4),(1.38126679696758E-8,
0.187650448938451,0.25,0.375,0.5,0.618621411128423,0.733216918900281,0.75,
0.881423683727945,1.),.UNSPECIFIED.);
#2333=B_SPLINE_CURVE_WITH_KNOTS('',3,(#33964,#33965,#33966,#33967,#33968,
#33969,#33970,#33971,#33972,#33973,#33974,#33975,#33976,#33977,#33978,#33979,
#33980,#33981,#33982,#33983,#33984,#33985,#33986,#33987,#33988,#33989,#33990,
#33991,#33992,#33993,#33994,#33995,#33996,#33997,#33998,#33999,#34000,#34001,
#34002,#34003,#34004,#34005,#34006,#34007,#34008,#34009,#34010,#34011,#34012,
#34013,#34014,#34015,#34016,#34017,#34018,#34019,#34020,#34021,#34022,#34023,
#34024,#34025,#34026,#34027,#34028,#34029,#34030,#34031,#34032,#34033,#34034,
#34035,#34036,#34037,#34038,#34039),.UNSPECIFIED.,.F.,.F.,(4,3,3,3,3,3,
3,3,3,3,3,3,3,3,3,3,3,3,3,3,3,3,3,3,3,4),(1.69545582308687E-6,0.0609595895495215,
0.06666666666667,0.10840451091604,0.11607460416853,0.1333333333333,0.2,
0.2666666666667,0.311268715280741,0.3333333333333,0.4,0.4666666666667,0.501758645465729,
0.5333333333333,0.6,0.6666666666667,0.683482450052278,0.7333333333333,0.796163252121639,
0.8,0.850694627387244,0.8666666666667,0.926125080370586,0.9333333333333,
0.990551624959652,0.999999945911362),.UNSPECIFIED.);
#2334=B_SPLINE_CURVE_WITH_KNOTS('',3,(#34206,#34207,#34208,#34209,#34210,
#34211,#34212,#34213,#34214,#34215,#34216,#34217,#34218,#34219,#34220,#34221,
#34222,#34223,#34224,#34225,#34226,#34227,#34228,#34229,#34230,#34231,#34232,
#34233,#34234,#34235,#34236,#34237,#34238,#34239,#34240,#34241,#34242,#34243,
#34244,#34245,#34246,#34247,#34248,#34249,#34250,#34251,#34252,#34253,#34254,
#34255,#34256,#34257,#34258,#34259,#34260,#34261,#34262,#34263,#34264,#34265,
#34266,#34267,#34268,#34269,#34270,#34271,#34272,#34273,#34274,#34275,#34276,
#34277,#34278,#34279,#34280,#34281),.UNSPECIFIED.,.F.,.F.,(4,3,3,3,3,3,
3,3,3,3,3,3,3,3,3,3,3,3,3,3,3,3,3,3,3,4),(0.,0.0592153998652141,0.07692307692308,
0.137971745989572,0.1538461538462,0.156168787892723,0.216720875042898,0.2307692307692,
0.298403926666996,0.3076923076923,0.331220102375332,0.3846153846154,0.4615384615385,
0.521400106929585,0.5384615384615,0.6153846153846,0.6923076923077,0.723395663579233,
0.7692307692308,0.816611805544925,0.8461538461538,0.88433378116142,0.918684917435874,
0.9230769230769,0.969983868366533,1.),.UNSPECIFIED.);
#2335=B_SPLINE_CURVE_WITH_KNOTS('',3,(#34398,#34399,#34400,#34401,#34402,
#34403,#34404,#34405,#34406,#34407,#34408,#34409,#34410,#34411,#34412,#34413,
#34414,#34415,#34416,#34417,#34418,#34419,#34420,#34421,#34422,#34423,#34424,
#34425,#34426,#34427,#34428,#34429,#34430,#34431),.UNSPECIFIED.,.F.,.F.,
(4,3,3,3,3,3,3,3,3,3,3,4),(3.05224366949974E-7,0.1666666666667,0.320864307652846,
0.3333333333333,0.5,0.643823830912737,0.6666666666667,0.810437048615872,
0.833327065149254,0.8333333333333,0.963427087902464,1.),.UNSPECIFIED.);
#2336=B_SPLINE_CURVE_WITH_KNOTS('',3,(#34596,#34597,#34598,#34599),
 .UNSPECIFIED.,.F.,.F.,(4,4),(-0.00619503390723115,0.),.UNSPECIFIED.);
#2337=B_SPLINE_CURVE_WITH_KNOTS('',3,(#34606,#34607,#34608,#34609,#34610,
#34611,#34612,#34613,#34614,#34615,#34616,#34617,#34618,#34619,#34620,#34621,
#34622,#34623,#34624,#34625,#34626,#34627,#34628,#34629,#34630,#34631,#34632,
#34633,#34634,#34635,#34636,#34637,#34638,#34639,#34640,#34641,#34642,#34643,
#34644,#34645,#34646,#34647,#34648,#34649,#34650,#34651,#34652,#34653,#34654,
#34655,#34656,#34657,#34658,#34659,#34660,#34661,#34662,#34663,#34664,#34665,
#34666,#34667,#34668,#34669,#34670,#34671,#34672,#34673,#34674,#34675,#34676,
#34677,#34678,#34679),.UNSPECIFIED.,.F.,.F.,(4,2,2,2,2,2,2,2,2,2,2,2,2,
2,2,2,2,2,2,2,2,2,2,2,2,2,2,2,2,2,2,2,2,2,2,2,4),(5.60374804517138E-5,0.0237574869632762,
0.0393947601276455,0.0585453864332768,0.08182795489794,0.114860762667679,
0.129204845739769,0.147297192833992,0.17057303225174,0.203467586480588,
0.217878012701244,0.235958253934255,0.259262055153465,0.29253982422056,
0.306780812007485,0.324906546091773,0.348145822827213,0.376378338610298,
0.39336918364381,0.410849344394283,0.451548256241227,0.476499668509328,
0.492967499160127,0.510629733377488,0.537942689233428,0.561233542584866,
0.579498114515359,0.594216460000935,0.626663924529217,0.650241887801689,
0.668490357191975,0.68331215520655,0.714495532592327,0.736570127490707,
0.748116113139686,0.765521137638678,0.786892363085868),.UNSPECIFIED.);
#2338=B_SPLINE_CURVE_WITH_KNOTS('',3,(#34822,#34823,#34824,#34825,#34826,
#34827,#34828,#34829,#34830,#34831,#34832,#34833,#34834,#34835,#34836,#34837,
#34838,#34839,#34840,#34841,#34842,#34843,#34844,#34845,#34846,#34847,#34848,
#34849,#34850,#34851,#34852,#34853,#34854,#34855,#34856,#34857,#34858,#34859,
#34860,#34861,#34862,#34863,#34864,#34865,#34866,#34867,#34868,#34869,#34870,
#34871,#34872,#34873,#34874,#34875,#34876,#34877,#34878,#34879,#34880,#34881,
#34882,#34883,#34884,#34885,#34886,#34887,#34888,#34889,#34890,#34891,#34892,
#34893,#34894,#34895,#34896,#34897,#34898,#34899,#34900,#34901,#34902,#34903,
#34904,#34905,#34906,#34907,#34908,#34909,#34910,#34911,#34912,#34913,#34914,
#34915,#34916,#34917,#34918,#34919,#34920,#34921,#34922,#34923,#34924,#34925,
#34926,#34927,#34928,#34929,#34930,#34931,#34932,#34933,#34934,#34935,#34936,
#34937,#34938,#34939),.UNSPECIFIED.,.F.,.F.,(4,2,2,2,2,2,2,2,2,2,2,2,2,
2,2,2,2,2,2,2,2,2,2,2,2,2,2,2,2,2,2,2,2,2,2,2,2,2,2,2,2,2,2,2,2,2,2,2,2,
2,2,2,2,2,2,2,2,2,4),(4.86308899125306E-5,0.025345822067703,0.0499710023559397,
0.0982392916290599,0.144379179758547,0.169738120416293,0.211164235877253,
0.233786911472833,0.259178954607802,0.300715901245229,0.322405039362481,
0.347812455770367,0.389985850776008,0.410393459018824,0.459653300986646,
0.506189829924729,0.53230871013449,0.574815902384265,0.59800879473142,0.624155748676925,
0.667049786253343,0.689141934513977,0.715301339433927,0.758872833057192,
0.77962771324359,0.830354079494171,0.881187653856567,0.907965106170109,
0.95074336338996,0.97675583503304,1.00356887094136,1.04822229000252,1.09298924554976,
1.11895483964794,1.16660560441434,1.215774402086,1.23658842173518,1.27752886770208,
1.30260580018034,1.32487921810867,1.36439772875352,1.38974130281919,1.43631486645491,
1.48427632141474,1.50456999497759,1.54451517828357,1.56897595594586,1.59069371809725,
1.62925310267272,1.65397444333067,1.69940118356495,1.74620026687915,1.76592586239095,
1.80503271787502,1.8288931679946,1.85039255317872,1.88777689653423,1.92593647559982,
1.97078937517229),.UNSPECIFIED.);
#2339=B_SPLINE_CURVE_WITH_KNOTS('',3,(#34943,#34944,#34945,#34946,#34947,
#34948,#34949,#34950,#34951,#34952,#34953,#34954,#34955,#34956,#34957,#34958,
#34959,#34960,#34961,#34962,#34963,#34964,#34965,#34966,#34967,#34968,#34969,
#34970,#34971,#34972,#34973,#34974,#34975,#34976,#34977,#34978,#34979,#34980,
#34981,#34982,#34983,#34984,#34985,#34986,#34987,#34988,#34989,#34990,#34991,
#34992,#34993,#34994,#34995,#34996,#34997,#34998,#34999,#35000,#35001,#35002,
#35003,#35004,#35005,#35006,#35007,#35008,#35009,#35010,#35011,#35012,#35013,
#35014,#35015,#35016,#35017,#35018,#35019,#35020,#35021,#35022,#35023,#35024,
#35025,#35026,#35027,#35028,#35029,#35030,#35031,#35032,#35033,#35034,#35035,
#35036,#35037,#35038,#35039,#35040,#35041,#35042,#35043,#35044,#35045,#35046,
#35047,#35048,#35049,#35050,#35051,#35052,#35053,#35054,#35055,#35056),
 .UNSPECIFIED.,.F.,.F.,(4,2,2,2,2,2,2,2,2,2,2,2,2,2,2,2,2,2,2,2,2,2,2,2,
2,2,2,2,2,2,2,2,2,2,2,2,2,2,2,2,2,2,2,2,2,2,2,2,2,2,2,2,2,2,2,2,4),(5.9483127789702E-5,
0.0316367019429408,0.0599442114156418,0.0883769919119353,0.116199833618219,
0.148646117264541,0.185649600266805,0.230767737668227,0.2833475209531,0.339441855741448,
0.383998353925252,0.423502762154872,0.462978744712189,0.502190993059282,
0.550924538584899,0.614750411652877,0.690541644647774,0.777537898691589,
0.891899588394075,0.990239042783837,1.0695630442833,1.13517856125268,1.1930368282216,
1.25130241000153,1.30822288488409,1.37470140206806,1.45052897133131,1.54326735518799,
1.65154718908405,1.75982702298013,1.85256540683686,1.92839297610017,1.99487149328411,
2.05179196816666,2.11005754994658,2.16791581691547,2.23353133388489,2.31285533538436,
2.41119478977405,2.5255564794758,2.61255273351889,2.6883439665132,2.75216983958068,
2.80090338510622,2.84011563345335,2.87959161601078,2.91909602424063,2.96365252242471,
3.01974685721341,3.0723266404986,3.11744477790028,3.15444826090276,3.18689454454933,
3.21471738625582,3.2431501667523,3.27145767622518,3.30303409387644),
 .UNSPECIFIED.);
#2340=B_SPLINE_CURVE_WITH_KNOTS('',3,(#35057,#35058,#35059,#35060,#35061,
#35062),.UNSPECIFIED.,.F.,.F.,(4,2,4),(-0.0324107798204044,-0.0161950117464181,
-1.97227469921358E-5),.UNSPECIFIED.);
#2341=B_SPLINE_CURVE_WITH_KNOTS('',3,(#35204,#35205,#35206,#35207,#35208,
#35209,#35210,#35211,#35212,#35213,#35214,#35215,#35216,#35217,#35218,#35219,
#35220,#35221,#35222,#35223,#35224,#35225,#35226,#35227,#35228,#35229,#35230,
#35231,#35232,#35233,#35234,#35235,#35236,#35237,#35238,#35239,#35240,#35241,
#35242,#35243,#35244,#35245,#35246,#35247),.UNSPECIFIED.,.F.,.F.,(4,2,2,
2,2,2,2,2,2,2,2,2,2,2,2,2,2,2,2,2,2,4),(7.68002795625173E-5,0.0286518841616717,
0.0572552412024219,0.105896121009425,0.164583029247044,0.2340740159792,
0.265841679009562,0.301384144553815,0.369456475007765,0.404267289112112,
0.440453098676966,0.503487717030501,0.567113082147453,0.604690173343838,
0.676352451170165,0.748055048385089,0.782538922080911,0.853283578669051,
0.926381914489287,0.997290896804745,1.03897238575266,1.08071694913185),
 .UNSPECIFIED.);
#2342=B_SPLINE_CURVE_WITH_KNOTS('',3,(#35249,#35250,#35251,#35252,#35253,
#35254),.UNSPECIFIED.,.F.,.F.,(4,2,4),(-0.0323546880682321,-0.0162250198953441,
-7.66108474423785E-6),.UNSPECIFIED.);
#2343=B_SPLINE_CURVE_WITH_KNOTS('',3,(#35256,#35257,#35258,#35259,#35260,
#35261,#35262,#35263,#35264,#35265,#35266,#35267,#35268,#35269,#35270,#35271,
#35272,#35273,#35274,#35275,#35276,#35277,#35278,#35279,#35280,#35281,#35282,
#35283,#35284,#35285,#35286,#35287,#35288,#35289,#35290,#35291,#35292,#35293,
#35294,#35295,#35296,#35297,#35298,#35299,#35300,#35301,#35302,#35303,#35304,
#35305,#35306,#35307,#35308,#35309,#35310,#35311,#35312,#35313,#35314,#35315,
#35316,#35317,#35318,#35319,#35320,#35321,#35322,#35323,#35324,#35325,#35326,
#35327,#35328,#35329,#35330,#35331,#35332,#35333,#35334,#35335,#35336,#35337,
#35338,#35339,#35340,#35341,#35342,#35343,#35344,#35345,#35346,#35347,#35348,
#35349,#35350,#35351,#35352,#35353,#35354,#35355,#35356,#35357,#35358,#35359,
#35360,#35361,#35362,#35363,#35364,#35365,#35366,#35367,#35368,#35369),
 .UNSPECIFIED.,.F.,.F.,(4,2,2,2,2,2,2,2,2,2,2,2,2,2,2,2,2,2,2,2,2,2,2,2,
2,2,2,2,2,2,2,2,2,2,2,2,2,2,2,2,2,2,2,2,2,2,2,2,2,2,2,2,2,2,2,2,4),(-3.30330797806971,
-3.2717281475933,-3.24341828644006,-3.21498314385619,-3.18715799073372,
-3.1547090115732,-3.1177024544619,-3.07258056881672,-3.01999641740284,-2.96389742250988,
-2.91933722274118,-2.87982953263513,-2.84035027056288,-2.8011347646109,
-2.75239717048713,-2.68856599500766,-2.61276846556455,-2.52576498420185,
-2.41139379376385,-2.31304616970509,-2.23371557826834,-2.16809461021059,
-2.11023153659623,-2.05196111433268,-1.99503591071289,-1.92855187074577,
-1.85271800201556,-1.75997191380558,-1.65168308443146,-1.54339425505734,
-1.4506481668473,-1.37481429811705,-1.30833025814995,-1.25140505453017,
-1.19313463226664,-1.13527155865229,-1.06965059059451,-0.990319999157752,
-0.891972375099075,-0.777601184661876,-0.690597703299961,-0.614800173857485,
-0.550968998378546,-0.50223140425488,-0.463015898302877,-0.423536636230542,
-0.384028946124274,-0.339468746355297,-0.283369751461995,-0.230785600047816,
-0.18566371440238,-0.148657157290866,-0.116208178130105,-0.0883830250074371,
-0.0599478824233905,-0.0316380212699721,-5.8970516573392E-5),
 .UNSPECIFIED.);
#2344=B_SPLINE_CURVE_WITH_KNOTS('',3,(#35512,#35513,#35514,#35515,#35516,
#35517,#35518,#35519,#35520,#35521,#35522,#35523,#35524,#35525,#35526,#35527,
#35528,#35529,#35530,#35531,#35532,#35533,#35534,#35535,#35536,#35537,#35538,
#35539,#35540,#35541,#35542,#35543,#35544,#35545,#35546,#35547,#35548,#35549,
#35550,#35551,#35552,#35553,#35554,#35555,#35556,#35557,#35558,#35559,#35560,
#35561,#35562,#35563,#35564,#35565,#35566,#35567,#35568,#35569,#35570,#35571,
#35572,#35573,#35574,#35575,#35576,#35577,#35578,#35579,#35580,#35581,#35582,
#35583,#35584,#35585,#35586,#35587,#35588,#35589,#35590,#35591,#35592,#35593,
#35594,#35595,#35596,#35597,#35598,#35599,#35600,#35601,#35602,#35603,#35604,
#35605,#35606,#35607,#35608,#35609,#35610,#35611,#35612,#35613,#35614,#35615,
#35616,#35617,#35618,#35619,#35620,#35621,#35622,#35623,#35624,#35625,#35626,
#35627,#35628,#35629),.UNSPECIFIED.,.F.,.F.,(4,2,2,2,2,2,2,2,2,2,2,2,2,
2,2,2,2,2,2,2,2,2,2,2,2,2,2,2,2,2,2,2,2,2,2,2,2,2,2,2,2,2,2,2,2,2,2,2,2,
2,2,2,2,2,2,2,2,2,4),(4.00512479403123E-5,0.0342074993316949,0.0631190140398426,
0.0925899546592947,0.10920786339202,0.127582223175736,0.157810038290439,
0.173443507766134,0.191832595775175,0.222341299061909,0.237090305071392,
0.272742999074723,0.306561294379606,0.325476646462585,0.356234881757118,
0.373150128431719,0.392087242288704,0.423090526652374,0.439265919840542,
0.458214798157994,0.48966564000899,0.504885740673708,0.541623698931582,
0.576311534812893,0.595787709949363,0.627489287296732,0.644765443703326,
0.664262365513633,0.696256286921859,0.712704551881602,0.732210340892689,
0.768190524101217,0.784517774259878,0.818349961866105,0.860212671232351,
0.916855859608072,0.94190207849065,0.9880100743632,1.01725619500541,1.06975386109676,
1.12552134681956,1.14924716271827,1.19554501871853,1.22399233697437,1.24941480692896,
1.29413044929263,1.32287514891999,1.37597186041185,1.43024555593699,1.45318819332844,
1.49839331258465,1.52607408936872,1.55051417176749,1.59432174380684,1.6222909588055,
1.67460232111634,1.72809366111648,1.75478242650006,1.782350223907),
 .UNSPECIFIED.);
#2345=B_SPLINE_CURVE_WITH_KNOTS('',3,(#35632,#35633,#35634,#35635,#35636,
#35637,#35638,#35639,#35640,#35641,#35642,#35643,#35644,#35645,#35646,#35647,
#35648,#35649,#35650,#35651,#35652,#35653,#35654,#35655,#35656,#35657,#35658,
#35659,#35660,#35661,#35662,#35663,#35664,#35665,#35666,#35667,#35668,#35669,
#35670,#35671,#35672,#35673,#35674,#35675,#35676,#35677,#35678,#35679,#35680,
#35681,#35682,#35683,#35684,#35685,#35686,#35687,#35688,#35689,#35690,#35691,
#35692,#35693,#35694,#35695,#35696,#35697,#35698,#35699,#35700,#35701,#35702,
#35703,#35704,#35705,#35706,#35707,#35708,#35709,#35710,#35711,#35712,#35713,
#35714,#35715,#35716,#35717,#35718,#35719,#35720,#35721,#35722,#35723,#35724,
#35725,#35726,#35727,#35728,#35729,#35730,#35731,#35732,#35733,#35734,#35735,
#35736,#35737,#35738,#35739,#35740,#35741,#35742,#35743,#35744,#35745),
 .UNSPECIFIED.,.F.,.F.,(4,2,2,2,2,2,2,2,2,2,2,2,2,2,2,2,2,2,2,2,2,2,2,2,
2,2,2,2,2,2,2,2,2,2,2,2,2,2,2,2,2,2,2,2,2,2,2,2,2,2,2,2,2,2,2,2,4),(5.94831277841767E-5,
0.0316367019429338,0.0599442114156145,0.0883769919118842,0.116199833618184,
0.148646117264509,0.185649600266781,0.230767737668212,0.283347520953061,
0.339441855741405,0.383998353925216,0.423502762154843,0.462978744712232,
0.5021909930594,0.550924538585036,0.614750411653134,0.690541644648174,0.777537898691899,
0.891899588395087,0.990239042787321,1.0695630442889,1.13517856126005,1.19303682823043,
1.25130241001183,1.3082228848959,1.37470140208164,1.45052897134696,1.54326735520618,
1.65154718910504,1.7598270230039,1.85256540686313,1.92839297612847,1.9948714933142,
2.05179196819826,2.11005754997969,2.16791581695011,2.23353133392122,2.31285533542278,
2.41119478981526,2.52555647952116,2.6125527335676,2.68834396656478,2.75216983963467,
2.80090338516196,2.84011563351046,2.87959161606925,2.91909602430044,2.96365252248596,
3.01974685727651,3.07232664056349,3.11744477796673,3.15444826097047,3.18689454461805,
3.21471738632542,3.24315016682283,3.27145767629665,3.30303488345968),
 .UNSPECIFIED.);
#2346=B_SPLINE_CURVE_WITH_KNOTS('',3,(#35887,#35888,#35889,#35890,#35891,
#35892,#35893,#35894,#35895,#35896,#35897,#35898,#35899,#35900,#35901,#35902,
#35903,#35904,#35905,#35906,#35907,#35908,#35909,#35910,#35911,#35912,#35913,
#35914,#35915,#35916,#35917,#35918,#35919,#35920,#35921,#35922,#35923,#35924,
#35925,#35926,#35927,#35928,#35929,#35930),.UNSPECIFIED.,.F.,.F.,(4,2,2,
2,2,2,2,2,2,2,2,2,2,2,2,2,2,2,2,2,2,4),(4.00913727096806E-5,0.0285826648472843,
0.0571136238949599,0.105754976155757,0.164159095723717,0.23287028670703,
0.264108714287391,0.299243064816363,0.366669064921763,0.40106244750476,
0.436833432270234,0.499315877244998,0.5624507698616,0.599844554878724,0.671009797795569,
0.74195779649287,0.776103848397365,0.84609583637898,0.905678874599204,0.955226346235828,
0.984408120187647,1.01363013542304),.UNSPECIFIED.);
#2347=B_SPLINE_CURVE_WITH_KNOTS('',3,(#35932,#35933,#35934,#35935,#35936,
#35937,#35938,#35939,#35940,#35941,#35942,#35943,#35944,#35945,#35946,#35947,
#35948,#35949,#35950,#35951,#35952,#35953,#35954,#35955,#35956,#35957,#35958,
#35959,#35960,#35961,#35962,#35963,#35964,#35965,#35966,#35967,#35968,#35969,
#35970,#35971,#35972,#35973,#35974,#35975,#35976,#35977,#35978,#35979,#35980,
#35981,#35982,#35983,#35984,#35985,#35986,#35987,#35988,#35989,#35990,#35991,
#35992,#35993,#35994,#35995,#35996,#35997,#35998,#35999,#36000,#36001,#36002,
#36003,#36004,#36005,#36006,#36007,#36008,#36009,#36010,#36011,#36012,#36013,
#36014,#36015,#36016,#36017,#36018,#36019,#36020,#36021,#36022,#36023,#36024,
#36025,#36026,#36027,#36028,#36029,#36030,#36031,#36032,#36033,#36034,#36035,
#36036,#36037,#36038,#36039,#36040,#36041,#36042,#36043,#36044,#36045),
 .UNSPECIFIED.,.F.,.F.,(4,2,2,2,2,2,2,2,2,2,2,2,2,2,2,2,2,2,2,2,2,2,2,2,
2,2,2,2,2,2,2,2,2,2,2,2,2,2,2,2,2,2,2,2,2,2,2,2,2,2,2,2,2,2,2,2,4),(-3.30303488333095,
-3.2714576761704,-3.2431501666988,-3.21471738620362,-3.18689454449838,-3.1544482608533,
-3.11744477785245,-3.07232664045274,-3.01974685716991,-2.96365252238372,
-2.91909602420161,-2.8795916159735,-2.84011563341763,-2.80090338507197,
-2.7521698395482,-2.68834396648255,-2.61255273349043,-2.52555647945005,
-2.41119478975125,-2.31285533536284,-2.23353133386437,-2.1679158168958,
-2.11005754992768,-2.05179196814856,-1.99487149326671,-1.92839297608357,
-1.85256540682122,-1.75982702296562,-1.65154718907099,-1.54326735517636,
-1.45052897132076,-1.37470140205837,-1.30822288487525,-1.25130240999341,
-1.19303682821425,-1.1351785612461,-1.06956304427756,-0.990239042779093,
-0.891899588390449,-0.777537898689057,-0.690541644646066,-0.614750411651893,
-0.550924538584524,-0.502190993059153,-0.462978744712191,-0.423502762154953,
-0.383998353925325,-0.339441855741553,-0.2833475209532,-0.230767737668287,
-0.185649600266819,-0.148646117264527,-0.116199833618222,-0.0883769919119469,
-0.0599442114156555,-0.0316367019429495,-5.94831277973711E-5),
 .UNSPECIFIED.);
#2348=B_SPLINE_CURVE_WITH_KNOTS('',3,(#36188,#36189,#36190,#36191,#36192,
#36193,#36194,#36195,#36196,#36197,#36198,#36199,#36200,#36201,#36202,#36203,
#36204,#36205,#36206,#36207,#36208,#36209,#36210,#36211,#36212,#36213,#36214,
#36215,#36216,#36217,#36218,#36219,#36220,#36221,#36222,#36223,#36224,#36225,
#36226,#36227,#36228,#36229,#36230,#36231,#36232,#36233,#36234,#36235,#36236,
#36237,#36238,#36239,#36240,#36241,#36242,#36243,#36244,#36245,#36246,#36247,
#36248,#36249,#36250,#36251,#36252,#36253,#36254,#36255,#36256,#36257,#36258,
#36259,#36260,#36261,#36262,#36263,#36264,#36265,#36266,#36267,#36268,#36269,
#36270,#36271,#36272,#36273,#36274,#36275,#36276,#36277,#36278,#36279,#36280,
#36281,#36282,#36283,#36284,#36285,#36286,#36287,#36288,#36289,#36290,#36291,
#36292,#36293,#36294,#36295,#36296,#36297,#36298,#36299,#36300,#36301,#36302,
#36303),.UNSPECIFIED.,.F.,.F.,(4,2,2,2,2,2,2,2,2,2,2,2,2,2,2,2,2,2,2,2,
2,2,2,2,2,2,2,2,2,2,2,2,2,2,2,2,2,2,2,2,2,2,2,2,2,2,2,2,2,2,2,2,2,2,2,2,
2,4),(7.6698861386074E-5,0.0253641144717246,0.0500064399592511,0.0982743512795232,
0.144396900860148,0.169754042124687,0.211180728494791,0.233786149641564,
0.259176234358203,0.300717954836437,0.322382035728535,0.347787127447208,
0.389971219681712,0.410351428726807,0.45960754915082,0.506309943404491,
0.532445730872144,0.574944756721432,0.598305762915829,0.624471352988871,
0.667316727791965,0.689646583714177,0.715828165174297,0.759295458119143,
0.780303810677911,0.831065128875955,0.879135074458262,0.931225408976213,
0.984294307137153,1.03610471716903,1.0589297141727,1.10681084378159,1.13379207944822,
1.15842115031494,1.19987899724597,1.22681729209237,1.27791685866676,1.32980038383556,
1.3518321432672,1.39495327783279,1.42141763652019,1.44501563941602,1.48665214587862,
1.5133950465113,1.56269008377841,1.61322123807819,1.63458710491603,1.67669797009781,
1.70246836128344,1.72533098712041,1.76593565513026,1.79198213681011,1.83957602019648,
1.88879043609758,1.90998743513082,1.95065703719148,1.9894885146296,2.02909458871922),
 .UNSPECIFIED.);
#2349=B_SPLINE_CURVE_WITH_KNOTS('',3,(#36306,#36307,#36308,#36309,#36310,
#36311,#36312,#36313,#36314,#36315,#36316,#36317,#36318,#36319,#36320,#36321,
#36322,#36323,#36324,#36325,#36326,#36327,#36328,#36329,#36330,#36331,#36332,
#36333,#36334,#36335,#36336,#36337,#36338,#36339,#36340,#36341,#36342,#36343,
#36344,#36345,#36346,#36347,#36348,#36349,#36350,#36351,#36352,#36353,#36354,
#36355,#36356,#36357,#36358,#36359,#36360,#36361,#36362,#36363,#36364,#36365,
#36366,#36367,#36368,#36369,#36370,#36371,#36372,#36373,#36374,#36375,#36376,
#36377,#36378,#36379,#36380,#36381,#36382,#36383,#36384,#36385,#36386,#36387,
#36388,#36389,#36390,#36391,#36392,#36393,#36394,#36395,#36396,#36397,#36398,
#36399,#36400,#36401,#36402,#36403,#36404,#36405,#36406,#36407,#36408,#36409,
#36410,#36411,#36412,#36413,#36414,#36415,#36416,#36417,#36418,#36419),
 .UNSPECIFIED.,.F.,.F.,(4,2,2,2,2,2,2,2,2,2,2,2,2,2,2,2,2,2,2,2,2,2,2,2,
2,2,2,2,2,2,2,2,2,2,2,2,2,2,2,2,2,2,2,2,2,2,2,2,2,2,2,2,2,2,2,2,4),(5.94831277856605E-5,
0.0316367019428793,0.05994421141559,0.0883769919118876,0.116199833618172,
0.148646117264482,0.185649600266723,0.230767737668117,0.283347520953013,
0.3394418557413,0.383998353924985,0.423502762154574,0.462978744711714,0.502190993058523,
0.550924538583601,0.614750411650344,0.690541644643776,0.777537898685706,
0.891899588386907,0.990239042779026,1.06956304428088,1.13517856125222,1.19303682822286,
1.2513024100045,1.30822288488875,1.37470140207469,1.45052897134019,1.54326735519958,
1.65154718909885,1.75982702299812,1.85256540685745,1.92839297612289,1.99487149330899,
2.05179196819336,2.11005754997495,2.16791581694551,2.23353133391694,2.31285533541884,
2.41119478981148,2.52555647951633,2.61255273356166,2.68834396655795,2.75216983962711,
2.80090338515382,2.84011563350184,2.87959161606014,2.91909602429086,2.96365252247589,
3.0197468572658,3.07232664055213,3.11744477795483,3.15444826095814,3.18689454460537,
3.21471738631243,3.2431501668095,3.27145767628297,3.30303488344564),
 .UNSPECIFIED.);
#2350=B_SPLINE_CURVE_WITH_KNOTS('',3,(#36561,#36562,#36563,#36564,#36565,
#36566,#36567,#36568,#36569,#36570,#36571,#36572,#36573,#36574,#36575,#36576,
#36577,#36578,#36579,#36580,#36581,#36582,#36583,#36584,#36585,#36586,#36587,
#36588,#36589,#36590,#36591,#36592,#36593,#36594,#36595,#36596,#36597,#36598,
#36599,#36600,#36601,#36602,#36603,#36604),.UNSPECIFIED.,.F.,.F.,(4,2,2,
2,2,2,2,2,2,2,2,2,2,2,2,2,2,2,2,2,2,4),(7.68002794356204E-5,0.0287777493485966,
0.0575152407768132,0.106155181951881,0.165514264466246,0.236890561238667,
0.269992967924706,0.342297528574894,0.41385280051629,0.451122206439615,
0.514413059508262,0.57781052913482,0.614649187845566,0.65011886251284,0.714826966817939,
0.751033279270129,0.78582652402978,0.856066631699381,0.929434885992276,
1.00126014577657,1.04560443038775,1.08990031448452),.UNSPECIFIED.);
#2351=B_SPLINE_CURVE_WITH_KNOTS('',3,(#36606,#36607,#36608,#36609,#36610,
#36611,#36612,#36613,#36614,#36615,#36616,#36617,#36618,#36619,#36620,#36621,
#36622,#36623,#36624,#36625,#36626,#36627,#36628,#36629,#36630,#36631,#36632,
#36633,#36634,#36635,#36636,#36637,#36638,#36639,#36640,#36641,#36642,#36643,
#36644,#36645,#36646,#36647,#36648,#36649,#36650,#36651,#36652,#36653,#36654,
#36655,#36656,#36657,#36658,#36659,#36660,#36661,#36662,#36663,#36664,#36665,
#36666,#36667,#36668,#36669,#36670,#36671,#36672,#36673,#36674,#36675,#36676,
#36677,#36678,#36679,#36680,#36681,#36682,#36683,#36684,#36685,#36686,#36687,
#36688,#36689,#36690,#36691,#36692,#36693,#36694,#36695,#36696,#36697,#36698,
#36699,#36700,#36701,#36702,#36703,#36704,#36705,#36706,#36707,#36708,#36709,
#36710,#36711,#36712,#36713,#36714,#36715,#36716,#36717,#36718,#36719),
 .UNSPECIFIED.,.F.,.F.,(4,2,2,2,2,2,2,2,2,2,2,2,2,2,2,2,2,2,2,2,2,2,2,2,
2,2,2,2,2,2,2,2,2,2,2,2,2,2,2,2,2,2,2,2,2,2,2,2,2,2,2,2,2,2,2,2,4),(-3.30303488335142,
-3.27145767619062,-3.24315016671873,-3.21471738622325,-3.18689454451777,
-3.1544482608724,-3.11744477787123,-3.07232664047114,-3.01974685718777,
-2.96365252240111,-2.91909602421871,-2.87959161599026,-2.84011563343427,
-2.8009033850886,-2.75216983956494,-2.68834396650006,-2.61255273350884,
-2.52555647946945,-2.41119478977154,-2.31285533538221,-2.23353133388263,
-2.16791581691316,-2.11005754994417,-2.05179196816421,-1.99487149328159,
-1.92839297609755,-1.85256540683422,-1.75982702297748,-1.65154718908131,
-1.54326735518514,-1.45052897132847,-1.3747014020652,-1.30822288488101,
-1.25130240999827,-1.19303682821834,-1.13517856124945,-1.06956304427989,
-0.990239042780272,-0.891899588390439,-0.777537898688797,-0.690541644645899,
-0.614750411651723,-0.550924538584345,-0.502190993058996,-0.462978744712068,
-0.423502762154865,-0.38399835392525,-0.339441855741458,-0.283347520953114,
-0.230767737668244,-0.185649600266803,-0.148646117264526,-0.1161998336182,
-0.0883769919119069,-0.0599442114156348,-0.0316367019429531,-5.9483127788608E-5),
 .UNSPECIFIED.);
#2352=B_SPLINE_CURVE_WITH_KNOTS('',3,(#36862,#36863,#36864,#36865,#36866,
#36867,#36868,#36869,#36870,#36871,#36872,#36873,#36874,#36875,#36876,#36877,
#36878,#36879,#36880,#36881,#36882,#36883,#36884,#36885,#36886,#36887,#36888,
#36889,#36890,#36891,#36892,#36893,#36894,#36895,#36896,#36897,#36898,#36899,
#36900,#36901,#36902,#36903,#36904,#36905,#36906,#36907,#36908,#36909,#36910,
#36911,#36912,#36913,#36914,#36915,#36916,#36917,#36918,#36919,#36920,#36921,
#36922,#36923,#36924,#36925,#36926,#36927,#36928,#36929,#36930,#36931,#36932,
#36933,#36934,#36935,#36936,#36937,#36938,#36939,#36940,#36941,#36942,#36943,
#36944,#36945,#36946,#36947,#36948,#36949,#36950,#36951,#36952,#36953,#36954,
#36955,#36956,#36957,#36958,#36959,#36960,#36961,#36962,#36963,#36964,#36965,
#36966,#36967,#36968,#36969,#36970,#36971,#36972,#36973,#36974,#36975,#36976,
#36977,#36978,#36979,#36980,#36981),.UNSPECIFIED.,.F.,.F.,(4,2,2,2,2,2,
2,2,2,2,2,2,2,2,2,2,2,2,2,2,2,2,2,2,2,2,2,2,2,2,2,2,2,2,2,2,2,2,2,2,2,2,
2,2,2,2,2,2,2,2,2,2,2,2,2,2,2,2,2,4),(4.0051248426754E-5,0.0342064761731191,
0.0631175860317564,0.0925901191772445,0.109204719988194,0.127579480307699,
0.157809813748144,0.17343819129591,0.191827601357051,0.222340229122194,
0.237083590647375,0.272737092201538,0.306595004693092,0.325515137613875,
0.356273057630785,0.373228961128414,0.392171250118677,0.423164564769037,
0.439399493407582,0.458354387574874,0.489781306563202,0.505067114058951,
0.541814948000685,0.576121524170463,0.595585940952813,0.627358776285785,
0.644284692241037,0.663765570017339,0.695920050526438,0.705048117245191,
0.742539832779656,0.761952372673167,0.779181946526965,0.809783461597958,
0.829402822794386,0.865434106670318,0.902572827052802,0.918291063237675,
0.949218481843105,0.968159729435232,0.984979059868996,1.01483166754968,
1.03397445379827,1.06914541132536,1.10537577037675,1.12070664338408,1.15088038093645,
1.16935823240658,1.18576522071897,1.21489233668997,1.23356698054014,1.26788472670369,
1.30323601192855,1.31813615732139,1.34767715894864,1.36570095301968,1.38194088462811,
1.41018067834471,1.43900555726746,1.47288628947006),.UNSPECIFIED.);
#2353=B_SPLINE_CURVE_WITH_KNOTS('',3,(#36984,#36985,#36986,#36987,#36988,
#36989,#36990,#36991,#36992,#36993,#36994,#36995,#36996,#36997,#36998,#36999,
#37000,#37001,#37002,#37003,#37004,#37005,#37006,#37007,#37008,#37009,#37010,
#37011,#37012,#37013,#37014,#37015,#37016,#37017,#37018,#37019,#37020,#37021,
#37022,#37023,#37024,#37025,#37026,#37027,#37028,#37029,#37030,#37031,#37032,
#37033,#37034,#37035,#37036,#37037,#37038,#37039,#37040,#37041,#37042,#37043,
#37044,#37045,#37046,#37047,#37048,#37049,#37050,#37051,#37052,#37053,#37054,
#37055,#37056,#37057,#37058,#37059,#37060,#37061,#37062,#37063,#37064,#37065,
#37066,#37067,#37068,#37069,#37070,#37071,#37072,#37073,#37074,#37075,#37076,
#37077,#37078,#37079,#37080,#37081,#37082,#37083,#37084,#37085,#37086,#37087,
#37088,#37089,#37090,#37091,#37092,#37093,#37094,#37095,#37096,#37097),
 .UNSPECIFIED.,.F.,.F.,(4,2,2,2,2,2,2,2,2,2,2,2,2,2,2,2,2,2,2,2,2,2,2,2,
2,2,2,2,2,2,2,2,2,2,2,2,2,2,2,2,2,2,2,2,2,2,2,2,2,2,2,2,2,2,2,2,4),(5.94831277915571E-5,
0.0316367019429085,0.0599442114156052,0.0883769919118883,0.116199833618177,
0.148646117264504,0.185649600266749,0.230767737668142,0.283347520952984,
0.339441855741318,0.383998353925107,0.423502762154725,0.462978744712151,
0.502190993059384,0.550924538585165,0.614750411653649,0.690541644649133,
0.777537898693328,0.891899588396945,0.99023904278927,1.069563044291,1.1351785612623,
1.19303682823281,1.25130241001434,1.30822288489854,1.37470140208444,1.45052897134983,
1.54326735520912,1.65154718910821,1.7598270230073,1.85256540686662,1.92839297613204,
1.99487149331798,2.05179196820223,2.11005754998372,2.1679158169542,2.23353133392551,
2.31285533542727,2.41119478981956,2.52555647952189,2.61255273356476,2.68834396655906,
2.75216983962656,2.80090338515208,2.84011563349924,2.87959161605671,2.9190960242866,
2.96365252247078,3.01974685725952,3.07232664054471,3.11744477794648,3.15444826094903,
3.18689454459555,3.21471738630203,3.24315016679852,3.27145767627144,3.30303488343336),
 .UNSPECIFIED.);
#2354=B_SPLINE_CURVE_WITH_KNOTS('',3,(#37239,#37240,#37241,#37242,#37243,
#37244,#37245,#37246,#37247,#37248,#37249,#37250,#37251,#37252,#37253,#37254,
#37255,#37256,#37257,#37258,#37259,#37260,#37261,#37262,#37263,#37264,#37265,
#37266,#37267,#37268,#37269,#37270,#37271,#37272,#37273,#37274,#37275,#37276,
#37277,#37278,#37279,#37280,#37281,#37282,#37283,#37284),.UNSPECIFIED.,
 .F.,.F.,(4,2,2,2,2,2,2,2,2,2,2,2,2,2,2,2,2,2,2,2,2,2,4),(4.00913729709594E-5,
0.0255224163009285,0.0506628404716964,0.0675638222751209,0.115459262979836,
0.139046414941069,0.163661762441637,0.209957952667681,0.234239146303838,
0.282831016253925,0.306172802073132,0.357736918849856,0.385227490793403,
0.411763916933472,0.463568750602167,0.51847542001774,0.571406026873824,
0.625515387332744,0.679017081593755,0.731021185439546,0.784186981559513,
0.809198205683984,0.834926852586118),.UNSPECIFIED.);
#2355=B_SPLINE_CURVE_WITH_KNOTS('',3,(#37286,#37287,#37288,#37289,#37290,
#37291,#37292,#37293,#37294,#37295,#37296,#37297,#37298,#37299,#37300,#37301,
#37302,#37303,#37304,#37305,#37306,#37307,#37308,#37309,#37310,#37311,#37312,
#37313,#37314,#37315,#37316,#37317,#37318,#37319,#37320,#37321,#37322,#37323,
#37324,#37325,#37326,#37327,#37328,#37329,#37330,#37331,#37332,#37333,#37334,
#37335,#37336,#37337,#37338,#37339,#37340,#37341,#37342,#37343,#37344,#37345,
#37346,#37347,#37348,#37349,#37350,#37351,#37352,#37353,#37354,#37355,#37356,
#37357,#37358,#37359,#37360,#37361,#37362,#37363,#37364,#37365,#37366,#37367,
#37368,#37369,#37370,#37371,#37372,#37373,#37374,#37375,#37376,#37377,#37378,
#37379,#37380,#37381,#37382,#37383,#37384,#37385,#37386,#37387,#37388,#37389,
#37390,#37391,#37392,#37393,#37394,#37395,#37396,#37397,#37398,#37399),
 .UNSPECIFIED.,.F.,.F.,(4,2,2,2,2,2,2,2,2,2,2,2,2,2,2,2,2,2,2,2,2,2,2,2,
2,2,2,2,2,2,2,2,2,2,2,2,2,2,2,2,2,2,2,2,2,2,2,2,2,2,2,2,2,2,2,2,4),(-3.30303488340775,
-3.27145767624626,-3.24315016677379,-3.21471738627774,-3.18689454457167,
-3.15444826092561,-3.11744477792366,-3.07232664052264,-3.01974685723822,
-2.96365252245034,-2.91909602426692,-2.87959161603762,-2.84011563348052,
-2.80090338513361,-2.75216983960824,-2.68834396654031,-2.61255273354548,
-2.52555647950205,-2.4111947897994,-2.31285533540785,-2.23353133390672,
-2.16791581693593,-2.11005754996586,-2.05179196818478,-1.99487149330102,
-1.92839297611563,-1.85256540685082,-1.75982702299225,-1.65154718909399,
-1.54326735519573,-1.45052897133712,-1.37470140207228,-1.30822288488685,
-1.25130241000305,-1.19303682822201,-1.13517856125197,-1.06956304428115,
-0.990239042780001,-0.891899588388456,-0.777537898686937,-0.690541644644683,
-0.614750411650919,-0.550924538583876,-0.502190993058717,-0.462978744711846,
-0.423502762154673,-0.383998353925072,-0.339441855741231,-0.283347520952903,
-0.230767737668099,-0.18564960026667,-0.148646117264394,-0.11619983361811,
-0.0883769919118416,-0.0599442114155554,-0.0316367019428531,-5.94831277862293E-5),
 .UNSPECIFIED.);
#2356=B_SPLINE_CURVE_WITH_KNOTS('',3,(#37542,#37543,#37544,#37545,#37546,
#37547,#37548,#37549,#37550,#37551,#37552,#37553,#37554,#37555,#37556,#37557,
#37558,#37559,#37560,#37561,#37562,#37563,#37564,#37565,#37566,#37567,#37568,
#37569,#37570,#37571,#37572,#37573,#37574,#37575,#37576,#37577,#37578,#37579,
#37580,#37581,#37582,#37583,#37584,#37585,#37586,#37587,#37588,#37589,#37590,
#37591,#37592,#37593,#37594,#37595,#37596,#37597,#37598,#37599,#37600,#37601,
#37602,#37603,#37604,#37605,#37606,#37607,#37608,#37609,#37610,#37611,#37612,
#37613,#37614,#37615,#37616,#37617,#37618,#37619,#37620,#37621,#37622,#37623,
#37624,#37625,#37626,#37627,#37628,#37629,#37630,#37631,#37632,#37633,#37634,
#37635,#37636,#37637,#37638,#37639,#37640,#37641,#37642,#37643,#37644,#37645,
#37646,#37647,#37648,#37649,#37650,#37651,#37652,#37653,#37654,#37655),
 .UNSPECIFIED.,.F.,.F.,(4,2,2,2,2,2,2,2,2,2,2,2,2,2,2,2,2,2,2,2,2,2,2,2,
2,2,2,2,2,2,2,2,2,2,2,2,2,2,2,2,2,2,2,2,2,2,2,2,2,2,2,2,2,2,2,2,4),(7.66667039813964E-5,
0.0343822570135638,0.0637613764833492,0.094199059661914,0.11047498602631,
0.12930195093692,0.160694844424638,0.175767290920764,0.212272713042494,
0.246749040585014,0.266102424593384,0.297603712513506,0.314777680002683,
0.334151582098445,0.365942900382604,0.382292601247752,0.401675502261559,
0.433971521537711,0.449330739706536,0.486917336364386,0.524517255803242,
0.562773220070549,0.602183403859061,0.639402116718175,0.679257550990186,
0.714264232281347,0.728825399703001,0.748794148989186,0.788083652792557,
0.804416787023143,0.837512446363635,0.857536416517704,0.874909500560555,
0.906807390286947,0.927057081979138,0.96346744856945,1.00205549387321,1.01846649219655,
1.05050898548041,1.07019271009353,1.08777765812595,1.11872228788031,1.13861213663028,
1.17533033601046,1.21288546357669,1.2287576670532,1.26006322092035,1.27921565891491,
1.29619753766833,1.32638200672507,1.34573993774699,1.38109560231843,1.41768017926844,
1.43343946269429,1.46366967964336,1.49253830141179,1.52198322200782),
 .UNSPECIFIED.);
#2357=B_SPLINE_CURVE_WITH_KNOTS('',3,(#37658,#37659,#37660,#37661,#37662,
#37663,#37664,#37665,#37666,#37667,#37668,#37669,#37670,#37671,#37672,#37673,
#37674,#37675,#37676,#37677,#37678,#37679,#37680,#37681,#37682,#37683,#37684,
#37685,#37686,#37687,#37688,#37689,#37690,#37691,#37692,#37693,#37694,#37695,
#37696,#37697,#37698,#37699,#37700,#37701,#37702,#37703,#37704,#37705,#37706,
#37707,#37708,#37709,#37710,#37711,#37712,#37713,#37714,#37715,#37716,#37717,
#37718,#37719,#37720,#37721,#37722,#37723,#37724,#37725,#37726,#37727,#37728,
#37729,#37730,#37731,#37732,#37733,#37734,#37735,#37736,#37737,#37738,#37739,
#37740,#37741,#37742,#37743,#37744,#37745,#37746,#37747,#37748,#37749,#37750,
#37751,#37752,#37753,#37754,#37755,#37756,#37757,#37758,#37759,#37760,#37761,
#37762,#37763,#37764,#37765,#37766,#37767,#37768,#37769,#37770,#37771),
 .UNSPECIFIED.,.F.,.F.,(4,2,2,2,2,2,2,2,2,2,2,2,2,2,2,2,2,2,2,2,2,2,2,2,
2,2,2,2,2,2,2,2,2,2,2,2,2,2,2,2,2,2,2,2,2,2,2,2,2,2,2,2,2,2,2,2,4),(4.94894020204337E-5,
0.0316314923673886,0.0599439530140688,0.0883817065950881,0.116209414703643,
0.148661373423333,0.185671328583896,0.230797357451291,0.28338633729426,
0.339490483359371,0.384054774774603,0.423566092591166,0.463048979763645,
0.502268086597013,0.551010155947864,0.614847192590904,0.690651681982884,
0.777663152257347,0.892044844589388,0.990401499212093,1.06973937501396,
1.1353663685795,1.19323475534907,1.25151052817173,1.30844095882898,1.37493110355368,
1.45077193556961,1.54352653999428,1.65182531276284,1.76012408553141,1.85287868995618,
1.92871952197216,1.99520966669679,2.05214009735399,2.11041587017671,2.16828425694633,
2.23391125051183,2.31324912631368,2.41160578093638,2.52598747326715,2.61299894354021,
2.68880343293115,2.75264046957332,2.80138253892366,2.84060164575671,2.88008453292891,
2.91959585074528,2.9641601421603,3.0202642882251,3.07285326806776,3.11797929693492,
3.15498925209528,3.18744121081486,3.21526891892331,3.24370667250417,3.27201913315071,
3.3036018633784),.UNSPECIFIED.);
#2358=B_SPLINE_CURVE_WITH_KNOTS('',3,(#37913,#37914,#37915,#37916,#37917,
#37918,#37919,#37920,#37921,#37922,#37923,#37924,#37925,#37926,#37927,#37928,
#37929,#37930,#37931,#37932,#37933,#37934,#37935,#37936,#37937,#37938,#37939,
#37940,#37941,#37942,#37943,#37944,#37945,#37946,#37947,#37948,#37949,#37950,
#37951,#37952,#37953,#37954,#37955,#37956),.UNSPECIFIED.,.F.,.F.,(4,2,2,
2,2,2,2,2,2,2,2,2,2,2,2,2,2,2,2,2,2,4),(6.66069981017537E-5,0.0257114809926198,
0.0510662466252859,0.0996676030717527,0.136326971149926,0.165900839293608,
0.203535749058119,0.253888941376676,0.278755475981711,0.304647335999316,
0.354681677934622,0.366819850806871,0.413020641579737,0.438815758028813,
0.463596322699854,0.5135634301164,0.550658857331488,0.579591342752336,0.614849419992928,
0.659933842154479,0.683662933835049,0.707689106989728),.UNSPECIFIED.);
#2359=B_SPLINE_CURVE_WITH_KNOTS('',3,(#37958,#37959,#37960,#37961,#37962,
#37963,#37964,#37965,#37966,#37967,#37968,#37969,#37970,#37971,#37972,#37973,
#37974,#37975,#37976,#37977,#37978,#37979,#37980,#37981,#37982,#37983,#37984,
#37985,#37986,#37987,#37988,#37989,#37990,#37991,#37992,#37993,#37994,#37995,
#37996,#37997,#37998,#37999,#38000,#38001,#38002,#38003,#38004,#38005,#38006,
#38007,#38008,#38009,#38010,#38011,#38012,#38013,#38014,#38015,#38016,#38017,
#38018,#38019,#38020,#38021,#38022,#38023,#38024,#38025,#38026,#38027,#38028,
#38029,#38030,#38031,#38032,#38033,#38034,#38035,#38036,#38037,#38038,#38039,
#38040,#38041,#38042,#38043,#38044,#38045,#38046,#38047,#38048,#38049,#38050,
#38051,#38052,#38053,#38054,#38055,#38056,#38057,#38058,#38059,#38060,#38061,
#38062,#38063,#38064,#38065,#38066,#38067,#38068,#38069,#38070,#38071),
 .UNSPECIFIED.,.F.,.F.,(4,2,2,2,2,2,2,2,2,2,2,2,2,2,2,2,2,2,2,2,2,2,2,2,
2,2,2,2,2,2,2,2,2,2,2,2,2,2,2,2,2,2,2,2,2,2,2,2,2,2,2,2,2,2,2,2,4),(-3.30303418879995,
-3.27145767624004,-3.24315016676724,-3.21471738627084,-3.18689454456452,
-3.15444826091816,-3.11744477791575,-3.07232664051416,-3.01974685722908,
-2.96365252244057,-2.91909602425668,-2.87959161602693,-2.84011563346943,
-2.80090338512216,-2.75216983959636,-2.68834396652805,-2.61255273353278,
-2.52555647948861,-2.4111947897857,-2.31285533539524,-2.23353133389494,
-2.16791581692479,-2.11005754995539,-2.051791968175,-1.99487149329178,-1.92839297610701,
-1.85256540684313,-1.75982702298575,-1.65154718908867,-1.54326735519157,
-1.45052897133412,-1.37470140207019,-1.30822288488551,-1.25130241000235,
-1.19303682822191,-1.13517856125246,-1.06956304428236,-0.990239042782088,
-0.891899588391592,-0.777537898689638,-0.690541644646586,-0.614750411652103,
-0.550924538584464,-0.502190993059046,-0.462978744712006,-0.423502762154696,
-0.383998353925075,-0.339441855741319,-0.283347520953013,-0.230767737668155,
-0.185649600266737,-0.148646117264472,-0.116199833618172,-0.0883769919118998,
-0.0599442114156078,-0.0316367019429014,-5.94831277983696E-5),
 .UNSPECIFIED.);
#2360=B_SPLINE_CURVE_WITH_KNOTS('',3,(#38214,#38215,#38216,#38217,#38218,
#38219,#38220,#38221,#38222,#38223,#38224,#38225,#38226,#38227,#38228,#38229,
#38230,#38231,#38232,#38233,#38234,#38235,#38236,#38237,#38238,#38239,#38240,
#38241,#38242,#38243,#38244,#38245,#38246,#38247,#38248,#38249,#38250,#38251,
#38252,#38253,#38254,#38255,#38256,#38257,#38258,#38259,#38260,#38261,#38262,
#38263,#38264,#38265,#38266,#38267,#38268,#38269,#38270,#38271,#38272,#38273,
#38274,#38275,#38276,#38277,#38278,#38279,#38280,#38281,#38282,#38283,#38284,
#38285,#38286,#38287,#38288,#38289,#38290,#38291,#38292,#38293,#38294,#38295,
#38296,#38297,#38298,#38299,#38300,#38301,#38302,#38303,#38304,#38305,#38306,
#38307,#38308,#38309,#38310,#38311),.UNSPECIFIED.,.F.,.F.,(4,2,2,2,2,2,
2,2,2,2,2,2,2,2,2,2,2,2,2,2,2,2,2,2,2,2,2,2,2,2,2,2,2,2,2,2,2,2,2,2,2,2,
2,2,2,2,2,2,4),(6.66228729229431E-5,0.0225476992818617,0.0442896901705524,
0.0591711937710805,0.104450063255743,0.134337450528061,0.15508110800453,
0.175912746947078,0.196048962747963,0.22351804937836,0.244541747565316,
0.27188301377946,0.294089951435767,0.316542973695342,0.336496597886517,
0.343517373123556,0.352726143951829,0.362515304186564,0.370161375413743,
0.377077685058301,0.387290271145451,0.404658951155952,0.423205010581693,
0.44195805752164,0.464515615946775,0.480911330011926,0.503550191581656,
0.527051081788821,0.54294486906486,0.578085257945204,0.599501605476778,
0.619019564203727,0.639300414853292,0.668132715757297,0.696074102483784,
0.717738403103488,0.728524348566846,0.739821161329477,0.750855444682612,
0.764498264544529,0.779141577748808,0.790310292685832,0.80307257247109,
0.818064081166539,0.837091745472003,0.848407593361733,0.859726051869667,
0.873284898580614,0.886799076579605),.UNSPECIFIED.);
#2361=B_SPLINE_CURVE_WITH_KNOTS('',3,(#38313,#38314,#38315,#38316,#38317,
#38318,#38319,#38320,#38321,#38322,#38323,#38324,#38325,#38326,#38327,#38328,
#38329,#38330,#38331,#38332,#38333,#38334,#38335,#38336,#38337,#38338),
 .UNSPECIFIED.,.F.,.F.,(4,2,2,2,2,2,2,2,2,2,2,2,4),(-0.349172101168083,
-0.30613774295609,-0.268493936474377,-0.249567397365854,-0.230355139827257,
-0.209628324386868,-0.191150939236384,-0.149007240432192,-0.117442311272233,
-0.0928116777959336,-0.0725064298073674,-0.0362198133233974,-2.55123851692849E-6),
 .UNSPECIFIED.);
#2362=B_SPLINE_CURVE_WITH_KNOTS('',3,(#38340,#38341,#38342,#38343,#38344,
#38345,#38346,#38347,#38348,#38349,#38350,#38351,#38352,#38353,#38354,#38355),
 .UNSPECIFIED.,.F.,.F.,(4,2,2,2,2,2,2,4),(-0.211885266973906,-0.196996598406475,
-0.181637026962749,-0.152787959014052,-0.117981173952917,-0.0783349442213858,
-0.0396812097311858,-3.20864029342772E-5),.UNSPECIFIED.);
#2363=B_SPLINE_CURVE_WITH_KNOTS('',3,(#38356,#38357,#38358,#38359,#38360,
#38361,#38362,#38363,#38364,#38365,#38366,#38367,#38368,#38369,#38370,#38371,
#38372,#38373,#38374,#38375,#38376,#38377,#38378,#38379,#38380,#38381,#38382,
#38383,#38384,#38385,#38386,#38387,#38388,#38389,#38390,#38391,#38392,#38393,
#38394,#38395,#38396,#38397,#38398,#38399,#38400,#38401,#38402,#38403,#38404,
#38405,#38406,#38407,#38408,#38409,#38410,#38411,#38412,#38413,#38414,#38415,
#38416,#38417,#38418,#38419,#38420,#38421,#38422,#38423,#38424,#38425,#38426,
#38427,#38428,#38429,#38430,#38431,#38432,#38433,#38434,#38435,#38436,#38437,
#38438,#38439,#38440,#38441,#38442,#38443,#38444,#38445,#38446,#38447,#38448,
#38449,#38450,#38451,#38452,#38453,#38454,#38455,#38456,#38457,#38458,#38459,
#38460,#38461,#38462,#38463,#38464,#38465,#38466,#38467,#38468,#38469,#38470,
#38471,#38472,#38473,#38474,#38475,#38476,#38477,#38478,#38479,#38480,#38481,
#38482,#38483,#38484,#38485,#38486,#38487,#38488,#38489,#38490,#38491,#38492,
#38493,#38494,#38495,#38496,#38497,#38498,#38499,#38500,#38501,#38502,#38503,
#38504,#38505,#38506,#38507,#38508,#38509,#38510,#38511,#38512,#38513,#38514,
#38515,#38516,#38517,#38518,#38519,#38520,#38521,#38522,#38523,#38524,#38525,
#38526,#38527,#38528,#38529,#38530,#38531,#38532,#38533,#38534,#38535,#38536,
#38537,#38538,#38539,#38540,#38541,#38542,#38543,#38544,#38545,#38546,#38547,
#38548,#38549,#38550,#38551),.UNSPECIFIED.,.F.,.F.,(4,2,2,2,2,2,2,2,2,2,
2,2,2,2,2,2,2,2,2,2,2,2,2,2,2,2,2,2,2,2,2,2,2,2,2,2,2,2,2,2,2,2,2,2,2,2,
2,2,2,2,2,2,2,2,2,2,2,2,2,2,2,2,2,2,2,2,2,2,2,2,2,2,2,2,2,2,2,2,2,2,2,2,
2,2,2,2,2,2,2,2,2,2,2,2,2,2,2,4),(0.000122652419997842,0.0276557142056561,
0.0548465532433756,0.0813319888533599,0.103445171604568,0.115816501830552,
0.122915814684137,0.135255605630576,0.140319560704333,0.14744633344284,
0.154191750101741,0.161382504212589,0.164946904823102,0.174356942050893,
0.17879527499184,0.184043768051259,0.188461477252554,0.192304551229565,
0.199594960441583,0.203034163875464,0.208670143610847,0.214717929164853,
0.222418730236186,0.225925018803337,0.235374252774503,0.239404309627104,
0.245544517663036,0.249502270007744,0.255205166531046,0.261251781907313,
0.266952340527656,0.272380500394639,0.281162721812626,0.289183682462574,
0.294722045602088,0.308694051842449,0.322765635411611,0.336572747895524,
0.344022753864475,0.356156366722283,0.364519285824678,0.370402346202873,
0.379037801767753,0.385001889576374,0.389757098712872,0.394272191758983,
0.40215252660916,0.407307790504656,0.410686758612044,0.417787992809562,
0.423400397500185,0.429613164782095,0.435329819529971,0.441713614987118,
0.444955924424928,0.451603094281047,0.456621478459793,0.464872671209544,
0.469666978601246,0.475175342349373,0.482934363353185,0.491739297739543,
0.496324515501596,0.503324561292956,0.516467205564147,0.52342352311931,
0.537228833926293,0.544092313574322,0.55745794089263,0.571067445650911,
0.5853212861971,0.590748042360905,0.595676057995859,0.602648937952715,0.608041695946353,
0.612019344091071,0.618008163606214,0.621609774966156,0.629401051040114,
0.633758561165747,0.640694591247517,0.644435352788924,0.64916605878867,
0.653981150987846,0.660154578341861,0.667158608840516,0.672437143489509,
0.678316991527251,0.68272216058364,0.69232166733335,0.696306656105387,0.702984169138243,
0.71012576320964,0.71727759998328,0.722900094763324,0.731656752166302,0.742171028011585,
0.755579756858543),.UNSPECIFIED.);
#2364=B_SPLINE_CURVE_WITH_KNOTS('',3,(#38693,#38694,#38695,#38696,#38697,
#38698,#38699,#38700,#38701,#38702,#38703,#38704,#38705,#38706,#38707,#38708,
#38709,#38710,#38711,#38712,#38713,#38714,#38715,#38716,#38717,#38718,#38719,
#38720,#38721,#38722,#38723,#38724,#38725,#38726,#38727,#38728,#38729,#38730,
#38731,#38732,#38733,#38734,#38735,#38736,#38737,#38738,#38739,#38740,#38741,
#38742,#38743,#38744,#38745,#38746,#38747,#38748,#38749,#38750,#38751,#38752,
#38753,#38754,#38755,#38756,#38757,#38758,#38759,#38760,#38761,#38762,#38763,
#38764,#38765,#38766,#38767,#38768,#38769,#38770,#38771,#38772,#38773,#38774,
#38775,#38776,#38777,#38778,#38779,#38780,#38781,#38782,#38783,#38784,#38785,
#38786,#38787,#38788,#38789,#38790,#38791,#38792,#38793,#38794,#38795,#38796,
#38797,#38798,#38799,#38800,#38801,#38802,#38803,#38804,#38805,#38806,#38807,
#38808,#38809,#38810,#38811,#38812,#38813,#38814,#38815,#38816,#38817,#38818,
#38819,#38820,#38821,#38822,#38823,#38824,#38825,#38826,#38827,#38828,#38829,
#38830,#38831,#38832,#38833,#38834,#38835,#38836,#38837,#38838,#38839,#38840,
#38841,#38842,#38843,#38844,#38845,#38846,#38847,#38848,#38849,#38850,#38851,
#38852,#38853,#38854),.UNSPECIFIED.,.F.,.F.,(4,2,2,2,2,2,2,2,2,2,2,2,2,
2,2,2,2,2,2,2,2,2,2,2,2,2,2,2,2,2,2,2,2,2,2,2,2,2,2,2,2,2,2,2,2,2,2,2,2,
2,2,2,2,2,2,2,2,2,2,2,2,2,2,2,2,2,2,2,2,2,2,2,2,2,2,2,2,2,2,2,4),(-4.07132161405629,
-4.00254204476235,-3.94917628400674,-3.86795081813188,-3.79332164531464,
-3.74072831013231,-3.68013965831211,-3.62552568967953,-3.56801317961879,
-3.52417666717784,-3.44856266284831,-3.40540846135397,-3.32669109777936,
-3.23487237385695,-3.13850440833536,-3.08645769787531,-3.05261484298801,
-2.96563410991923,-2.91656098005686,-2.86751731174139,-2.75489628469704,
-2.63126531072298,-2.513177710874,-2.38918165075726,-2.29341735780137,-2.23088977537095,
-2.19395315434401,-2.15469465057632,-2.09719660594431,-2.06819801622426,
-2.02951834482612,-1.98366456753363,-1.95300592485793,-1.91770365730641,
-1.88548048679027,-1.85188758413217,-1.82623395367009,-1.79604688936397,
-1.76674581938805,-1.7355621004847,-1.70471705422878,-1.66878201729108,
-1.64442858220071,-1.60296803607516,-1.56376092859971,-1.53634240109056,
-1.47445473086875,-1.37923891142332,-1.29995519569865,-1.18058216401935,
-1.06184737759313,-0.948750431355718,-0.863398080645727,-0.798764826289785,
-0.776013241654084,-0.742153628487462,-0.708920662731534,-0.672900978419029,
-0.647342028991442,-0.59047469202054,-0.565959615586883,-0.532894643003156,
-0.498221639823335,-0.474840364742629,-0.446916707542781,-0.420111565412746,
-0.392838466973543,-0.361655184901136,-0.336878232420111,-0.317827718572486,
-0.28935652060261,-0.247826078558967,-0.223680401877466,-0.186986046828687,
-0.144119788584455,-0.131147823980291,-0.110060597497317,-0.0909381017436983,
-0.0676719087717867,-0.0340691893263995,-4.90219995722183E-5),
 .UNSPECIFIED.);
#2365=B_SPLINE_CURVE_WITH_KNOTS('',3,(#38855,#38856,#38857,#38858,#38859,
#38860,#38861,#38862,#38863,#38864,#38865,#38866,#38867,#38868),
 .UNSPECIFIED.,.F.,.F.,(4,2,2,2,2,2,4),(-0.122023436879687,-0.106448133343434,
-0.0921171939725468,-0.0737837856348753,-0.0478286240892578,-0.0261030661831481,
-1.94845283136557E-5),.UNSPECIFIED.);
#2366=B_SPLINE_CURVE_WITH_KNOTS('',3,(#38870,#38871,#38872,#38873,#38874,
#38875,#38876,#38877,#38878,#38879,#38880,#38881,#38882,#38883,#38884,#38885,
#38886,#38887,#38888,#38889,#38890,#38891,#38892,#38893,#38894,#38895,#38896,
#38897,#38898,#38899,#38900,#38901,#38902,#38903,#38904,#38905,#38906,#38907,
#38908,#38909,#38910,#38911,#38912,#38913,#38914,#38915,#38916,#38917,#38918,
#38919,#38920,#38921,#38922,#38923,#38924,#38925,#38926,#38927,#38928,#38929,
#38930,#38931,#38932,#38933,#38934,#38935,#38936,#38937,#38938,#38939,#38940,
#38941,#38942,#38943,#38944,#38945,#38946,#38947,#38948),.UNSPECIFIED.,
 .F.,.F.,(4,3,3,3,3,3,3,3,3,3,3,3,3,3,3,3,3,3,3,3,3,3,3,3,3,3,4),(7.95863275788224E-5,
0.064551352652461,0.117854587835117,0.177729271849115,0.21074324143075,
0.260240782777837,0.30320069554456,0.357169753186396,0.404857781481859,
0.448155184829136,0.47909625451946,0.503910515180243,0.546919912939329,
0.570033569021481,0.608240220497836,0.649721217879779,0.683507534352941,
0.706246676627233,0.758819622585974,0.79057152095178,0.813334638529592,
0.857858751710615,0.880864688605644,0.904150315147694,0.944593770952623,
0.985288372137794,0.99955530932234),.UNSPECIFIED.);
#2367=B_SPLINE_CURVE_WITH_KNOTS('',3,(#39794,#39795,#39796,#39797,#39798,
#39799),.UNSPECIFIED.,.F.,.F.,(4,2,4),(-0.0127260790025929,-0.00639347718755023,
-5.76939431744538E-5),.UNSPECIFIED.);
#2368=B_SPLINE_CURVE_WITH_KNOTS('',3,(#39908,#39909,#39910,#39911,#39912,
#39913,#39914,#39915,#39916,#39917,#39918),.UNSPECIFIED.,.F.,.F.,(4,1,1,
1,1,1,1,1,4),(1.74506463504632E-7,0.125,0.25,0.375,0.5,0.625,0.75,0.875,
1.),.UNSPECIFIED.);
#2369=B_SPLINE_CURVE_WITH_KNOTS('',3,(#39949,#39950,#39951,#39952,#39953,
#39954,#39955,#39956,#39957,#39958,#39959,#39960,#39961,#39962,#39963,#39964,
#39965,#39966,#39967,#39968),.UNSPECIFIED.,.F.,.F.,(4,2,2,2,2,2,2,2,2,4),
(-0.419307317134397,-0.376446924920619,-0.33249018087809,-0.280553953647668,
-0.23721700391194,-0.211165835567419,-0.176188829306431,-0.103876860558225,
-0.0598885228554427,-7.92473299855586E-5),.UNSPECIFIED.);
#2370=B_SPLINE_CURVE_WITH_KNOTS('',3,(#39971,#39972,#39973,#39974,#39975,
#39976,#39977,#39978,#39979,#39980,#39981,#39982,#39983,#39984,#39985,#39986,
#39987,#39988,#39989,#39990,#39991,#39992,#39993,#39994,#39995,#39996,#39997,
#39998,#39999,#40000,#40001,#40002,#40003,#40004,#40005,#40006,#40007,#40008,
#40009,#40010,#40011,#40012,#40013,#40014,#40015,#40016,#40017,#40018,#40019,
#40020,#40021,#40022,#40023,#40024,#40025,#40026,#40027,#40028,#40029,#40030,
#40031,#40032,#40033,#40034,#40035,#40036,#40037,#40038,#40039,#40040,#40041,
#40042,#40043,#40044,#40045,#40046,#40047,#40048,#40049,#40050,#40051,#40052,
#40053,#40054,#40055,#40056,#40057,#40058,#40059,#40060,#40061,#40062,#40063,
#40064),.UNSPECIFIED.,.F.,.F.,(4,2,2,2,2,2,2,2,2,2,2,2,2,2,2,2,2,2,2,2,
2,2,2,2,2,2,2,2,2,2,2,2,2,2,2,2,2,2,2,2,2,2,2,2,2,2,4),(-2.51522491911469,
-2.43371628670848,-2.40614105864553,-2.35503484951906,-2.3067707648452,
-2.26453305057241,-2.20227928383436,-2.16148265557214,-2.13390997902887,
-2.08957850490265,-2.03646371047655,-1.9919948120233,-1.92062186138243,
-1.88521373290542,-1.85899856608694,-1.81624253543225,-1.76404253816429,
-1.72004994921576,-1.64679859763786,-1.61217885105375,-1.58623349108635,
-1.5444488533066,-1.49182130376262,-1.44768968772001,-1.37404101789524,
-1.33957277358892,-1.31365851369137,-1.25749939461323,-1.19246119704988,
-1.14800016017443,-1.09411985945728,-1.05158498284418,-1.02338208188437,
-0.98085216957734,-0.921983788777027,-0.878231883102996,-0.827079325501673,
-0.7819718511449,-0.755826821261395,-0.720496555599507,-0.649110885847386,
-0.60522036792117,-0.553537634951159,-0.509637222343958,-0.483557930911433,
-0.448474158791355,-0.419307317134397),.UNSPECIFIED.);
#2371=B_SPLINE_CURVE_WITH_KNOTS('',3,(#40067,#40068,#40069,#40070,#40071,
#40072,#40073,#40074,#40075,#40076,#40077,#40078,#40079,#40080),
 .UNSPECIFIED.,.F.,.F.,(4,2,2,2,2,2,4),(0.000102940691851845,0.105922775754071,
0.210135463685387,0.343012105338019,0.449458054020239,0.527761272578075,
0.61650116285291),.UNSPECIFIED.);
#2372=B_SPLINE_CURVE_WITH_KNOTS('',3,(#40082,#40083,#40084,#40085,#40086,
#40087,#40088,#40089,#40090,#40091,#40092,#40093,#40094,#40095),
 .UNSPECIFIED.,.F.,.F.,(4,2,2,2,2,2,4),(5.24774905396007E-5,0.102919223275153,
0.200207974164601,0.331136583215735,0.463939911457513,0.553292170439522,
0.637797491354806),.UNSPECIFIED.);
#2373=B_SPLINE_CURVE_WITH_KNOTS('',3,(#40096,#40097,#40098,#40099,#40100,
#40101,#40102,#40103,#40104,#40105,#40106,#40107,#40108,#40109,#40110,#40111,
#40112,#40113,#40114,#40115,#40116,#40117,#40118,#40119,#40120,#40121,#40122,
#40123,#40124,#40125,#40126,#40127,#40128,#40129,#40130,#40131,#40132,#40133,
#40134,#40135,#40136,#40137,#40138,#40139,#40140,#40141,#40142,#40143,#40144,
#40145,#40146,#40147,#40148,#40149,#40150,#40151,#40152,#40153,#40154,#40155,
#40156,#40157,#40158,#40159,#40160,#40161,#40162,#40163,#40164,#40165,#40166,
#40167,#40168,#40169,#40170,#40171,#40172,#40173,#40174,#40175,#40176,#40177,
#40178,#40179,#40180,#40181,#40182,#40183,#40184,#40185,#40186,#40187,#40188,
#40189,#40190,#40191,#40192,#40193,#40194,#40195,#40196,#40197,#40198),
 .UNSPECIFIED.,.F.,.F.,(4,3,3,3,3,3,3,3,3,3,3,3,3,3,3,3,3,3,3,3,3,3,3,3,
3,3,3,3,3,3,3,3,3,3,4),(2.32323281300321E-5,0.0263338187849373,0.0528930048012295,
0.0775527614301843,0.119264862169425,0.151532031317049,0.178160167750092,
0.208545348730825,0.230146401786176,0.259521454361925,0.289979534064853,
0.307566150720886,0.338352589115474,0.370211365474543,0.381353773173637,
0.401064064510986,0.443757841669673,0.487322691796688,0.518553003926838,
0.542684984551173,0.578781121546917,0.611023690584681,0.626943865232523,
0.66435333949954,0.690413260713517,0.720854398171208,0.762829179862876,
0.796341399568512,0.840816408102127,0.873251888090859,0.904910640783385,
0.922121378589668,0.946130264709519,0.973008581785241,0.999886898860964),
 .UNSPECIFIED.);
#2374=B_SPLINE_CURVE_WITH_KNOTS('',3,(#40276,#40277,#40278,#40279,#40280,
#40281,#40282,#40283,#40284,#40285,#40286,#40287,#40288,#40289,#40290,#40291,
#40292,#40293,#40294,#40295,#40296,#40297,#40298,#40299,#40300,#40301,#40302,
#40303,#40304,#40305,#40306,#40307,#40308,#40309,#40310,#40311,#40312,#40313,
#40314,#40315,#40316,#40317,#40318,#40319,#40320,#40321,#40322,#40323,#40324,
#40325),.UNSPECIFIED.,.F.,.F.,(4,2,2,2,2,2,2,2,2,2,2,2,2,2,2,2,2,2,2,2,
2,2,2,2,4),(-0.971724970861776,-0.96224259779374,-0.952818323332198,-0.933893341089848,
-0.921462843293419,-0.89460619776171,-0.871724738068697,-0.85365992165184,
-0.81998862327022,-0.787153942616391,-0.779148549923685,-0.744697301863035,
-0.701771598759441,-0.687301558135749,-0.628830738460491,-0.599891230916682,
-0.570631735013558,-0.517566468648308,-0.458469083445789,-0.384209139007974,
-0.330398146101072,-0.213378846484283,-0.160737820237478,-0.0805171288285796,
-0.00012725556241822),.UNSPECIFIED.);
#2375=B_SPLINE_CURVE_WITH_KNOTS('',3,(#40329,#40330,#40331,#40332,#40333,
#40334,#40335,#40336),.UNSPECIFIED.,.F.,.F.,(4,2,2,4),(-0.209975020768575,
-0.157314244107572,-0.104768532932063,-0.000184589268263047),
 .UNSPECIFIED.);
#2376=B_SPLINE_CURVE_WITH_KNOTS('',3,(#40338,#40339,#40340,#40341,#40342,
#40343,#40344,#40345,#40346,#40347,#40348,#40349,#40350,#40351,#40352,#40353,
#40354,#40355,#40356,#40357,#40358,#40359,#40360,#40361),.UNSPECIFIED.,
 .F.,.F.,(4,2,2,2,2,2,2,2,2,2,2,4),(-1.20838688604733,-1.02839026997692,
-0.883923566776128,-0.809599158177502,-0.752742598652501,-0.622907067493251,
-0.544861408462318,-0.469857238864126,-0.380271098777597,-0.22441099221183,
-0.11473204145142,-6.43510293987729E-5),.UNSPECIFIED.);
#2377=B_SPLINE_CURVE_WITH_KNOTS('',3,(#40362,#40363,#40364,#40365,#40366,
#40367),.UNSPECIFIED.,.F.,.F.,(4,2,4),(-0.210251406797625,-0.104231041931576,
-2.34000127149505E-5),.UNSPECIFIED.);
#2378=B_SPLINE_CURVE_WITH_KNOTS('',3,(#40445,#40446,#40447,#40448,#40449,
#40450,#40451,#40452,#40453,#40454,#40455,#40456,#40457,#40458,#40459,#40460,
#40461,#40462,#40463,#40464,#40465,#40466,#40467,#40468,#40469,#40470,#40471,
#40472),.UNSPECIFIED.,.F.,.F.,(4,2,2,2,2,2,2,2,2,2,2,2,2,4),(0.000185064574131046,
0.0602712190498164,0.0995806517125012,0.155361344960956,0.243764972296806,
0.328938012928217,0.44400330868783,0.523479738663989,0.636194951156639,
0.696271818136377,0.798069126561032,0.914768324732951,0.968509100593359,
1.0452089632934),.UNSPECIFIED.);
#2379=B_SPLINE_CURVE_WITH_KNOTS('',3,(#40474,#40475,#40476,#40477,#40478,
#40479,#40480,#40481,#40482,#40483,#40484,#40485,#40486,#40487,#40488,#40489,
#40490,#40491,#40492,#40493,#40494,#40495,#40496,#40497,#40498,#40499,#40500,
#40501,#40502,#40503,#40504,#40505,#40506,#40507,#40508,#40509,#40510,#40511),
 .UNSPECIFIED.,.F.,.F.,(4,2,2,2,2,2,2,2,2,2,2,2,2,2,2,2,2,2,4),(9.99999997513407E-7,
0.0303667674586334,0.141492987035643,0.19944954580558,0.303623465621176,
0.412366612058417,0.464341609383842,0.616716522689497,0.679112215291004,
0.7325047929673,0.817077506721457,0.960667112020537,1.01645812460288,1.07615291575373,
1.20142634084652,1.23728397080356,1.29083685108454,1.35242730915233,1.46720649961044),
 .UNSPECIFIED.);
#2380=B_SPLINE_CURVE_WITH_KNOTS('',3,(#40514,#40515,#40516,#40517,#40518,
#40519,#40520,#40521,#40522,#40523,#40524,#40525,#40526,#40527,#40528,#40529,
#40530,#40531,#40532,#40533,#40534,#40535,#40536,#40537,#40538,#40539,#40540,
#40541,#40542,#40543,#40544,#40545,#40546,#40547,#40548,#40549,#40550,#40551,
#40552,#40553,#40554,#40555,#40556,#40557,#40558,#40559,#40560,#40561,#40562,
#40563,#40564,#40565,#40566,#40567,#40568,#40569,#40570,#40571,#40572,#40573,
#40574,#40575,#40576,#40577,#40578,#40579,#40580,#40581,#40582,#40583),
 .UNSPECIFIED.,.F.,.F.,(4,2,2,2,2,2,2,2,2,2,2,2,2,2,2,2,2,2,2,2,2,2,2,2,
2,2,2,2,2,2,2,2,2,2,4),(0.000157510224987102,0.0993438493857167,0.188679914346204,
0.251784653428834,0.325862121808707,0.396147813640377,0.465938047156506,
0.526407126825593,0.693172362540282,0.884298387388191,1.03992644234621,
1.1210001397561,1.26371285847868,1.34200253030502,1.42337789123169,1.50196743316852,
1.66711606180234,1.73823621187051,1.81027162284586,1.89143678561552,1.97120519965067,
2.08594346219961,2.16818425450836,2.37346759844623,2.53001217453886,2.68063586602847,
2.89513436904536,3.28430649623881,3.51460467191784,4.14852019298852,4.82236598808902,
5.27439622507704,5.66498526255755,6.25935444338318,6.85318641309348),
 .UNSPECIFIED.);
#2381=B_SPLINE_CURVE_WITH_KNOTS('',3,(#40802,#40803,#40804,#40805,#40806,
#40807,#40808,#40809,#40810,#40811,#40812,#40813,#40814,#40815,#40816,#40817,
#40818,#40819,#40820,#40821,#40822,#40823,#40824,#40825,#40826,#40827,#40828,
#40829,#40830,#40831,#40832,#40833,#40834,#40835,#40836,#40837,#40838,#40839,
#40840,#40841,#40842,#40843,#40844,#40845,#40846,#40847,#40848,#40849,#40850,
#40851,#40852,#40853,#40854,#40855,#40856,#40857,#40858,#40859,#40860,#40861,
#40862,#40863,#40864,#40865,#40866,#40867,#40868,#40869,#40870,#40871,#40872,
#40873,#40874,#40875,#40876,#40877,#40878,#40879,#40880,#40881,#40882,#40883,
#40884,#40885,#40886,#40887,#40888,#40889,#40890,#40891,#40892,#40893,#40894,
#40895,#40896,#40897,#40898,#40899,#40900,#40901,#40902,#40903,#40904,#40905,
#40906,#40907,#40908,#40909,#40910,#40911),.UNSPECIFIED.,.F.,.F.,(4,2,2,
2,2,2,2,2,2,2,2,2,2,2,2,2,2,2,2,2,2,2,2,2,2,2,2,2,2,2,2,2,2,2,2,2,2,2,2,
2,2,2,2,2,2,2,2,2,2,2,2,2,2,2,4),(0.000129114132454983,0.113390093891427,
0.218435321804352,0.324979934352919,0.428164360055101,0.552137859304061,
0.695073909918494,0.846441157571017,0.970455720707209,1.07899479568917,
1.18909049989486,1.29569784196736,1.42371115790198,1.57122215461547,1.72750515786628,
1.85545991638375,1.9674643599747,2.08103983160671,2.1910360991499,2.32304792646442,
2.47507422104983,2.63622907694774,2.76807562998618,2.88350978283409,3.00052157323439,
3.11386868051087,3.24982151808213,3.40628388628472,3.5627462544873,3.69869909205856,
3.81204619933504,3.92905798973533,4.04449214258324,4.17633869562168,4.3374935515196,
4.48951984610501,4.62153167341952,4.73152794096275,4.84510341259479,4.95710785618572,
5.08506261470318,5.24134561795402,5.38885661466752,5.51686993060214,5.62347727267468,
5.7335729768804,5.84211205186234,5.96612661499854,6.11749386265112,6.26042991326557,
6.38440341251452,6.48758783821671,6.59413245076532,6.69917767867827,6.81244210168984),
 .UNSPECIFIED.);
#2382=B_SPLINE_CURVE_WITH_KNOTS('',3,(#40914,#40915,#40916,#40917,#40918,
#40919,#40920,#40921,#40922,#40923,#40924,#40925,#40926,#40927,#40928,#40929,
#40930,#40931,#40932,#40933,#40934,#40935,#40936,#40937,#40938,#40939,#40940,
#40941,#40942,#40943,#40944,#40945,#40946,#40947,#40948,#40949,#40950,#40951,
#40952,#40953,#40954,#40955,#40956,#40957,#40958,#40959,#40960,#40961,#40962,
#40963,#40964,#40965,#40966,#40967,#40968,#40969,#40970,#40971,#40972,#40973,
#40974,#40975,#40976,#40977,#40978,#40979,#40980,#40981,#40982,#40983,#40984,
#40985,#40986,#40987,#40988,#40989,#40990,#40991,#40992,#40993,#40994,#40995,
#40996,#40997,#40998,#40999,#41000,#41001,#41002,#41003,#41004,#41005,#41006,
#41007,#41008,#41009,#41010,#41011,#41012,#41013,#41014,#41015,#41016,#41017,
#41018,#41019,#41020,#41021,#41022,#41023),.UNSPECIFIED.,.F.,.F.,(4,2,2,
2,2,2,2,2,2,2,2,2,2,2,2,2,2,2,2,2,2,2,2,2,2,2,2,2,2,2,2,2,2,2,2,2,2,2,2,
2,2,2,2,2,2,2,2,2,2,2,2,2,2,2,4),(-6.81071791048935,-6.69748642459302,-6.59246866459779,
-6.48595191203587,-6.38279446767657,-6.25885338583429,-6.1159547110793,
-5.96462704393112,-5.84064490893926,-5.73213421546912,-5.6220672998129,
-5.51548783412999,-5.38750799195991,-5.24003556739288,-5.08379343005054,
-4.95587212998563,-4.84389697405391,-4.73035120088386,-4.62038369588879,
-4.48840638789589,-4.33641984614675,-4.17530713008141,-4.04349505314758,
-3.92809108478184,-3.81110989139477,-3.69779242286604,-3.5618751351377,
-3.40545367974512,-3.24903222435254,-3.1131149366242,-2.99979746809548,
-2.8828162747084,-2.76741230634266,-2.63560022940884,-2.47448751334349,
-2.32250097159435,-2.19052366360146,-2.08055615860636,-1.96701038543629,
-1.85503522950457,-1.72711392943967,-1.5708717920973,-1.42339936753026,
-1.29541952536018,-1.18884005967721,-1.07877314402097,-0.970262450550858,
-0.846280315558988,-0.694952648410747,-0.552053973655728,-0.428112891813464,
-0.324955447454145,-0.218438694892192,-0.113420934896934,-0.000186114852025488),
 .UNSPECIFIED.);
#2383=B_SPLINE_CURVE_WITH_KNOTS('',3,(#41166,#41167,#41168,#41169,#41170,
#41171,#41172,#41173,#41174,#41175,#41176,#41177,#41178,#41179,#41180,#41181,
#41182,#41183,#41184,#41185,#41186,#41187,#41188,#41189,#41190,#41191,#41192,
#41193,#41194,#41195,#41196,#41197,#41198,#41199,#41200,#41201,#41202,#41203,
#41204,#41205,#41206,#41207,#41208,#41209,#41210,#41211,#41212,#41213,#41214,
#41215,#41216,#41217,#41218,#41219,#41220,#41221,#41222,#41223,#41224,#41225,
#41226,#41227,#41228,#41229,#41230,#41231,#41232,#41233,#41234,#41235,#41236,
#41237,#41238,#41239,#41240,#41241,#41242,#41243,#41244,#41245,#41246,#41247,
#41248,#41249,#41250,#41251,#41252,#41253,#41254,#41255,#41256,#41257,#41258,
#41259,#41260,#41261,#41262,#41263,#41264,#41265,#41266,#41267,#41268,#41269,
#41270,#41271,#41272,#41273,#41274,#41275,#41276,#41277,#41278,#41279,#41280,
#41281,#41282,#41283,#41284,#41285,#41286,#41287,#41288,#41289,#41290,#41291,
#41292,#41293,#41294,#41295,#41296,#41297,#41298,#41299,#41300,#41301,#41302,
#41303,#41304,#41305,#41306,#41307,#41308,#41309,#41310,#41311,#41312,#41313,
#41314,#41315,#41316,#41317,#41318,#41319,#41320,#41321,#41322,#41323,#41324,
#41325,#41326,#41327,#41328,#41329,#41330,#41331,#41332,#41333,#41334,#41335,
#41336,#41337,#41338,#41339,#41340,#41341,#41342,#41343,#41344,#41345),
 .UNSPECIFIED.,.F.,.F.,(4,2,2,2,2,2,2,2,2,2,2,2,2,2,2,2,2,2,2,2,2,2,2,2,
2,2,2,2,2,2,2,2,2,2,2,2,2,2,2,2,2,2,2,2,2,2,2,2,2,2,2,2,2,2,2,2,2,2,2,2,
2,2,2,2,2,2,2,2,2,2,2,2,2,2,2,2,2,2,2,2,2,2,2,2,2,2,2,2,2,4),(-5.86988290593197,
-5.83799332401546,-5.79410197724347,-5.73947964729276,-5.62977741049655,
-5.57972122260326,-5.51896918907118,-5.47512868052878,-5.35958775805997,
-5.30757022918753,-5.24754404245887,-5.20428195828346,-5.07801471872521,
-5.02875474902955,-4.97324450334103,-4.93014937845045,-4.80416147096541,
-4.7550384082473,-4.6997479903665,-4.65670129543007,-4.53092765933326,-4.48187016125483,
-4.42666019747262,-4.38368480638791,-4.25812788045421,-4.20914763124866,
-4.15399926806423,-4.11109081074757,-3.98580328536774,-3.93688802667624,
-3.88176062631921,-3.83890805816712,-3.71404101847719,-3.66515154462887,
-3.60985929431661,-3.56702816116338,-3.44313083149954,-3.39412861872233,
-3.33802934768471,-3.29508939030358,-3.17422274637664,-3.12456077020254,
-3.06526182537254,-3.02164022195564,-2.91325098632136,-2.85041530839486,
-2.80367996750775,-2.77122802009947,-2.72111557671893,-2.65878038666057,
-2.57421680926107,-2.52981130868839,-2.46204933981601,-2.4091686270665,
-2.30227765142875,-2.25801195797186,-2.19063687866087,-2.1378305403487,
-2.03047221215058,-1.98620174494898,-1.91885234144652,-1.86602471087127,
-1.75851326634842,-1.71421318079729,-1.64682064027922,-1.5939543206139,
-1.48634182173124,-1.4420067412229,-1.37457067592944,-1.32166044695823,
-1.21396913119586,-1.16959665799744,-1.10210581435966,-1.04916806628168,
-0.941379231431628,-0.896990858089643,-0.829343262584152,-0.776309816913608,
-0.668367641255489,-0.623859599579781,-0.556774519076718,-0.503805192902935,
-0.396308068918789,-0.351980356323967,-0.288013742466906,-0.237877191458961,
-0.129159111742741,-0.075595333196945,-0.031302567710868,-0.000193940477510359),
 .UNSPECIFIED.);
#2384=B_SPLINE_CURVE_WITH_KNOTS('',3,(#41487,#41488,#41489,#41490,#41491,
#41492,#41493,#41494,#41495,#41496,#41497,#41498,#41499,#41500,#41501,#41502,
#41503,#41504,#41505,#41506,#41507,#41508,#41509,#41510,#41511,#41512,#41513,
#41514,#41515,#41516,#41517,#41518,#41519,#41520,#41521,#41522,#41523,#41524,
#41525,#41526,#41527,#41528,#41529,#41530,#41531,#41532,#41533,#41534,#41535,
#41536,#41537,#41538,#41539,#41540,#41541,#41542,#41543,#41544,#41545,#41546,
#41547,#41548,#41549,#41550,#41551,#41552,#41553,#41554,#41555,#41556,#41557,
#41558,#41559,#41560,#41561,#41562,#41563,#41564,#41565,#41566,#41567,#41568,
#41569,#41570,#41571,#41572,#41573,#41574,#41575,#41576,#41577,#41578,#41579,
#41580,#41581,#41582,#41583,#41584,#41585,#41586,#41587,#41588,#41589,#41590,
#41591,#41592,#41593,#41594,#41595,#41596),.UNSPECIFIED.,.F.,.F.,(4,2,2,
2,2,2,2,2,2,2,2,2,2,2,2,2,2,2,2,2,2,2,2,2,2,2,2,2,2,2,2,2,2,2,2,2,2,2,2,
2,2,2,2,2,2,2,2,2,2,2,2,2,2,2,4),(-2.49584851444866,-2.42086616323668,-2.38614802829034,
-2.32969252891064,-2.28689945253446,-2.25395120746466,-2.19725039548955,
-2.14933335428152,-2.11468560901464,-2.06295576638154,-2.01712270260594,
-1.9832659184357,-1.92918001564781,-1.87970035978081,-1.84448761932614,
-1.7909980855805,-1.7462609286404,-1.71281222802058,-1.65811618243505,-1.60936580617528,
-1.5744861659387,-1.52084660708105,-1.47650724803446,-1.44321711480835,
-1.38159961844885,-1.33711580712783,-1.3035798530162,-1.2440853340121,-1.19077695863606,
-1.15694577714375,-1.11233093085342,-1.05023681326708,-1.01665656842421,
-0.970997769558366,-0.919431423775674,-0.883873349329957,-0.834016049267621,
-0.780973472692911,-0.747397098791494,-0.702008621311116,-0.649456920662372,
-0.613558084171164,-0.562951419053681,-0.510583395420632,-0.476597773425144,
-0.430104647279553,-0.379361620258774,-0.344100444554333,-0.295183740065816,
-0.240012225361866,-0.207030628428394,-0.163797587969506,-0.107959271216929,
-0.0724909230265645,-0.000105906793946138),.UNSPECIFIED.);
#2385=B_SPLINE_CURVE_WITH_KNOTS('',3,(#41739,#41740,#41741,#41742,#41743,
#41744,#41745,#41746,#41747,#41748,#41749,#41750,#41751,#41752,#41753,#41754,
#41755,#41756,#41757,#41758,#41759,#41760,#41761,#41762,#41763,#41764,#41765,
#41766,#41767,#41768,#41769,#41770,#41771,#41772,#41773,#41774,#41775,#41776,
#41777,#41778,#41779,#41780,#41781,#41782,#41783,#41784,#41785,#41786,#41787,
#41788,#41789,#41790,#41791,#41792,#41793,#41794,#41795,#41796,#41797,#41798,
#41799,#41800,#41801,#41802,#41803,#41804,#41805,#41806,#41807,#41808,#41809,
#41810,#41811,#41812,#41813,#41814,#41815,#41816,#41817,#41818,#41819,#41820,
#41821,#41822,#41823,#41824,#41825,#41826,#41827,#41828,#41829,#41830,#41831,
#41832,#41833,#41834,#41835,#41836,#41837,#41838,#41839,#41840,#41841,#41842,
#41843,#41844,#41845,#41846,#41847,#41848,#41849,#41850,#41851,#41852,#41853,
#41854,#41855,#41856,#41857,#41858,#41859,#41860,#41861,#41862,#41863,#41864,
#41865,#41866,#41867,#41868,#41869,#41870,#41871,#41872,#41873,#41874,#41875,
#41876,#41877,#41878,#41879,#41880,#41881,#41882,#41883,#41884,#41885,#41886,
#41887,#41888,#41889,#41890,#41891,#41892,#41893,#41894,#41895,#41896,#41897,
#41898,#41899,#41900,#41901,#41902,#41903,#41904,#41905,#41906,#41907,#41908,
#41909,#41910,#41911,#41912,#41913,#41914,#41915,#41916),.UNSPECIFIED.,
 .F.,.F.,(4,2,2,2,2,2,2,2,2,2,2,2,2,2,2,2,2,2,2,2,2,2,2,2,2,2,2,2,2,2,2,
2,2,2,2,2,2,2,2,2,2,2,2,2,2,2,2,2,2,2,2,2,2,2,2,2,2,2,2,2,2,2,2,2,2,2,2,
2,2,2,2,2,2,2,2,2,2,2,2,2,2,2,2,2,2,2,2,2,4),(-5.81343192393955,-5.78194346696491,
-5.73860415445271,-5.68466898290961,-5.57634666406845,-5.52692010070965,
-5.46693218365186,-5.4236431138491,-5.30955586922977,-5.25819254093151,
-5.19892102074225,-5.15620304728678,-5.03152512823552,-4.98288452023335,
-4.92807128029553,-4.88551799894344,-4.761118517748,-4.71261244572808,-4.65801319340276,
-4.61550715243308,-4.49132836731065,-4.44288477248686,-4.38835425229245,
-4.34591659340536,-4.22198359917362,-4.17360838650696,-4.11910134060711,
-4.07672268689262,-3.95316704188153,-3.90482827128912,-3.85021123988982,
-3.80786268380277,-3.68511673907705,-3.63670402666718,-3.58146188061304,
-3.53904198777237,-3.41871675745947,-3.36980866685654,-3.31206741735705,
-3.26914721180126,-3.15695262661369,-3.10594423568562,-3.0396793434762,
-2.99407929884949,-2.91424701825505,-2.82416604159401,-2.78115665183707,
-2.71647252526577,-2.66484413909547,-2.55173705551146,-2.51017912487732,
-2.45062249495088,-2.40013388510142,-2.28229703494248,-2.2409509298103,
-2.18252957317486,-2.13221307248469,-2.01310169337678,-1.97173795571909,
-1.91349444879949,-1.86313974466627,-1.74354587650129,-1.70211444989438,
-1.64382017524692,-1.59337849490485,-1.47348244784259,-1.43197037520573,
-1.3735829242948,-1.32304103988193,-1.20289737935556,-1.16130054378407,
-1.10279889411852,-1.05216928238786,-0.931771617962573,-0.890109738866415,
-0.8313818925562,-0.780597212044168,-0.659883751882108,-0.618052880715235,
-0.559845381164947,-0.509078297483705,-0.388637749176731,-0.346952093505117,
-0.286460606447632,-0.235650373603816,-0.127852847589458,-0.0744147835208843,
-0.0312981374707393,-0.000207727027547122),.UNSPECIFIED.);
#2386=B_SPLINE_CURVE_WITH_KNOTS('',3,(#41918,#41919,#41920,#41921,#41922,
#41923,#41924,#41925,#41926,#41927,#41928,#41929,#41930,#41931,#41932,#41933,
#41934,#41935,#41936,#41937,#41938,#41939,#41940,#41941,#41942,#41943,#41944,
#41945,#41946,#41947,#41948,#41949,#41950,#41951,#41952,#41953,#41954,#41955,
#41956,#41957,#41958,#41959,#41960,#41961,#41962,#41963,#41964,#41965,#41966,
#41967,#41968,#41969,#41970,#41971,#41972,#41973,#41974,#41975,#41976,#41977,
#41978,#41979,#41980,#41981,#41982,#41983,#41984,#41985,#41986,#41987,#41988,
#41989,#41990,#41991,#41992,#41993,#41994,#41995,#41996,#41997,#41998,#41999,
#42000,#42001,#42002,#42003,#42004,#42005,#42006,#42007,#42008,#42009,#42010,
#42011,#42012,#42013,#42014,#42015,#42016,#42017,#42018,#42019,#42020,#42021,
#42022,#42023,#42024,#42025,#42026,#42027),.UNSPECIFIED.,.F.,.F.,(4,2,2,
2,2,2,2,2,2,2,2,2,2,2,2,2,2,2,2,2,2,2,2,2,2,2,2,2,2,2,2,2,2,2,2,2,2,2,2,
2,2,2,2,2,2,2,2,2,2,2,2,2,2,2,4),(-2.49855388017476,-2.42342814551093,-2.3886436215689,
-2.33208016642435,-2.28920525988184,-2.25619401022828,-2.19938477359639,
-2.1513761038903,-2.11666210416291,-2.06483328147968,-2.01891261002298,
-1.98499109214821,-1.9308014529537,-1.88122737363105,-1.84594735686781,
-1.79236561780895,-1.74753713913737,-1.71402314799028,-1.65928344444008,
-1.61040262535647,-1.57544496390384,-1.5201610388553,-1.47660780572407,
-1.44344956811401,-1.38267536477288,-1.33782063810444,-1.30413387384197,
-1.24902398769069,-1.18682567208135,-1.1497092469778,-1.09474953306849,
-1.04753155189499,-1.01198397316158,-0.958727816046237,-0.917591786477728,
-0.880296196817386,-0.824910897146943,-0.780056305587087,-0.74596103696419,
-0.698528616918437,-0.649434328880524,-0.613516472675831,-0.562850084374765,
-0.51057844847517,-0.476590111852955,-0.430086093677056,-0.379361558957249,
-0.34410033730707,-0.295183489536067,-0.240012217833707,-0.207030618161296,
-0.163797566109981,-0.107959290444451,-0.0724909555157676,-0.000105906793936821),
 .UNSPECIFIED.);
#2387=B_SPLINE_CURVE_WITH_KNOTS('',3,(#42030,#42031,#42032,#42033,#42034,
#42035,#42036,#42037,#42038,#42039,#42040,#42041,#42042,#42043,#42044,#42045,
#42046,#42047,#42048,#42049,#42050,#42051,#42052,#42053,#42054,#42055,#42056,
#42057,#42058,#42059,#42060,#42061,#42062,#42063,#42064,#42065,#42066,#42067,
#42068,#42069,#42070,#42071,#42072,#42073,#42074,#42075,#42076,#42077,#42078,
#42079,#42080,#42081,#42082,#42083,#42084,#42085,#42086,#42087,#42088,#42089,
#42090,#42091,#42092,#42093,#42094,#42095,#42096,#42097,#42098,#42099,#42100,
#42101,#42102,#42103,#42104,#42105,#42106,#42107,#42108,#42109,#42110,#42111,
#42112,#42113,#42114,#42115,#42116,#42117,#42118,#42119,#42120,#42121,#42122,
#42123,#42124,#42125,#42126,#42127,#42128,#42129,#42130,#42131,#42132,#42133,
#42134,#42135,#42136,#42137,#42138,#42139),.UNSPECIFIED.,.F.,.F.,(4,2,2,
2,2,2,2,2,2,2,2,2,2,2,2,2,2,2,2,2,2,2,2,2,2,2,2,2,2,2,2,2,2,2,2,2,2,2,2,
2,2,2,2,2,2,2,2,2,2,2,2,2,2,2,4),(0.000186114852028536,0.113420934897052,
0.218438694892283,0.32495544745418,0.428112891813475,0.552053973655751,
0.694952648410875,0.846280315559075,0.970262450550931,1.07877314402106,
1.18884005967728,1.29541952536018,1.42339936753021,1.57087179209733,1.72711392943967,
1.85503522950455,1.96701038543624,2.08055615860629,2.19052366360141,2.32250097159434,
2.47448751334346,2.63560022940877,2.76741230634255,2.88281627470825,2.99979746809535,
3.11311493662413,3.2490322243525,3.40545367974495,3.56187513513741,3.69779242286587,
3.81110989139468,3.92809108478164,4.04349505314729,4.17530713008115,4.33641984614643,
4.48840638789552,4.62038369588843,4.73035120088352,4.84389697405351,4.9558721299852,
5.08379343005007,5.24003556739236,5.38750799195943,5.51548783412943,5.6220672998123,
5.7321342154685,5.84064490893866,5.96462704393049,6.11595471107872,6.25885338583376,
6.382794467676,6.48595191203529,6.59246866459722,6.69748642459247,6.81072123047711),
 .UNSPECIFIED.);
#2388=B_SPLINE_CURVE_WITH_KNOTS('',3,(#42281,#42282,#42283,#42284,#42285,
#42286,#42287,#42288,#42289,#42290,#42291,#42292,#42293,#42294,#42295,#42296,
#42297,#42298,#42299,#42300,#42301,#42302,#42303,#42304,#42305,#42306,#42307,
#42308,#42309,#42310,#42311,#42312,#42313,#42314,#42315,#42316,#42317,#42318,
#42319,#42320,#42321,#42322,#42323,#42324,#42325,#42326,#42327,#42328,#42329,
#42330,#42331,#42332,#42333,#42334,#42335,#42336,#42337,#42338,#42339,#42340,
#42341,#42342,#42343,#42344,#42345,#42346,#42347,#42348,#42349,#42350,#42351,
#42352,#42353,#42354,#42355,#42356,#42357,#42358,#42359,#42360,#42361,#42362,
#42363,#42364,#42365,#42366,#42367,#42368,#42369,#42370,#42371,#42372,#42373,
#42374,#42375,#42376,#42377,#42378,#42379,#42380,#42381,#42382,#42383,#42384,
#42385,#42386,#42387,#42388,#42389,#42390),.UNSPECIFIED.,.F.,.F.,(4,2,2,
2,2,2,2,2,2,2,2,2,2,2,2,2,2,2,2,2,2,2,2,2,2,2,2,2,2,2,2,2,2,2,2,2,2,2,2,
2,2,2,2,2,2,2,2,2,2,2,2,2,2,2,4),(-6.81072123047651,-6.69748642459177,-6.59246866459655,
-6.48595191203466,-6.38279446767538,-6.25885338583311,-6.115954711078,-5.96462704392981,
-5.84064490893797,-5.73213421546785,-5.62206729981164,-5.51548783412876,
-5.38750799195874,-5.24003556739163,-5.08379343004931,-4.95587212998444,
-4.84389697405276,-4.73035120088272,-4.6203836958876,-4.4884063878947,-4.33641984614558,
-4.17530713008029,-4.04349505314652,-3.92809108478083,-3.81110989139374,
-3.69779242286497,-3.56187513513662,-3.40545367974418,-3.24903222435173,
-3.11311493662328,-2.99979746809448,-2.88281627470753,-2.76741230634189,
-2.63560022940804,-2.47448751334277,-2.3225009715937,-2.1905236636008,-2.08055615860572,
-1.96701038543575,-1.85503522950406,-1.7271139294392,-1.57087179209693,
-1.42339936752987,-1.29541952535988,-1.18884005967702,-1.07877314402082,
-0.970262450550672,-0.84628031555885,-0.694952648410639,-0.552053973655609,
-0.428112891813383,-0.324955447454098,-0.218438694892172,-0.113420934896926,
-0.000186114852029566),.UNSPECIFIED.);
#2389=B_SPLINE_CURVE_WITH_KNOTS('',3,(#42533,#42534,#42535,#42536,#42537,
#42538,#42539,#42540,#42541,#42542,#42543,#42544,#42545,#42546,#42547,#42548,
#42549,#42550,#42551,#42552,#42553,#42554,#42555,#42556,#42557,#42558,#42559,
#42560,#42561,#42562,#42563,#42564,#42565,#42566,#42567,#42568,#42569,#42570,
#42571,#42572,#42573,#42574,#42575,#42576,#42577,#42578,#42579,#42580,#42581,
#42582,#42583,#42584,#42585,#42586,#42587,#42588,#42589,#42590,#42591,#42592,
#42593,#42594,#42595,#42596,#42597,#42598,#42599,#42600,#42601,#42602,#42603,
#42604,#42605,#42606,#42607,#42608,#42609,#42610,#42611,#42612,#42613,#42614,
#42615,#42616,#42617,#42618,#42619,#42620,#42621,#42622,#42623,#42624,#42625,
#42626,#42627,#42628,#42629,#42630,#42631,#42632,#42633,#42634,#42635,#42636,
#42637,#42638,#42639,#42640,#42641,#42642),.UNSPECIFIED.,.F.,.F.,(4,2,2,
2,2,2,2,2,2,2,2,2,2,2,2,2,2,2,2,2,2,2,2,2,2,2,2,2,2,2,2,2,2,2,2,2,2,2,2,
2,2,2,2,2,2,2,2,2,2,2,2,2,2,2,4),(-6.81072186467709,-6.69748703256578,-6.59246924824708,
-6.48595247101454,-6.38279500276269,-6.25885389221412,-6.11595518436193,
-5.9646274821643,-5.84064531845661,-5.73213459985401,-5.62206765870493,
-5.51548816833691,-5.38750829652513,-5.24003583780158,-5.0837936642716,
-4.95587233457851,-4.84389715271197,-4.73035135324333,-4.62038382277836,
-4.48840648421781,-4.33641990726669,-4.17530715388565,-4.04349504642242,
-3.9280910513277,-3.81110983084635,-3.69779233607186,-3.56187501686334,
-3.40545352524158,-3.24903203361983,-3.11311471441129,-2.99979721963673,
-2.88281599915529,-2.76741200406055,-2.63559989659742,-2.47448714321635,
-2.32250056626518,-2.19052322770464,-2.08055569723965,-1.96700989777096,
-1.85503471590438,-1.72711338621126,-1.57087121268124,-1.42339875395765,
-1.29541888214586,-1.18883939177779,-1.07877245062866,-0.970261732026059,
-0.84627956831836,-0.694951866120717,-0.552053158268449,-0.428112047719832,
-0.324954579467925,-0.218437802235375,-0.113420017916685,-0.000184814530532018),
 .UNSPECIFIED.);
#2390=B_SPLINE_CURVE_WITH_KNOTS('',3,(#42643,#42644,#42645,#42646,#42647,
#42648),.UNSPECIFIED.,.F.,.F.,(4,2,4),(-0.0463376484595311,-0.0232792425040161,
-2.35223677633965E-5),.UNSPECIFIED.);
#2391=B_SPLINE_CURVE_WITH_KNOTS('',3,(#42649,#42650,#42651,#42652,#42653,
#42654,#42655,#42656,#42657,#42658,#42659,#42660,#42661,#42662,#42663,#42664,
#42665,#42666,#42667,#42668,#42669,#42670,#42671,#42672,#42673,#42674,#42675,
#42676,#42677,#42678,#42679,#42680,#42681,#42682,#42683,#42684,#42685,#42686,
#42687,#42688,#42689,#42690,#42691,#42692,#42693,#42694,#42695,#42696,#42697,
#42698,#42699,#42700,#42701,#42702,#42703,#42704,#42705,#42706,#42707,#42708,
#42709,#42710,#42711,#42712,#42713,#42714,#42715,#42716,#42717,#42718,#42719,
#42720,#42721,#42722,#42723,#42724,#42725,#42726,#42727,#42728,#42729,#42730,
#42731,#42732,#42733,#42734,#42735,#42736,#42737,#42738,#42739,#42740,#42741,
#42742,#42743,#42744,#42745,#42746,#42747,#42748,#42749,#42750,#42751,#42752,
#42753,#42754,#42755,#42756,#42757,#42758,#42759,#42760,#42761,#42762,#42763,
#42764,#42765,#42766,#42767,#42768,#42769,#42770,#42771,#42772,#42773,#42774,
#42775,#42776,#42777,#42778,#42779,#42780,#42781,#42782,#42783,#42784,#42785,
#42786,#42787,#42788,#42789,#42790,#42791,#42792,#42793,#42794,#42795,#42796,
#42797,#42798,#42799,#42800,#42801,#42802,#42803,#42804,#42805,#42806,#42807,
#42808,#42809,#42810,#42811,#42812,#42813,#42814,#42815,#42816,#42817,#42818,
#42819,#42820,#42821,#42822,#42823,#42824,#42825,#42826),.UNSPECIFIED.,
 .F.,.F.,(4,2,2,2,2,2,2,2,2,2,2,2,2,2,2,2,2,2,2,2,2,2,2,2,2,2,2,2,2,2,2,
2,2,2,2,2,2,2,2,2,2,2,2,2,2,2,2,2,2,2,2,2,2,2,2,2,2,2,2,2,2,2,2,2,2,2,2,
2,2,2,2,2,2,2,2,2,2,2,2,2,2,2,2,2,2,2,2,2,4),(-5.81158509839654,-5.78007408364135,
-5.73690027962185,-5.68285782741762,-5.57464154317438,-5.5252442398387,
-5.46529189609478,-5.42202845680168,-5.30800824915912,-5.25667545783596,
-5.19743952887423,-5.15474692022444,-5.03014130861183,-4.98152983756949,
-4.92675073446084,-4.88422295126807,-4.75989199425356,-4.7114158759881,
-4.65685488190427,-4.61437511286984,-4.49025212361444,-4.44184157097751,
-4.38736406263288,-4.3449554315813,-4.22103416306194,-4.17270285247783,
-4.11830038804471,-4.07596050565412,-3.95226274312296,-3.90400608326453,
-3.84967403192356,-3.80739874540725,-3.68396757439753,-3.6357733449824,
-3.58145273720433,-3.53923214088518,-3.41623040582683,-3.36805825972575,
-3.31355917139572,-3.27135621400733,-3.14936222041352,-3.10106551523939,
-3.03930670133814,-2.9934508296899,-2.91534231128656,-2.8237282641102,-2.78088320114212,
-2.71668216090014,-2.66517461717443,-2.55168867130034,-2.51014507494687,
-2.45064697615994,-2.40017133277286,-2.28228599391634,-2.2409429664815,
-2.1825352375726,-2.13222166770922,-2.0130990851343,-1.97173606397672,-1.91349579123466,
-1.8631417778932,-1.74354525541854,-1.70211399882852,-1.64382049510977,
-1.59337897915575,-1.47348229965046,-1.43197026753863,-1.37358300059391,
-1.32304115540395,-1.20289734397171,-1.1613005180707,-1.10279891231429,
-1.052169309939,-0.931771609500933,-0.890109732715275,-0.831381896884102,
-0.78059721860677,-0.659883749855692,-0.618052879239476,-0.559845382197793,
-0.50907829905577,-0.388637748692026,-0.346952093154151,-0.286460606693424,
-0.235650373973567,-0.127852847812578,-0.074414783243345,-0.031298137464462,
-0.000207727027570367),.UNSPECIFIED.);
#2392=B_SPLINE_CURVE_WITH_KNOTS('',3,(#42968,#42969,#42970,#42971,#42972,
#42973),.UNSPECIFIED.,.F.,.F.,(4,2,4),(-0.0464673921126319,-0.0232138500385779,
-5.92302360825546E-5),.UNSPECIFIED.);
#2393=B_SPLINE_CURVE_WITH_KNOTS('',3,(#42974,#42975,#42976,#42977,#42978,
#42979,#42980,#42981,#42982,#42983,#42984,#42985,#42986,#42987,#42988,#42989,
#42990,#42991,#42992,#42993,#42994,#42995,#42996,#42997,#42998,#42999,#43000,
#43001,#43002,#43003,#43004,#43005,#43006,#43007,#43008,#43009,#43010,#43011,
#43012,#43013,#43014,#43015,#43016,#43017,#43018,#43019,#43020,#43021,#43022,
#43023,#43024,#43025,#43026,#43027,#43028,#43029,#43030,#43031,#43032,#43033,
#43034,#43035,#43036,#43037,#43038,#43039,#43040,#43041,#43042,#43043,#43044,
#43045,#43046,#43047,#43048,#43049,#43050,#43051,#43052,#43053,#43054,#43055,
#43056,#43057,#43058,#43059,#43060,#43061,#43062,#43063,#43064,#43065,#43066,
#43067,#43068,#43069,#43070,#43071,#43072,#43073,#43074,#43075,#43076,#43077,
#43078,#43079,#43080,#43081,#43082,#43083),.UNSPECIFIED.,.F.,.F.,(4,2,2,
2,2,2,2,2,2,2,2,2,2,2,2,2,2,2,2,2,2,2,2,2,2,2,2,2,2,2,2,2,2,2,2,2,2,2,2,
2,2,2,2,2,2,2,2,2,2,2,2,2,2,2,4),(0.000186114852028654,0.113420934896994,
0.218438694892263,0.324955447454189,0.428112891813479,0.552053973655729,
0.69495264841079,0.846280315559027,0.970262450550892,1.07877314402105,1.18884005967725,
1.29541952536013,1.42339936753017,1.57087179209725,1.72711392943958,1.85503522950449,
1.96701038543619,2.08055615860619,2.1905236636013,2.32250097159425,2.47448751334338,
2.63560022940869,2.76741230634258,2.8828162747083,2.99979746809533,3.11311493662407,
3.24903222435243,3.40545367974502,3.56187513513759,3.69779242286599,3.81110989139479,
3.92809108478191,4.04349505314765,4.17530713008144,4.33641984614678,4.48840638789596,
4.6203836958889,4.73035120088403,4.84389697405409,4.95587212998582,5.08379343005076,
5.24003556739313,5.38750799196026,5.51548783413032,5.62206729981324,5.73213421546949,
5.84064490893965,5.96462704393152,6.11595471107978,6.25885338583492,6.38279446767723,
6.48595191203657,6.59246866459851,6.69748642459376,6.81072158854588),
 .UNSPECIFIED.);
#2394=B_SPLINE_CURVE_WITH_KNOTS('',3,(#43225,#43226,#43227,#43228,#43229,
#43230),.UNSPECIFIED.,.F.,.F.,(4,2,4),(-0.0289951303379412,-0.014591319104119,
-0.000183151741413589),.UNSPECIFIED.);
#2395=B_SPLINE_CURVE_WITH_KNOTS('',3,(#43381,#43382,#43383,#43384,#43385,
#43386,#43387,#43388,#43389,#43390,#43391,#43392,#43393,#43394,#43395,#43396,
#43397,#43398,#43399,#43400,#43401,#43402,#43403),.UNSPECIFIED.,.F.,.F.,
(4,2,2,2,2,3,2,2,2,2,4),(-0.599381390807594,-0.519369386765995,-0.439357382724396,
-0.329518037043297,-0.219678691362198,0.,0.219678691362198,0.329518037043297,
0.439357382724396,0.519369386765995,0.599381390807594),.UNSPECIFIED.);
#2396=B_SPLINE_CURVE_WITH_KNOTS('',3,(#43404,#43405,#43406,#43407,#43408,
#43409,#43410,#43411,#43412,#43413,#43414,#43415,#43416,#43417,#43418,#43419,
#43420,#43421,#43422,#43423,#43424,#43425),.UNSPECIFIED.,.F.,.F.,(4,2,2,
2,2,2,2,2,2,2,4),(0.599381390807594,0.679393394849193,0.759405398890792,
0.869244744571891,0.97908409025299,1.19876278161519,1.41844147297739,1.52828081865849,
1.63812016433958,1.71813216838118,1.79814417242278),.UNSPECIFIED.);
#2397=B_SPLINE_CURVE_WITH_KNOTS('',3,(#43436,#43437,#43438,#43439,#43440,
#43441,#43442,#43443,#43444,#43445,#43446,#43447,#43448,#43449,#43450,#43451,
#43452,#43453,#43454,#43455,#43456,#43457,#43458,#43459,#43460,#43461,#43462,
#43463,#43464,#43465,#43466,#43467,#43468,#43469,#43470,#43471,#43472,#43473,
#43474,#43475,#43476,#43477,#43478,#43479,#43480,#43481,#43482,#43483,#43484,
#43485,#43486,#43487,#43488,#43489,#43490,#43491,#43492,#43493,#43494,#43495,
#43496,#43497,#43498,#43499,#43500,#43501,#43502,#43503,#43504,#43505,#43506,
#43507,#43508,#43509,#43510,#43511,#43512,#43513,#43514,#43515,#43516,#43517,
#43518,#43519,#43520,#43521,#43522,#43523,#43524,#43525,#43526,#43527,#43528,
#43529,#43530,#43531,#43532,#43533,#43534,#43535,#43536,#43537,#43538,#43539,
#43540,#43541,#43542,#43543,#43544,#43545,#43546,#43547,#43548,#43549,#43550,
#43551,#43552,#43553,#43554,#43555,#43556,#43557,#43558,#43559,#43560,#43561,
#43562,#43563,#43564,#43565,#43566,#43567,#43568,#43569,#43570,#43571,#43572,
#43573,#43574,#43575,#43576,#43577,#43578,#43579,#43580,#43581,#43582,#43583,
#43584,#43585,#43586,#43587,#43588,#43589,#43590,#43591,#43592,#43593,#43594,
#43595,#43596,#43597,#43598),.UNSPECIFIED.,.F.,.F.,(4,3,3,3,3,3,3,3,3,3,
3,3,3,3,3,3,3,3,3,3,3,3,3,3,3,3,3,3,3,3,3,3,3,3,3,3,3,3,3,3,3,3,3,3,3,3,
3,3,3,3,3,3,3,3,4),(0.,0.0271485983010553,0.05263157894737,0.0811718380673146,
0.1052631578947,0.135206120413793,0.1578947368421,0.189291818846306,0.2105263157895,
0.243358105064165,0.2631578947368,0.294194908421614,0.297337794500015,0.3157894736842,
0.340129611785252,0.3513224823538,0.3684210526316,0.389398663890277,0.405409303715733,
0.4210526315789,0.443739980215653,0.459561087966757,0.4736842105263,0.493656585303444,
0.512541581707809,0.513628960080588,0.5263157894737,0.55624241470489,0.567623145833444,
0.5789473684211,0.606798151158574,0.621680971678114,0.6315789473684,0.661305928252685,
0.675748561652349,0.6842105263158,0.720695129581258,0.72974635703808,0.7368421052632,
0.765451968761437,0.783751433607901,0.7894736842105,0.813669118094079,0.837825750838692,
0.8421052631579,0.867000882414173,0.891896501670446,0.8947368421053,0.916009887512648,
0.936015949101071,0.945950981672964,0.9473684210526,0.9668595667857,0.985375475970587,
0.999999996167332),.UNSPECIFIED.);
#2398=B_SPLINE_CURVE_WITH_KNOTS('',3,(#43602,#43603,#43604,#43605,#43606,
#43607,#43608,#43609,#43610,#43611),.UNSPECIFIED.,.F.,.F.,(4,3,3,4),(0.,
0.3333333333333,0.6666666666667,1.),.UNSPECIFIED.);
#2399=B_SPLINE_CURVE_WITH_KNOTS('',3,(#43613,#43614,#43615,#43616,#43617,
#43618,#43619,#43620,#43621),.UNSPECIFIED.,.F.,.F.,(4,1,1,1,1,1,4),(2.5958560708529E-7,
0.1666666666667,0.3333333333333,0.5,0.6666666666667,0.8333333333333,0.999999934146645),
 .UNSPECIFIED.);
#2400=B_SPLINE_CURVE_WITH_KNOTS('',3,(#43623,#43624,#43625,#43626,#43627,
#43628,#43629,#43630),.UNSPECIFIED.,.F.,.F.,(4,1,1,1,1,4),(5.10274934168318E-8,
0.2,0.4,0.6,0.8,1.),.UNSPECIFIED.);
#2401=B_SPLINE_CURVE_WITH_KNOTS('',3,(#43670,#43671,#43672,#43673,#43674,
#43675,#43676,#43677,#43678,#43679,#43680,#43681,#43682,#43683,#43684,#43685,
#43686,#43687,#43688,#43689,#43690,#43691,#43692,#43693,#43694,#43695,#43696,
#43697,#43698,#43699,#43700,#43701,#43702,#43703,#43704,#43705,#43706,#43707,
#43708,#43709,#43710,#43711,#43712,#43713,#43714,#43715,#43716,#43717,#43718,
#43719,#43720,#43721,#43722,#43723,#43724,#43725,#43726,#43727,#43728,#43729,
#43730,#43731,#43732,#43733,#43734,#43735,#43736,#43737,#43738,#43739,#43740,
#43741,#43742,#43743,#43744,#43745,#43746,#43747,#43748,#43749,#43750,#43751,
#43752,#43753,#43754,#43755,#43756,#43757,#43758,#43759,#43760),
 .UNSPECIFIED.,.F.,.F.,(4,3,3,3,3,3,3,3,3,3,3,3,3,3,3,3,3,3,3,3,3,3,3,3,
3,3,3,3,3,3,4),(2.55444286463925E-6,3.59894613493354E-5,0.0376304039226987,
0.0778196513591974,0.09090909090909,0.100015854684267,0.149597044039808,
0.1818181818182,0.20002307736844,0.252770096807691,0.2727272727273,0.300045132044768,
0.356511609189304,0.3636363636364,0.399993667063145,0.4545454545455,0.500004431078461,
0.5454545454545,0.600029859440393,0.6363636363636,0.696679386572962,0.699994555111378,
0.7272727272727,0.779840762831178,0.800031874864246,0.8181818181818,0.873862262978403,
0.899972577418814,0.9090909090909,0.961329494918914,1.),.UNSPECIFIED.);
#2402=B_SPLINE_CURVE_WITH_KNOTS('',3,(#43825,#43826,#43827,#43828,#43829,
#43830,#43831,#43832,#43833,#43834,#43835,#43836,#43837,#43838),
 .UNSPECIFIED.,.F.,.F.,(4,1,1,1,1,1,1,1,1,1,1,4),(1.1830067436204E-6,0.09090909090909,
0.1818181818182,0.2727272727273,0.3636363636364,0.4545454545455,0.5454545454545,
0.6363636363636,0.7272727272727,0.8181818181818,0.9090909090909,1.),
 .UNSPECIFIED.);
#2403=B_SPLINE_CURVE_WITH_KNOTS('',3,(#43906,#43907,#43908,#43909,#43910,
#43911,#43912,#43913,#43914,#43915,#43916,#43917,#43918,#43919,#43920,#43921,
#43922,#43923,#43924,#43925,#43926,#43927,#43928,#43929,#43930,#43931,#43932,
#43933,#43934,#43935,#43936,#43937,#43938,#43939,#43940,#43941,#43942,#43943,
#43944,#43945,#43946,#43947,#43948,#43949,#43950,#43951,#43952,#43953,#43954,
#43955,#43956,#43957,#43958,#43959,#43960,#43961,#43962,#43963,#43964,#43965,
#43966,#43967,#43968,#43969,#43970,#43971,#43972,#43973,#43974,#43975,#43976,
#43977,#43978,#43979,#43980,#43981,#43982,#43983,#43984,#43985,#43986,#43987,
#43988,#43989,#43990,#43991,#43992,#43993),.UNSPECIFIED.,.F.,.F.,(4,3,3,
3,3,3,3,3,3,3,3,3,3,3,3,3,3,3,3,3,3,3,3,3,3,3,3,3,3,4),(0.,0.0521094210463995,
0.09090909090909,0.100029793188817,0.155493160568291,0.1818181818182,0.199972986695707,
0.25252274815469,0.2727272727273,0.300015130565433,0.3636363636364,0.399976334120297,
0.4545454545455,0.50000649866054,0.5454545454545,0.600029082805183,0.6363636363636,
0.693010325114171,0.699967328272808,0.7272727272727,0.779887482806084,0.799997660318204,
0.8181818181818,0.86860586501179,0.900008800503424,0.9090909090909,0.949304252134719,
0.986777025421057,0.999997850420203,0.999998520519915),.UNSPECIFIED.);
#2404=B_SPLINE_CURVE_WITH_KNOTS('',3,(#43994,#43995,#43996,#43997,#43998,
#43999,#44000,#44001,#44002,#44003,#44004,#44005,#44006,#44007,#44008,#44009,
#44010,#44011,#44012,#44013,#44014,#44015,#44016,#44017,#44018,#44019,#44020,
#44021,#44022,#44023,#44024,#44025,#44026,#44027,#44028,#44029,#44030,#44031,
#44032,#44033,#44034,#44035,#44036,#44037,#44038,#44039,#44040,#44041,#44042,
#44043,#44044,#44045,#44046,#44047,#44048),.UNSPECIFIED.,.F.,.F.,(4,3,3,
3,3,3,3,3,3,3,3,3,3,3,3,3,3,3,4),(0.,0.09090909090909,0.1818181818182,0.2727272727273,
0.3636363636364,0.448887126274961,0.4545454545455,0.538390793737757,0.5454545454545,
0.620795104544488,0.6363636363636,0.70236319270021,0.7272727272727,0.792436576680819,
0.8181818181818,0.883253394758865,0.9090909090909,0.979516285384546,0.999999999997833),
 .UNSPECIFIED.);
#2405=B_SPLINE_CURVE_WITH_KNOTS('',3,(#44110,#44111,#44112,#44113,#44114,
#44115,#44116,#44117,#44118,#44119,#44120,#44121,#44122,#44123,#44124,#44125,
#44126,#44127,#44128,#44129,#44130,#44131,#44132,#44133,#44134),
 .UNSPECIFIED.,.F.,.F.,(4,3,3,3,3,3,3,3,4),(0.,0.125,0.25,0.375,0.5,0.625,
0.75,0.875,1.),.UNSPECIFIED.);
#2406=B_SPLINE_CURVE_WITH_KNOTS('',3,(#44137,#44138,#44139,#44140,#44141,
#44142,#44143,#44144,#44145,#44146,#44147,#44148,#44149,#44150,#44151,#44152,
#44153,#44154,#44155,#44156,#44157,#44158,#44159,#44160,#44161,#44162,#44163,
#44164),.UNSPECIFIED.,.F.,.F.,(4,3,3,3,3,3,3,3,3,4),(0.,0.1111111111111,
0.2222222222222,0.3333333333333,0.4444444444444,0.5555555555556,0.6666666666667,
0.7777777777778,0.8888888888889,0.999999995464213),.UNSPECIFIED.);
#2407=B_SPLINE_CURVE_WITH_KNOTS('',3,(#44250,#44251,#44252,#44253,#44254,
#44255,#44256,#44257,#44258,#44259,#44260,#44261,#44262,#44263,#44264,#44265,
#44266,#44267,#44268,#44269,#44270,#44271,#44272,#44273,#44274,#44275,#44276,
#44277,#44278,#44279,#44280,#44281,#44282,#44283,#44284,#44285,#44286,#44287,
#44288,#44289,#44290,#44291,#44292,#44293,#44294,#44295,#44296,#44297,#44298,
#44299,#44300,#44301,#44302,#44303,#44304,#44305,#44306,#44307,#44308,#44309,
#44310,#44311,#44312,#44313,#44314,#44315,#44316,#44317,#44318,#44319,#44320,
#44321,#44322,#44323,#44324,#44325,#44326,#44327,#44328,#44329,#44330,#44331,
#44332,#44333,#44334,#44335,#44336,#44337,#44338,#44339,#44340,#44341,#44342,
#44343,#44344,#44345,#44346,#44347,#44348,#44349,#44350,#44351,#44352,#44353,
#44354,#44355,#44356,#44357,#44358,#44359,#44360,#44361,#44362,#44363,#44364,
#44365,#44366,#44367),.UNSPECIFIED.,.F.,.F.,(4,3,3,3,3,3,3,3,3,3,3,3,3,
3,3,3,3,3,3,3,3,3,3,3,3,3,3,3,3,3,3,3,3,3,3,3,3,3,3,4),(2.86331152536071E-8,
0.0645615368166531,0.07142857142857,0.105823175263765,0.126783995341246,
0.1428571428571,0.196188267240046,0.2142857142857,0.245830118964743,0.276006551966036,
0.2857142857143,0.286907673257762,0.31962058114641,0.353834550293338,0.3571428571429,
0.410078570789993,0.420069072508489,0.4285714285714,0.485540140741139,0.5,
0.543491980185507,0.5714285714286,0.615772050421601,0.6428571428571,0.663598566580769,
0.696842541691307,0.7142857142857,0.746138463334994,0.777991212384288,0.7857142857143,
0.819589820812744,0.852305725672241,0.8571428571429,0.876162598148888,0.904048950216825,
0.9285714285714,0.952879545673236,0.963346746013781,0.986631905020373,1.),
 .UNSPECIFIED.);
#2408=B_SPLINE_CURVE_WITH_KNOTS('',3,(#44372,#44373,#44374,#44375,#44376,
#44377,#44378,#44379),.UNSPECIFIED.,.F.,.F.,(4,2,2,4),(1.00274854907622E-6,
0.034413002030414,0.062461027026842,0.0705842206571842),.UNSPECIFIED.);
#2409=B_SPLINE_CURVE_WITH_KNOTS('',3,(#44473,#44474,#44475,#44476,#44477,
#44478,#44479,#44480,#44481,#44482,#44483,#44484,#44485,#44486,#44487,#44488,
#44489,#44490,#44491,#44492,#44493,#44494,#44495),.UNSPECIFIED.,.F.,.F.,
(4,1,1,1,1,1,1,1,1,1,1,1,1,1,1,1,1,1,1,1,4),(0.,0.05,0.1,0.15,0.2,0.25,
0.3,0.35,0.4,0.45,0.5,0.55,0.6,0.65,0.7,0.75,0.8,0.85,0.9,0.95,1.),
 .UNSPECIFIED.);
#2410=B_SPLINE_CURVE_WITH_KNOTS('',3,(#44534,#44535,#44536,#44537,#44538,
#44539),.UNSPECIFIED.,.F.,.F.,(4,1,1,4),(0.,0.3333333333333,0.6666666666667,
1.),.UNSPECIFIED.);
#2411=B_SPLINE_CURVE_WITH_KNOTS('',3,(#44549,#44550,#44551,#44552,#44553,
#44554,#44555,#44556,#44557,#44558),.UNSPECIFIED.,.F.,.F.,(4,3,3,4),(0.,
0.3333333333333,0.6666666666667,1.),.UNSPECIFIED.);
#2412=B_SPLINE_CURVE_WITH_KNOTS('',3,(#44560,#44561,#44562,#44563,#44564,
#44565,#44566,#44567,#44568,#44569,#44570,#44571,#44572,#44573,#44574,#44575,
#44576,#44577,#44578,#44579,#44580,#44581,#44582,#44583,#44584,#44585,#44586,
#44587,#44588,#44589,#44590,#44591,#44592,#44593),.UNSPECIFIED.,.F.,.F.,
(4,3,3,3,3,3,3,3,3,3,3,4),(0.,0.128706181276151,0.2,0.32521503540555,0.4,
0.506081427734201,0.6,0.693453062106393,0.786170793391711,0.8,0.904195677401466,
0.99999863924574),.UNSPECIFIED.);
#2413=B_SPLINE_CURVE_WITH_KNOTS('',3,(#44595,#44596,#44597,#44598,#44599,
#44600,#44601,#44602,#44603,#44604,#44605,#44606,#44607,#44608,#44609,#44610,
#44611,#44612,#44613,#44614,#44615,#44616,#44617,#44618,#44619,#44620,#44621,
#44622,#44623,#44624,#44625,#44626,#44627,#44628,#44629,#44630,#44631,#44632,
#44633,#44634,#44635,#44636,#44637,#44638,#44639,#44640,#44641,#44642,#44643,
#44644,#44645,#44646,#44647,#44648,#44649,#44650,#44651,#44652,#44653,#44654,
#44655,#44656,#44657,#44658,#44659,#44660,#44661,#44662,#44663,#44664,#44665,
#44666,#44667),.UNSPECIFIED.,.F.,.F.,(4,3,3,3,3,3,3,3,3,3,3,3,3,3,3,3,3,
3,3,3,3,3,3,3,4),(0.,0.05555555555555,0.106924267986465,0.1111111111111,
0.161796567291066,0.212394385898786,0.2222222222222,0.27465541537399,0.327511260060941,
0.3333333333333,0.389820070129939,0.4444444444444,0.503505530229127,0.5555555555556,
0.612328691897827,0.6666666666667,0.72222222222225,0.774969127013547,0.7777777777778,
0.82835260149752,0.87870895459855,0.8888888888889,0.941118027379493,0.996727628424779,
1.),.UNSPECIFIED.);
#2414=B_SPLINE_CURVE_WITH_KNOTS('',3,(#44668,#44669,#44670,#44671,#44672,
#44673,#44674,#44675,#44676,#44677,#44678,#44679,#44680,#44681,#44682,#44683,
#44684,#44685,#44686,#44687,#44688,#44689,#44690,#44691,#44692,#44693,#44694,
#44695,#44696,#44697,#44698,#44699,#44700,#44701,#44702,#44703,#44704,#44705,
#44706,#44707,#44708,#44709,#44710,#44711,#44712,#44713,#44714,#44715,#44716),
 .UNSPECIFIED.,.F.,.F.,(4,3,3,3,3,3,3,3,3,3,3,3,3,3,3,3,4),(4.33800647388095E-8,
0.115672156634637,0.179199191820932,0.2,0.292238719088017,0.378853944193901,
0.384477438176035,0.4,0.504607292126722,0.589623488819915,0.6,0.691024217930037,
0.782473470110827,0.794807707256916,0.8,0.903113049573187,0.999999723429614),
 .UNSPECIFIED.);
#2415=B_SPLINE_CURVE_WITH_KNOTS('',3,(#44754,#44755,#44756,#44757,#44758,
#44759,#44760,#44761,#44762,#44763,#44764,#44765,#44766,#44767,#44768,#44769,
#44770,#44771,#44772,#44773,#44774,#44775,#44776,#44777,#44778,#44779,#44780,
#44781,#44782,#44783,#44784,#44785,#44786,#44787,#44788,#44789,#44790,#44791,
#44792,#44793,#44794,#44795,#44796),.UNSPECIFIED.,.F.,.F.,(4,3,3,3,3,3,
3,3,3,3,3,3,3,3,4),(1.02489136070401E-6,2.78892909788713E-6,0.0898895600139057,
0.1666666666667,0.16666735661307,0.250000344973185,0.3333333333333,0.460510299335861,
0.5,0.60992454588341,0.6666666666667,0.778760920788974,0.8333333333333,
0.964311512862908,0.999999944055817),.UNSPECIFIED.);
#2416=B_SPLINE_CURVE_WITH_KNOTS('',3,(#44884,#44885,#44886,#44887,#44888,
#44889,#44890,#44891,#44892,#44893,#44894,#44895,#44896,#44897,#44898,#44899,
#44900,#44901,#44902,#44903,#44904,#44905,#44906,#44907,#44908,#44909,#44910,
#44911,#44912,#44913,#44914),.UNSPECIFIED.,.F.,.F.,(4,3,3,3,3,3,3,3,3,3,
4),(0.,0.2,0.4,0.6,0.600006275012996,0.721742469521887,0.799981987265399,
0.8,0.912452142717923,0.999991024190224,1.),.UNSPECIFIED.);
#2417=B_SPLINE_CURVE_WITH_KNOTS('',3,(#44975,#44976,#44977,#44978,#44979,
#44980,#44981,#44982,#44983,#44984,#44985,#44986,#44987,#44988,#44989,#44990,
#44991,#44992,#44993,#44994,#44995,#44996,#44997,#44998,#44999,#45000,#45001,
#45002,#45003,#45004,#45005),.UNSPECIFIED.,.F.,.F.,(4,3,3,3,3,3,3,3,3,3,
4),(4.98087268739273E-6,0.149736166300919,0.2,0.315183284203544,0.4,0.403962239763029,
0.6,0.768315918661213,0.8,0.880495757642992,1.),.UNSPECIFIED.);
#2418=B_SPLINE_CURVE_WITH_KNOTS('',3,(#45006,#45007,#45008,#45009,#45010,
#45011,#45012,#45013,#45014,#45015,#45016,#45017,#45018,#45019,#45020,#45021,
#45022,#45023,#45024,#45025,#45026,#45027,#45028,#45029,#45030,#45031,#45032,
#45033,#45034,#45035,#45036,#45037,#45038,#45039,#45040,#45041,#45042,#45043,
#45044,#45045,#45046,#45047,#45048,#45049,#45050,#45051,#45052,#45053,#45054,
#45055,#45056,#45057,#45058,#45059,#45060,#45061,#45062,#45063),
 .UNSPECIFIED.,.F.,.F.,(4,3,3,3,3,3,3,3,3,3,3,3,3,3,3,3,3,3,3,4),(0.,0.0785005850502826,
0.1428571428571,0.152289983519359,0.224965657458616,0.2857142857143,0.365357998177071,
0.4285714285714,0.495413593720157,0.562079339149973,0.5714285714286,0.58250627313346,
0.653487828717598,0.7142857142857,0.774274923856638,0.815018706983836,0.8571428571429,
0.924946709565138,0.992791568957691,1.),.UNSPECIFIED.);
#2419=B_SPLINE_CURVE_WITH_KNOTS('',3,(#45114,#45115,#45116,#45117,#45118,
#45119,#45120,#45121,#45122,#45123,#45124,#45125,#45126,#45127,#45128,#45129,
#45130,#45131,#45132,#45133,#45134,#45135,#45136,#45137,#45138,#45139,#45140,
#45141,#45142,#45143,#45144,#45145,#45146,#45147,#45148,#45149,#45150,#45151,
#45152,#45153,#45154,#45155,#45156,#45157,#45158,#45159,#45160,#45161,#45162,
#45163,#45164,#45165,#45166,#45167,#45168,#45169,#45170,#45171,#45172,#45173,
#45174,#45175,#45176,#45177,#45178,#45179,#45180),.UNSPECIFIED.,.F.,.F.,
(4,3,3,3,3,3,3,3,3,3,3,3,3,3,3,3,3,3,3,3,3,3,4),(1.52199927505013E-7,0.0615976282481722,
0.123466697458492,0.1428571428571,0.198336877388203,0.254197653065242,0.2857142857143,
0.351407196402381,0.416990445187705,0.4285714285714,0.476573915420894,0.524965880688773,
0.5714285714286,0.627091486629155,0.684253122670088,0.7142857142857,0.759626312948552,
0.804674497897221,0.848776226530048,0.8571428571429,0.911252892719779,0.96436009832331,
1.),.UNSPECIFIED.);
#2420=B_SPLINE_CURVE_WITH_KNOTS('',3,(#45325,#45326,#45327,#45328,#45329,
#45330,#45331,#45332,#45333,#45334,#45335,#45336,#45337,#45338,#45339,#45340,
#45341,#45342,#45343,#45344,#45345,#45346,#45347,#45348,#45349,#45350,#45351,
#45352,#45353,#45354,#45355,#45356,#45357,#45358,#45359,#45360,#45361,#45362,
#45363,#45364,#45365,#45366,#45367,#45368,#45369,#45370,#45371,#45372,#45373,
#45374,#45375,#45376,#45377,#45378,#45379,#45380,#45381,#45382,#45383,#45384,
#45385,#45386,#45387,#45388,#45389,#45390,#45391,#45392,#45393,#45394,#45395,
#45396,#45397,#45398,#45399,#45400,#45401,#45402,#45403,#45404,#45405,#45406,
#45407,#45408,#45409,#45410,#45411,#45412,#45413,#45414,#45415,#45416,#45417,
#45418,#45419,#45420,#45421,#45422,#45423,#45424,#45425,#45426,#45427,#45428,
#45429,#45430),.UNSPECIFIED.,.F.,.F.,(4,3,3,3,3,3,3,3,3,3,3,3,3,3,3,3,3,
3,3,3,3,3,3,3,3,3,3,3,3,3,3,3,3,3,3,4),(4.07533832038655E-8,0.0285863583342577,
0.0561745109866684,0.07142857142857,0.103500023873821,0.136613116776887,
0.1428571428571,0.164726875357122,0.203610380996657,0.2142857142857,0.255318345978842,
0.281307398781265,0.2857142857143,0.330530146034011,0.3571428571429,0.40506357525368,
0.414638109539121,0.4285714285714,0.4808296111022,0.5,0.549245837571629,
0.5714285714286,0.572143480381714,0.627101769658719,0.6428571428571,0.7102100620386,
0.7142857142857,0.742403038961964,0.7857142857143,0.839203130289171,0.8571428571429,
0.898082398123236,0.920731769414707,0.9285714285714,0.977975463981205,0.999993896438902),
 .UNSPECIFIED.);
#2421=B_SPLINE_CURVE_WITH_KNOTS('',3,(#45432,#45433,#45434,#45435,#45436,
#45437,#45438,#45439),.UNSPECIFIED.,.F.,.F.,(4,2,2,4),(-0.0527156059695698,
-0.0448511032213948,-0.0273145742577129,0.),.UNSPECIFIED.);
#2422=B_SPLINE_CURVE_WITH_KNOTS('',3,(#45514,#45515,#45516,#45517,#45518,
#45519,#45520,#45521,#45522,#45523,#45524,#45525,#45526,#45527),
 .UNSPECIFIED.,.F.,.F.,(4,2,2,2,2,2,4),(2.91925194763159E-6,0.0934696392563499,
0.166869193276301,0.18008495547347,0.185834312297566,0.188453342685018,
0.190941477315289),.UNSPECIFIED.);
#2423=B_SPLINE_CURVE_WITH_KNOTS('',3,(#45538,#45539,#45540,#45541,#45542,
#45543,#45544,#45545,#45546,#45547,#45548,#45549,#45550,#45551,#45552,#45553,
#45554,#45555,#45556,#45557,#45558,#45559,#45560,#45561,#45562,#45563,#45564,
#45565,#45566,#45567,#45568,#45569,#45570,#45571,#45572,#45573,#45574,#45575,
#45576,#45577,#45578,#45579,#45580,#45581,#45582,#45583,#45584,#45585,#45586,
#45587,#45588,#45589,#45590,#45591,#45592),.UNSPECIFIED.,.F.,.F.,(4,3,3,
3,3,3,3,3,3,3,3,3,3,3,3,3,3,3,4),(0.,0.0590659964221531,0.118210774712157,
0.125,0.215580128193309,0.25,0.3125,0.375,0.4375,0.5,0.606604025388335,
0.625,0.6875,0.75,0.805504989390552,0.860991155263171,0.875,0.943021966926566,
1.),.UNSPECIFIED.);
#2424=B_SPLINE_CURVE_WITH_KNOTS('',3,(#45648,#45649,#45650,#45651,#45652,
#45653,#45654,#45655,#45656,#45657,#45658,#45659,#45660,#45661,#45662,#45663,
#45664,#45665,#45666,#45667,#45668,#45669,#45670,#45671,#45672,#45673,#45674,
#45675,#45676,#45677,#45678,#45679,#45680,#45681,#45682,#45683,#45684,#45685,
#45686,#45687,#45688,#45689,#45690,#45691,#45692,#45693,#45694,#45695,#45696,
#45697,#45698,#45699,#45700,#45701,#45702,#45703,#45704,#45705),
 .UNSPECIFIED.,.F.,.F.,(4,3,3,3,3,3,3,3,3,3,3,3,3,3,3,3,3,3,3,4),(0.,0.000317629015129917,
0.0773853855433874,0.125,0.17861003880418,0.232539979538112,0.25,0.328925013375417,
0.375,0.46719173907792,0.5,0.563115540635534,0.625,0.706667897106718,0.75,
0.826211882215789,0.875,0.945358955314075,0.99986711918626,1.),
 .UNSPECIFIED.);
#2425=B_SPLINE_CURVE_WITH_KNOTS('',3,(#45824,#45825,#45826,#45827,#45828,
#45829,#45830,#45831,#45832,#45833,#45834,#45835,#45836,#45837,#45838,#45839,
#45840,#45841,#45842,#45843,#45844,#45845,#45846,#45847,#45848,#45849,#45850,
#45851,#45852,#45853,#45854,#45855,#45856,#45857,#45858,#45859,#45860,#45861,
#45862,#45863,#45864,#45865,#45866,#45867,#45868,#45869,#45870,#45871,#45872,
#45873,#45874,#45875,#45876,#45877,#45878,#45879,#45880,#45881,#45882,#45883,
#45884,#45885,#45886,#45887),.UNSPECIFIED.,.F.,.F.,(4,3,3,3,3,3,3,3,3,3,
3,3,3,3,3,3,3,3,3,3,3,4),(1.1164216272441E-6,1.64886277366089E-6,0.0294346969467261,
0.0615346142090942,0.07142857142857,0.122235287796492,0.1428571428571,0.2142857142857,
0.2857142857143,0.3571428571429,0.4285714285714,0.5,0.5714285714286,0.6428571428571,
0.7142857142857,0.7857142857143,0.842909114801495,0.8571428571429,0.904173100246843,
0.9285714285714,0.993096032114401,1.),.UNSPECIFIED.);
#2426=B_SPLINE_CURVE_WITH_KNOTS('',3,(#45889,#45890,#45891,#45892,#45893,
#45894,#45895,#45896,#45897,#45898,#45899,#45900,#45901,#45902,#45903,#45904,
#45905,#45906,#45907,#45908,#45909,#45910,#45911,#45912,#45913,#45914,#45915,
#45916,#45917,#45918,#45919,#45920,#45921,#45922,#45923,#45924,#45925,#45926,
#45927,#45928,#45929,#45930,#45931,#45932,#45933,#45934,#45935,#45936,#45937,
#45938,#45939,#45940),.UNSPECIFIED.,.F.,.F.,(4,3,3,3,3,3,3,3,3,3,3,3,3,
3,3,3,3,4),(8.6778036994424E-7,0.0586819159367273,0.07142857142857,0.1428571428571,
0.2142857142857,0.2857142857143,0.3571428571429,0.4285714285714,0.5,0.5714285714286,
0.6428571428571,0.7142857142857,0.7857142857143,0.8571428571429,0.920068145469386,
0.9285714285714,0.994698303801108,1.),.UNSPECIFIED.);
#2427=B_SPLINE_CURVE_WITH_KNOTS('',3,(#46022,#46023,#46024,#46025,#46026,
#46027,#46028,#46029),.UNSPECIFIED.,.F.,.F.,(4,1,1,1,1,4),(8.18300672274726E-6,
0.2,0.4,0.6,0.8,1.),.UNSPECIFIED.);
#2428=B_SPLINE_CURVE_WITH_KNOTS('',3,(#46066,#46067,#46068,#46069),
 .UNSPECIFIED.,.F.,.F.,(4,4),(-0.000287379327346715,0.),.UNSPECIFIED.);
#2429=B_SPLINE_CURVE_WITH_KNOTS('',3,(#46071,#46072,#46073,#46074,#46075,
#46076,#46077,#46078,#46079,#46080,#46081,#46082,#46083,#46084,#46085,#46086,
#46087,#46088,#46089,#46090,#46091,#46092,#46093,#46094,#46095,#46096,#46097,
#46098,#46099,#46100,#46101,#46102,#46103,#46104,#46105,#46106,#46107,#46108,
#46109,#46110,#46111,#46112,#46113,#46114,#46115,#46116,#46117,#46118,#46119,
#46120,#46121,#46122,#46123,#46124,#46125,#46126,#46127,#46128,#46129,#46130,
#46131,#46132,#46133,#46134,#46135,#46136,#46137,#46138,#46139,#46140,#46141,
#46142,#46143,#46144,#46145,#46146,#46147,#46148,#46149,#46150,#46151,#46152,
#46153,#46154,#46155,#46156,#46157,#46158,#46159,#46160,#46161,#46162,#46163,
#46164),.UNSPECIFIED.,.F.,.F.,(4,3,3,3,3,3,3,3,3,3,3,3,3,3,3,3,3,3,3,3,
3,3,3,3,3,3,3,3,3,3,3,4),(0.,0.0334880516165954,0.0622449481709034,0.0833304545710313,
0.123139222900696,0.158240223188287,0.176189139696093,0.217007009430374,
0.243869787273509,0.26354322405106,0.302458774449498,0.33355876922255,0.374434885871789,
0.405321381393714,0.426172721464637,0.480843228725633,0.507476669962832,
0.544616299200151,0.574867627238567,0.592227140301538,0.637891373171595,
0.668397489031486,0.7156914768719,0.744145082796372,0.770511427895059,0.813365315244751,
0.836703116619631,0.881940300050722,0.91091246542526,0.927753817005376,
0.962791389277124,0.997828961548873),.UNSPECIFIED.);
#2430=B_SPLINE_CURVE_WITH_KNOTS('',3,(#46166,#46167,#46168,#46169),
 .UNSPECIFIED.,.F.,.F.,(4,4),(-0.00107348259049816,0.),.UNSPECIFIED.);
#2431=B_SPLINE_CURVE_WITH_KNOTS('',3,(#46171,#46172,#46173,#46174,#46175,
#46176,#46177,#46178,#46179,#46180,#46181,#46182,#46183,#46184),
 .UNSPECIFIED.,.F.,.F.,(4,2,2,2,2,2,4),(-0.747237513889951,-0.627110670602595,
-0.492162734458781,-0.361378717436516,-0.240449917906045,-0.127292557609884,
-2.3301729044132E-6),.UNSPECIFIED.);
#2432=B_SPLINE_CURVE_WITH_KNOTS('',3,(#46185,#46186,#46187,#46188,#46189,
#46190,#46191,#46192,#46193,#46194,#46195,#46196,#46197,#46198,#46199,#46200),
 .UNSPECIFIED.,.F.,.F.,(4,2,2,2,2,2,2,4),(-0.557266864962719,-0.476580853062999,
-0.396866002960756,-0.315372123091983,-0.242726490281515,-0.148650466132605,
-0.073950688870771,-0.000468069961644113),.UNSPECIFIED.);
#2433=B_SPLINE_CURVE_WITH_KNOTS('',3,(#46239,#46240,#46241,#46242,#46243,
#46244,#46245,#46246,#46247,#46248),.UNSPECIFIED.,.F.,.F.,(4,2,2,2,4),(-0.373790461969616,
-0.353425955511238,-0.32400441351636,-0.295535379633958,-0.267904010196117),
 .UNSPECIFIED.);
#2434=B_SPLINE_CURVE_WITH_KNOTS('',3,(#46250,#46251,#46252,#46253,#46254,
#46255,#46256,#46257,#46258,#46259,#46260),.UNSPECIFIED.,.F.,.F.,(4,2,3,
2,4),(-0.218968937117933,-0.202250368267603,0.,0.202250368267602,0.21896893711841),
 .UNSPECIFIED.);
#2435=B_SPLINE_CURVE_WITH_KNOTS('',3,(#46262,#46263,#46264,#46265,#46266,
#46267,#46268,#46269,#46270,#46271),.UNSPECIFIED.,.F.,.F.,(4,2,2,2,4),(0.267904010196053,
0.295535379633939,0.324004413516362,0.353425955511275,0.37379046196938),
 .UNSPECIFIED.);
#2436=B_SPLINE_CURVE_WITH_KNOTS('',3,(#46273,#46274,#46275,#46276,#46277,
#46278,#46279,#46280,#46281,#46282,#46283),.UNSPECIFIED.,.F.,.F.,(4,2,3,
2,4),(-0.218968937118539,-0.202250368267599,0.,0.202250368267599,0.218968937117935),
 .UNSPECIFIED.);
#2437=B_SPLINE_CURVE_WITH_KNOTS('',3,(#46285,#46286,#46287,#46288,#46289,
#46290,#46291,#46292,#46293,#46294),.UNSPECIFIED.,.F.,.F.,(4,2,2,2,4),(0.26790401019593,
0.295535379633943,0.324004413516341,0.353425955511207,0.373790461969294),
 .UNSPECIFIED.);
#2438=B_SPLINE_CURVE_WITH_KNOTS('',3,(#46296,#46297,#46298,#46299,#46300,
#46301,#46302,#46303,#46304,#46305,#46306),.UNSPECIFIED.,.F.,.F.,(4,2,3,
2,4),(-0.218968937118688,-0.20225036826751,0.,0.202250368267511,0.218968937117607),
 .UNSPECIFIED.);
#2439=B_SPLINE_CURVE_WITH_KNOTS('',3,(#46308,#46309,#46310,#46311,#46312,
#46313,#46314,#46315,#46316,#46317),.UNSPECIFIED.,.F.,.F.,(4,2,2,2,4),(0.267904010195979,
0.295535379633993,0.324004413516352,0.353425955511146,0.373790461969576),
 .UNSPECIFIED.);
#2440=B_SPLINE_CURVE_WITH_KNOTS('',3,(#46319,#46320,#46321,#46322,#46323,
#46324,#46325,#46326,#46327,#46328,#46329),.UNSPECIFIED.,.F.,.F.,(4,2,3,
2,4),(-0.218968937118343,-0.202250368267423,0.,0.202250368267423,0.218968937117866),
 .UNSPECIFIED.);
#2441=B_SPLINE_CURVE_WITH_KNOTS('',3,(#46331,#46332,#46333,#46334,#46335,
#46336,#46337,#46338,#46339,#46340),.UNSPECIFIED.,.F.,.F.,(4,2,2,2,4),(0.267904010196159,
0.295535379634028,0.324004413516362,0.353425955511117,0.373790461969744),
 .UNSPECIFIED.);
#2442=B_SPLINE_CURVE_WITH_KNOTS('',3,(#46342,#46343,#46344,#46345,#46346,
#46347),.UNSPECIFIED.,.F.,.F.,(4,2,4),(0.,0.202250368267416,0.21896893711845),
 .UNSPECIFIED.);
#2443=B_SPLINE_CURVE_WITH_KNOTS('',3,(#46352,#46353,#46354,#46355,#46356,
#46357),.UNSPECIFIED.,.F.,.F.,(4,2,4),(-0.218968937117756,-0.202250368267416,
0.),.UNSPECIFIED.);
#2444=B_SPLINE_CURVE_WITH_KNOTS('',3,(#46359,#46360,#46361,#46362,#46363,
#46364,#46365,#46366,#46367,#46368),.UNSPECIFIED.,.F.,.F.,(4,2,2,2,4),(0.267904010196074,
0.295535379633993,0.324004413516349,0.353425955511146,0.373790461969709),
 .UNSPECIFIED.);
#2445=B_SPLINE_CURVE_WITH_KNOTS('',3,(#46369,#46370,#46371,#46372,#46373,
#46374,#46375,#46376,#46377,#46378,#46379),.UNSPECIFIED.,.F.,.F.,(4,2,3,
2,4),(-0.218968937117586,-0.202250368267507,0.,0.202250368267507,0.218968937118666),
 .UNSPECIFIED.);
#2446=B_SPLINE_CURVE_WITH_KNOTS('',3,(#46414,#46415,#46416,#46417,#46418,
#46419,#46420,#46421,#46422,#46423,#46424,#46425,#46426,#46427,#46428,#46429,
#46430,#46431,#46432,#46433,#46434,#46435,#46436,#46437,#46438,#46439),
 .UNSPECIFIED.,.F.,.F.,(4,2,2,2,2,2,2,2,2,2,2,2,4),(1.6778324559149,1.72014131704469,
1.79018729092096,1.88481538797586,1.95967575697182,2.03596140156688,2.11055839736739,
2.1861310055091,2.25999784739323,2.32219814460217,2.41722647505349,2.46648828140439,
2.51647759383358),.UNSPECIFIED.);
#2447=B_SPLINE_CURVE_WITH_KNOTS('',3,(#46442,#46443,#46444,#46445,#46446,
#46447,#46448,#46449,#46450,#46451,#46452,#46453,#46454,#46455,#46456,#46457,
#46458,#46459,#46460,#46461,#46462,#46463,#46464,#46465,#46466,#46467,#46468,
#46469,#46470,#46471,#46472,#46473,#46474,#46475,#46476,#46477,#46478,#46479,
#46480,#46481,#46482,#46483,#46484,#46485,#46486,#46487),.UNSPECIFIED.,
 .F.,.F.,(4,2,2,2,2,2,2,2,2,2,2,2,2,2,2,2,2,2,2,2,2,2,4),(1.15114226328039E-5,
0.0649848036365928,0.127981322338831,0.255478974596226,0.331652000771546,
0.409872196413906,0.486219934049148,0.564442937902226,0.640587838009818,
0.718804933776125,0.795179715777592,0.873400886535082,0.949509589781659,
1.02772338331364,1.10413447964806,1.18235401068144,1.25841586014867,1.33116362067197,
1.39373306987938,1.45442777298624,1.59477450954928,1.63378500658915,1.6778324559149),
 .UNSPECIFIED.);
#2448=B_SPLINE_CURVE_WITH_KNOTS('',3,(#46490,#46491,#46492,#46493,#46494,
#46495),.UNSPECIFIED.,.F.,.F.,(4,2,4),(-0.0531336167389032,-0.0265660123967773,
-4.38116269941419E-6),.UNSPECIFIED.);
#2449=B_SPLINE_CURVE_WITH_KNOTS('',3,(#46497,#46498,#46499,#46500,#46501,
#46502),.UNSPECIFIED.,.F.,.F.,(4,2,4),(-0.0218956957452984,-0.0109537633218819,
-1.19176186653708E-5),.UNSPECIFIED.);
#2450=B_SPLINE_CURVE_WITH_KNOTS('',3,(#46503,#46504,#46505,#46506,#46507,
#46508),.UNSPECIFIED.,.F.,.F.,(4,2,4),(-0.0531191162051923,-0.026569992816066,
-2.41222135409933E-6),.UNSPECIFIED.);
#2451=B_SPLINE_CURVE_WITH_KNOTS('',3,(#46779,#46780,#46781,#46782,#46783,
#46784,#46785,#46786,#46787,#46788,#46789,#46790,#46791,#46792,#46793,#46794,
#46795,#46796,#46797,#46798,#46799,#46800,#46801,#46802,#46803,#46804,#46805,
#46806,#46807,#46808,#46809,#46810,#46811,#46812,#46813,#46814,#46815,#46816,
#46817,#46818,#46819,#46820,#46821,#46822,#46823,#46824,#46825,#46826,#46827,
#46828,#46829,#46830,#46831,#46832,#46833,#46834,#46835,#46836,#46837,#46838,
#46839,#46840,#46841,#46842),.UNSPECIFIED.,.F.,.F.,(4,2,2,2,2,2,2,2,2,2,
2,2,2,2,2,2,2,2,2,2,2,2,2,2,2,2,2,2,2,2,2,4),(7.36481248802261E-6,0.0579261863271751,
0.114674480656631,0.225347966852895,0.303563316130361,0.375602352513824,
0.453406536051233,0.52859202455298,0.606172616816621,0.682782389736415,
0.749975319947736,0.789346627707107,0.867396567563414,0.945814740155127,
1.02375669910915,1.10207765612309,1.2603944919097,1.41863075344829,1.57694494459286,
1.65531768858497,1.73329243799722,1.81176162349561,1.88982856427288,1.92921183430251,
1.99622866693818,2.07313536180107,2.15061317674896,2.22631027196354,2.3039857757181,
2.41210220258,2.46759986362207,2.52414659527546),.UNSPECIFIED.);
#2452=B_SPLINE_CURVE_WITH_KNOTS('',3,(#46843,#46844,#46845,#46846,#46847,
#46848,#46849,#46850,#46851,#46852,#46853,#46854,#46855,#46856,#46857,#46858,
#46859,#46860,#46861,#46862,#46863,#46864,#46865,#46866,#46867,#46868,#46869,
#46870,#46871,#46872,#46873,#46874,#46875,#46876,#46877,#46878,#46879,#46880,
#46881,#46882,#46883,#46884,#46885,#46886,#46887,#46888,#46889,#46890,#46891,
#46892,#46893,#46894,#46895,#46896,#46897,#46898,#46899,#46900,#46901,#46902,
#46903,#46904,#46905,#46906,#46907,#46908,#46909,#46910,#46911,#46912,#46913,
#46914,#46915,#46916,#46917,#46918,#46919,#46920,#46921,#46922,#46923,#46924,
#46925,#46926,#46927,#46928,#46929,#46930,#46931,#46932,#46933,#46934,#46935,
#46936,#46937,#46938,#46939,#46940,#46941,#46942,#46943,#46944,#46945,#46946,
#46947,#46948,#46949,#46950,#46951,#46952,#46953,#46954,#46955,#46956,#46957,
#46958,#46959,#46960,#46961,#46962,#46963,#46964,#46965,#46966,#46967,#46968,
#46969,#46970,#46971,#46972,#46973,#46974,#46975,#46976,#46977,#46978,#46979,
#46980,#46981,#46982,#46983,#46984,#46985,#46986,#46987,#46988,#46989,#46990,
#46991,#46992,#46993,#46994,#46995,#46996,#46997,#46998,#46999,#47000,#47001,
#47002,#47003,#47004,#47005,#47006,#47007,#47008,#47009,#47010),
 .UNSPECIFIED.,.F.,.F.,(4,2,2,2,2,2,2,2,2,2,2,2,2,2,2,2,2,2,2,2,2,2,2,2,
2,2,2,2,2,2,2,2,2,2,2,2,2,2,2,2,2,2,2,2,2,2,2,2,2,2,2,2,2,2,2,2,2,2,2,2,
2,2,2,2,2,2,2,2,2,2,2,2,2,2,2,2,2,2,2,2,2,2,2,4),(1.24307839451921E-5,0.0500273781858429,
0.099432803829234,0.195716540713382,0.25931817354893,0.337078262407541,
0.41344857617591,0.491361811458937,0.567992316284045,0.685555037500459,
0.763791026299535,0.843756617848861,0.882404673909104,0.998511957697595,
1.03743102042921,1.15497455383376,1.2340055935132,1.31470136763013,1.35366727028043,
1.47047427818367,1.50973762807098,1.58913673742986,1.66712864886114,1.74668253295675,
1.82493349101501,1.90462011905243,1.98308203374839,2.0628836750312,2.14151982609838,
2.26262206703986,2.34260764228006,2.42442363424022,2.50469828881245,2.58645550422729,
2.64529450774882,2.6857733268076,2.76607475517718,2.84663676425656,2.92676812082607,
3.00717695406304,3.16980613391867,3.33233948572403,3.49488234557123,3.57373135676786,
3.65370773327419,3.73415195068027,3.81430460423484,3.8948941969404,3.97521273743168,
4.01569959042438,4.07557765927915,4.15735964286485,4.23756779460293,4.31940929267925,
4.39932515385298,4.52048519992014,4.59929039046647,4.76196968485967,4.9245887247453,
5.08724026339377,5.16760525699317,5.24765305595157,5.3281517942438,5.40837336056063,
5.44882670984173,5.50987808032324,5.59161240552458,5.67174675036586,5.75354015640541,
5.83338037483471,5.9548614177171,6.0337228672632,6.19633644131774,6.35890538617673,
6.5215321367131,6.60193149454333,6.68203660128082,6.76257971195663,6.84285225787908,
6.88331730866563,6.94338925665242,7.02513015990786,7.09949049144025,7.17394332972263),
 .UNSPECIFIED.);
#2453=B_SPLINE_CURVE_WITH_KNOTS('',3,(#47012,#47013,#47014,#47015,#47016,
#47017,#47018,#47019,#47020,#47021,#47022,#47023,#47024,#47025,#47026,#47027,
#47028,#47029,#47030,#47031,#47032,#47033,#47034,#47035,#47036,#47037,#47038,
#47039,#47040,#47041,#47042,#47043,#47044,#47045,#47046,#47047,#47048,#47049,
#47050,#47051,#47052,#47053,#47054,#47055,#47056,#47057,#47058,#47059,#47060,
#47061,#47062,#47063,#47064,#47065,#47066,#47067,#47068,#47069,#47070,#47071,
#47072,#47073,#47074,#47075,#47076,#47077,#47078,#47079,#47080,#47081,#47082,
#47083,#47084,#47085,#47086,#47087,#47088,#47089,#47090,#47091,#47092,#47093,
#47094,#47095,#47096,#47097,#47098,#47099,#47100,#47101,#47102,#47103,#47104,
#47105,#47106,#47107,#47108,#47109,#47110,#47111,#47112,#47113,#47114,#47115,
#47116,#47117,#47118,#47119,#47120,#47121,#47122,#47123,#47124,#47125,#47126,
#47127,#47128,#47129,#47130,#47131,#47132,#47133,#47134,#47135,#47136,#47137,
#47138,#47139,#47140,#47141,#47142,#47143,#47144,#47145,#47146,#47147,#47148,
#47149,#47150,#47151,#47152,#47153,#47154,#47155,#47156,#47157,#47158,#47159,
#47160,#47161,#47162,#47163,#47164,#47165,#47166,#47167,#47168,#47169,#47170,
#47171,#47172,#47173,#47174,#47175,#47176,#47177,#47178,#47179,#47180,#47181,
#47182,#47183,#47184,#47185,#47186,#47187,#47188,#47189,#47190,#47191,#47192,
#47193,#47194,#47195,#47196,#47197,#47198,#47199,#47200,#47201,#47202,#47203,
#47204,#47205,#47206,#47207,#47208,#47209,#47210,#47211,#47212,#47213,#47214,
#47215,#47216,#47217,#47218,#47219,#47220,#47221,#47222,#47223,#47224,#47225,
#47226,#47227,#47228,#47229,#47230,#47231,#47232,#47233,#47234,#47235,#47236,
#47237,#47238,#47239,#47240,#47241,#47242,#47243,#47244,#47245,#47246,#47247,
#47248,#47249,#47250,#47251,#47252,#47253,#47254,#47255,#47256,#47257,#47258,
#47259,#47260,#47261,#47262,#47263,#47264,#47265,#47266,#47267,#47268,#47269,
#47270,#47271,#47272,#47273,#47274,#47275,#47276,#47277,#47278,#47279,#47280,
#47281,#47282,#47283,#47284,#47285,#47286,#47287,#47288,#47289,#47290,#47291,
#47292,#47293,#47294,#47295,#47296,#47297,#47298,#47299,#47300,#47301,#47302,
#47303,#47304,#47305,#47306,#47307,#47308,#47309,#47310,#47311,#47312,#47313,
#47314,#47315,#47316,#47317,#47318,#47319,#47320,#47321,#47322,#47323,#47324,
#47325,#47326,#47327,#47328,#47329,#47330,#47331,#47332,#47333,#47334,#47335,
#47336,#47337,#47338,#47339,#47340,#47341,#47342,#47343,#47344,#47345,#47346,
#47347,#47348,#47349,#47350,#47351,#47352,#47353,#47354,#47355,#47356,#47357,
#47358,#47359,#47360,#47361,#47362,#47363,#47364,#47365,#47366,#47367,#47368,
#47369,#47370,#47371,#47372,#47373,#47374,#47375,#47376,#47377,#47378,#47379,
#47380,#47381,#47382,#47383,#47384,#47385,#47386,#47387,#47388,#47389,#47390,
#47391,#47392,#47393,#47394,#47395,#47396,#47397,#47398,#47399,#47400,#47401,
#47402,#47403,#47404,#47405,#47406,#47407,#47408,#47409,#47410,#47411,#47412,
#47413,#47414,#47415,#47416,#47417,#47418,#47419,#47420,#47421,#47422,#47423,
#47424,#47425,#47426,#47427,#47428,#47429,#47430,#47431,#47432,#47433,#47434,
#47435,#47436,#47437,#47438,#47439,#47440,#47441,#47442,#47443,#47444,#47445,
#47446,#47447,#47448,#47449,#47450,#47451,#47452,#47453,#47454,#47455,#47456,
#47457,#47458,#47459,#47460,#47461,#47462,#47463,#47464,#47465,#47466,#47467,
#47468,#47469,#47470,#47471,#47472,#47473,#47474,#47475,#47476,#47477,#47478,
#47479,#47480,#47481,#47482,#47483,#47484,#47485,#47486,#47487,#47488,#47489,
#47490,#47491,#47492,#47493,#47494,#47495,#47496,#47497,#47498,#47499,#47500,
#47501,#47502,#47503,#47504,#47505,#47506,#47507,#47508,#47509,#47510,#47511,
#47512,#47513,#47514,#47515,#47516,#47517,#47518,#47519,#47520,#47521,#47522,
#47523,#47524,#47525,#47526,#47527,#47528,#47529,#47530,#47531,#47532,#47533,
#47534,#47535,#47536,#47537,#47538,#47539,#47540,#47541,#47542,#47543,#47544,
#47545,#47546,#47547,#47548,#47549,#47550,#47551,#47552,#47553,#47554,#47555,
#47556,#47557,#47558,#47559,#47560,#47561,#47562,#47563,#47564,#47565,#47566,
#47567,#47568,#47569,#47570,#47571,#47572,#47573,#47574,#47575,#47576,#47577,
#47578,#47579,#47580,#47581,#47582,#47583,#47584,#47585,#47586,#47587,#47588,
#47589,#47590,#47591,#47592,#47593,#47594,#47595,#47596,#47597,#47598,#47599,
#47600,#47601,#47602,#47603,#47604,#47605,#47606,#47607,#47608,#47609,#47610,
#47611,#47612,#47613,#47614,#47615,#47616,#47617,#47618,#47619,#47620,#47621,
#47622,#47623,#47624),.UNSPECIFIED.,.F.,.F.,(4,3,3,3,3,3,3,3,3,3,3,3,3,
3,3,3,3,3,3,3,3,3,3,3,3,3,3,3,3,3,3,3,3,3,3,3,3,3,3,3,3,3,3,3,3,3,3,3,3,
3,3,3,3,3,3,3,3,3,3,3,3,3,3,3,3,3,3,3,3,3,3,3,3,3,3,3,3,3,3,3,3,3,3,3,3,
3,3,3,3,3,3,3,3,3,3,3,3,3,3,3,3,3,3,3,3,3,3,3,3,3,3,3,3,3,3,3,3,3,3,3,3,
3,3,3,3,3,3,3,3,3,3,3,3,3,3,3,3,3,3,3,3,3,3,3,3,3,3,3,3,3,3,3,3,3,3,3,3,
3,3,3,3,3,3,3,3,3,3,3,3,3,3,3,3,3,3,3,3,3,3,3,3,3,3,3,3,3,3,3,3,3,3,3,3,
3,3,3,3,3,3,3,3,3,3,3,4),(3.25655971975498E-10,0.006896551724138,0.0124999836137833,
0.01379310344828,0.02068965517241,0.02758620689655,0.0287500147726358,0.03448275862069,
0.04137931034483,0.0449999960540127,0.04827586206897,0.0551724137931,0.061249990576592,
0.06206896551724,0.06896551724138,0.07586206896552,0.0775000201460335,0.08275862068966,
0.08965517241379,0.0937499863389232,0.09655172413793,0.1034482758621,0.109999997295967,
0.1103448275862,0.1172413793103,0.1241379310345,0.126250021167855,0.1310344827586,
0.1379310344828,0.142499980080655,0.1448275862069,0.151724137931,0.1586206896552,
0.15875000071435,0.1655172413793,0.1724137931034,0.17500001705366,0.1793103448276,
0.1862068965517,0.191249978763953,0.1931034482759,0.2,0.2068965517241,0.207500006105615,
0.2137931034483,0.2206896551724,0.223750008641753,0.2275862068966,0.2344827586207,
0.239999982367645,0.2413793103448,0.248275862069,0.2551724137931,0.256250013484736,
0.2620689655172,0.2689655172414,0.272499998025251,0.2758620689655,0.2827586206897,
0.288749989207179,0.2896551724138,0.2965517241379,0.3034482758621,0.305000019440364,
0.3103448275862,0.3172413793103,0.321249987913626,0.3241379310345,0.3310344827586,
0.337499996263586,0.3379310344828,0.3448275862069,0.351724137931,0.353750021363703,
0.3586206896552,0.3655172413793,0.369999980876539,0.3724137931034,0.3793103448276,
0.3862068965517,0.3931034482759,0.4,0.40250001816575,0.4068965517241,0.4137931034483,
0.41874997861438,0.4206896551724,0.4275862068966,0.4344827586207,0.435000004876984,
0.4413793103448,0.448275862069,0.451250010408905,0.4551724137931,0.4620689655172,
0.46749998140113,0.4689655172414,0.4758620689655,0.4827586206897,0.483750012153462,
0.4896551724138,0.4965517241379,0.499999999999995,0.5034482758621,0.5103448275862,
0.516249987846535,0.5172413793103,0.5241379310345,0.5310344827586,0.532500018598869,
0.5379310344828,0.5448275862069,0.548749989591095,0.551724137931,0.5586206896552,
0.564999995123012,0.5655172413793,0.5724137931034,0.5793103448276,0.581250021385624,
0.5862068965517,0.5931034482759,0.597499981834243,0.6,0.6068965517241,0.6137931034483,
0.6206896551724,0.6275862068966,0.630000019123452,0.6344827586207,0.6413793103448,
0.646249978636291,0.648275862069,0.6551724137931,0.6620689655172,0.662500003736419,
0.6689655172414,0.6758620689655,0.678750012086381,0.6827586206897,0.6896551724138,
0.694999980559641,0.6965517241379,0.7034482758621,0.7103448275862,0.711250010792824,
0.7172413793103,0.7241379310345,0.727500001974746,0.7310344827586,0.7379310344828,
0.743749986515264,0.7448275862069,0.751724137931,0.7586206896552,0.760000017632363,
0.7655172413793,0.7724137931034,0.776249991358243,0.7793103448276,0.7862068965517,
0.792499993894376,0.7931034482759,0.8,0.8068965517241,0.808750021236045,
0.8137931034483,0.8206896551724,0.82499998294634,0.8275862068966,0.8344827586207,
0.841249999285646,0.8413793103448,0.848275862069,0.8551724137931,0.85750001991935,
0.8620689655172,0.8689655172414,0.873749978832143,0.8758620689655,0.8827586206897,
0.8896551724138,0.890000002704033,0.8965517241379,0.9034482758621,0.906250013661082,
0.9103448275862,0.9172413793103,0.922499979853959,0.9241379310345,0.9310344827586,
0.9379310344828,0.938750009423415,0.9448275862069,0.951724137931,0.955000003945983,
0.9586206896552,0.9655172413793,0.971249985227355,0.9724137931034,0.9793103448276,
0.9862068965517,0.98750001638623,0.9931034482759,0.999999999088867),
 .UNSPECIFIED.);
#2454=B_SPLINE_CURVE_WITH_KNOTS('',3,(#47895,#47896,#47897,#47898,#47899,
#47900,#47901,#47902,#47903,#47904,#47905,#47906,#47907,#47908,#47909,#47910,
#47911,#47912,#47913,#47914,#47915,#47916,#47917,#47918,#47919,#47920,#47921,
#47922,#47923,#47924,#47925,#47926,#47927,#47928,#47929,#47930,#47931,#47932,
#47933,#47934,#47935,#47936,#47937,#47938,#47939,#47940,#47941,#47942,#47943,
#47944,#47945,#47946,#47947,#47948,#47949,#47950,#47951,#47952,#47953,#47954,
#47955,#47956,#47957,#47958,#47959,#47960,#47961,#47962,#47963,#47964,#47965,
#47966,#47967,#47968,#47969,#47970,#47971,#47972,#47973,#47974,#47975,#47976,
#47977,#47978,#47979,#47980,#47981,#47982,#47983,#47984,#47985,#47986,#47987,
#47988,#47989,#47990,#47991,#47992,#47993,#47994,#47995,#47996,#47997,#47998,
#47999,#48000,#48001,#48002,#48003,#48004,#48005,#48006,#48007,#48008,#48009,
#48010,#48011,#48012,#48013,#48014,#48015,#48016,#48017,#48018,#48019,#48020,
#48021,#48022,#48023,#48024,#48025,#48026,#48027,#48028,#48029,#48030,#48031,
#48032,#48033,#48034,#48035,#48036,#48037,#48038,#48039,#48040,#48041,#48042,
#48043,#48044,#48045,#48046,#48047,#48048,#48049,#48050,#48051,#48052,#48053,
#48054,#48055,#48056,#48057,#48058,#48059,#48060),.UNSPECIFIED.,.F.,.F.,
(4,2,2,2,2,2,2,2,2,2,2,2,2,2,2,2,2,2,2,2,2,2,2,2,2,2,2,2,2,2,2,2,2,2,2,
2,2,2,2,2,2,2,2,2,2,2,2,2,2,2,2,2,2,2,2,2,2,2,2,2,2,2,2,2,2,2,2,2,2,2,2,
2,2,2,2,2,2,2,2,2,2,2,4),(1.24307838879642E-5,0.0646066183114824,0.12856607719689,
0.254865757065513,0.372586486589494,0.449979962307396,0.529184791067371,
0.606862719354848,0.686010979860581,0.744503176051179,0.783677591093499,
0.861352736963718,0.939287795082856,1.09685206179482,1.25431390180843,1.41176835032023,
1.48820524639062,1.60667073493631,1.68398378903913,1.76316312364665,1.80149266896066,
1.87901566013445,1.95514961899729,2.03282673397556,2.10922039203301,2.18702955426342,
2.26363435169808,2.3415577655465,2.41833663806098,2.53655733854788,2.61466702094577,
2.69456135835026,2.77295307250581,2.8527899969026,2.91011937237683,2.94964851629334,
3.02806833447274,3.10674296165139,3.18499796256133,3.26352190353714,3.42232679541464,
3.50005504605113,3.65720764541172,3.81435430173883,3.8922586891329,3.97064841787099,
4.04872265952644,4.1272404412672,4.20548511978754,4.28415133142332,4.36254991085045,
4.40206259190978,4.45974116890874,4.53954264803744,4.61782220009431,4.69768194550285,
4.77567736887365,4.89370244308361,4.97054560362708,5.04848147348265,5.12518346334503,
5.20301839793177,5.27955407125725,5.35727542243828,5.43361193177689,5.5112037764545,
5.587297988917,5.66474041371507,5.70304440969069,5.81603976418334,5.85399652301374,
5.93267626293519,6.00983067657395,6.08856751052276,6.16543987971809,6.28216635188411,
6.35802486747928,6.51454555434391,6.67101557798643,6.82752506424321,6.86956990518419,
6.93242642201505,6.99601164762652),.UNSPECIFIED.);
#2455=B_SPLINE_CURVE_WITH_KNOTS('',3,(#48064,#48065,#48066,#48067,#48068,
#48069,#48070,#48071,#48072,#48073,#48074,#48075,#48076,#48077,#48078,#48079,
#48080,#48081,#48082,#48083,#48084,#48085,#48086,#48087,#48088,#48089,#48090,
#48091,#48092,#48093,#48094,#48095,#48096,#48097,#48098,#48099,#48100,#48101,
#48102,#48103,#48104,#48105,#48106,#48107,#48108,#48109,#48110,#48111,#48112,
#48113,#48114,#48115,#48116,#48117,#48118,#48119,#48120,#48121,#48122,#48123,
#48124,#48125,#48126,#48127,#48128,#48129,#48130,#48131,#48132,#48133,#48134,
#48135,#48136,#48137,#48138,#48139,#48140,#48141,#48142,#48143,#48144,#48145,
#48146,#48147,#48148,#48149,#48150,#48151,#48152,#48153,#48154,#48155,#48156,
#48157,#48158,#48159,#48160,#48161,#48162,#48163,#48164,#48165,#48166,#48167,
#48168,#48169,#48170,#48171,#48172,#48173,#48174,#48175,#48176,#48177,#48178,
#48179,#48180,#48181,#48182,#48183,#48184,#48185,#48186,#48187,#48188,#48189,
#48190,#48191,#48192,#48193,#48194,#48195,#48196,#48197,#48198,#48199,#48200,
#48201,#48202,#48203,#48204,#48205,#48206,#48207,#48208,#48209,#48210,#48211,
#48212,#48213,#48214,#48215,#48216,#48217,#48218,#48219,#48220,#48221,#48222,
#48223,#48224,#48225,#48226,#48227,#48228,#48229,#48230,#48231,#48232,#48233,
#48234,#48235,#48236,#48237,#48238,#48239,#48240,#48241,#48242,#48243,#48244,
#48245,#48246,#48247,#48248,#48249,#48250,#48251,#48252,#48253,#48254,#48255,
#48256,#48257,#48258,#48259,#48260,#48261,#48262,#48263,#48264,#48265,#48266,
#48267,#48268,#48269,#48270,#48271,#48272,#48273,#48274,#48275,#48276,#48277,
#48278,#48279,#48280,#48281,#48282,#48283,#48284,#48285,#48286,#48287,#48288,
#48289,#48290,#48291,#48292,#48293,#48294,#48295,#48296,#48297,#48298,#48299,
#48300,#48301,#48302,#48303,#48304,#48305,#48306,#48307,#48308,#48309,#48310,
#48311,#48312,#48313,#48314,#48315,#48316,#48317,#48318,#48319,#48320,#48321,
#48322,#48323,#48324,#48325,#48326,#48327,#48328,#48329,#48330,#48331,#48332,
#48333,#48334,#48335,#48336,#48337,#48338,#48339,#48340,#48341,#48342,#48343,
#48344,#48345,#48346,#48347,#48348,#48349,#48350,#48351,#48352,#48353,#48354,
#48355,#48356,#48357,#48358,#48359,#48360,#48361,#48362,#48363,#48364,#48365,
#48366,#48367,#48368,#48369,#48370,#48371,#48372,#48373,#48374,#48375,#48376,
#48377,#48378,#48379,#48380,#48381,#48382,#48383,#48384,#48385,#48386,#48387,
#48388,#48389,#48390,#48391,#48392,#48393,#48394,#48395,#48396,#48397,#48398,
#48399,#48400,#48401,#48402,#48403,#48404,#48405,#48406,#48407,#48408,#48409,
#48410,#48411,#48412,#48413,#48414,#48415,#48416,#48417,#48418,#48419,#48420,
#48421,#48422,#48423,#48424,#48425,#48426,#48427,#48428,#48429,#48430,#48431,
#48432,#48433,#48434,#48435,#48436,#48437,#48438,#48439,#48440,#48441,#48442,
#48443,#48444,#48445,#48446,#48447,#48448,#48449,#48450,#48451,#48452,#48453,
#48454,#48455,#48456,#48457,#48458,#48459,#48460,#48461,#48462,#48463,#48464,
#48465,#48466,#48467,#48468,#48469,#48470,#48471,#48472,#48473,#48474,#48475,
#48476,#48477,#48478,#48479,#48480,#48481,#48482,#48483,#48484,#48485,#48486,
#48487,#48488,#48489,#48490,#48491,#48492,#48493,#48494,#48495,#48496,#48497,
#48498,#48499,#48500,#48501,#48502,#48503,#48504,#48505,#48506,#48507,#48508,
#48509,#48510,#48511,#48512,#48513,#48514,#48515,#48516,#48517,#48518,#48519,
#48520,#48521,#48522,#48523,#48524,#48525,#48526,#48527,#48528,#48529,#48530,
#48531,#48532,#48533,#48534,#48535,#48536,#48537,#48538,#48539,#48540,#48541,
#48542,#48543,#48544,#48545,#48546,#48547,#48548,#48549,#48550,#48551,#48552,
#48553,#48554,#48555,#48556,#48557,#48558,#48559,#48560,#48561,#48562,#48563,
#48564,#48565,#48566,#48567,#48568,#48569,#48570,#48571,#48572,#48573,#48574,
#48575,#48576,#48577,#48578,#48579,#48580,#48581,#48582,#48583,#48584,#48585,
#48586,#48587,#48588,#48589,#48590,#48591,#48592,#48593,#48594,#48595,#48596,
#48597,#48598,#48599,#48600,#48601,#48602,#48603,#48604,#48605,#48606,#48607,
#48608,#48609,#48610,#48611,#48612,#48613,#48614,#48615,#48616,#48617,#48618,
#48619,#48620,#48621,#48622,#48623,#48624,#48625,#48626,#48627,#48628,#48629,
#48630,#48631,#48632,#48633,#48634,#48635,#48636,#48637,#48638,#48639,#48640,
#48641,#48642,#48643,#48644,#48645,#48646,#48647,#48648,#48649,#48650,#48651,
#48652,#48653,#48654,#48655,#48656,#48657,#48658,#48659,#48660,#48661,#48662,
#48663,#48664,#48665,#48666,#48667,#48668,#48669,#48670,#48671,#48672,#48673,
#48674,#48675,#48676),.UNSPECIFIED.,.F.,.F.,(4,3,3,3,3,3,3,3,3,3,3,3,3,
3,3,3,3,3,3,3,3,3,3,3,3,3,3,3,3,3,3,3,3,3,3,3,3,3,3,3,3,3,3,3,3,3,3,3,3,
3,3,3,3,3,3,3,3,3,3,3,3,3,3,3,3,3,3,3,3,3,3,3,3,3,3,3,3,3,3,3,3,3,3,3,3,
3,3,3,3,3,3,3,3,3,3,3,3,3,3,3,3,3,3,3,3,3,3,3,3,3,3,3,3,3,3,3,3,3,3,3,3,
3,3,3,3,3,3,3,3,3,3,3,3,3,3,3,3,3,3,3,3,3,3,3,3,3,3,3,3,3,3,3,3,3,3,3,3,
3,3,3,3,3,3,3,3,3,3,3,3,3,3,3,3,3,3,3,3,3,3,3,3,3,3,3,3,3,3,3,3,3,3,3,3,
3,3,3,3,3,3,3,3,3,3,3,4),(0.,0.006896551724138,0.0124999836137735,0.01379310344828,
0.02068965517241,0.02758620689655,0.0287500147726293,0.03448275862069,0.04137931034483,
0.0449999960540111,0.04827586206897,0.0551724137931,0.061249990576592,0.06206896551724,
0.06896551724138,0.07586206896552,0.077500020146031,0.08275862068966,0.08965517241379,
0.0937499863389159,0.09655172413793,0.1034482758621,0.109999997295967,0.1103448275862,
0.1172413793103,0.1241379310345,0.126250021167858,0.1310344827586,0.1379310344828,
0.142499980080653,0.1448275862069,0.151724137931,0.1586206896552,0.15875000071435,
0.1655172413793,0.1724137931034,0.175000017053664,0.1793103448276,0.1862068965517,
0.191249978763952,0.1931034482759,0.2,0.2068965517241,0.207500006105622,
0.2137931034483,0.2206896551724,0.223750008641754,0.2275862068966,0.2344827586207,
0.239999982367649,0.2413793103448,0.248275862069,0.2551724137931,0.256250013484739,
0.2620689655172,0.2689655172414,0.272499998025252,0.2758620689655,0.2827586206897,
0.288749989207176,0.2896551724138,0.2965517241379,0.3034482758621,0.305000019440357,
0.3103448275862,0.3172413793103,0.321249987913624,0.3241379310345,0.3310344827586,
0.337499996263584,0.3379310344828,0.3448275862069,0.351724137931,0.353750021363705,
0.3586206896552,0.3655172413793,0.369999980876542,0.3724137931034,0.3793103448276,
0.3862068965517,0.3931034482759,0.4,0.402500018165757,0.4068965517241,0.4137931034483,
0.418749978614374,0.4206896551724,0.4275862068966,0.4344827586207,0.435000004876983,
0.4413793103448,0.448275862069,0.451250010408905,0.4551724137931,0.4620689655172,
0.467499981401136,0.4689655172414,0.4758620689655,0.4827586206897,0.483750012153467,
0.4896551724138,0.4965517241379,0.5,0.5034482758621,0.5103448275862,0.516249987846536,
0.5172413793103,0.5241379310345,0.5310344827586,0.532500018598866,0.5379310344828,
0.5448275862069,0.548749989591093,0.551724137931,0.5586206896552,0.564999995123015,
0.5655172413793,0.5724137931034,0.5793103448276,0.581250021385624,0.5862068965517,
0.5931034482759,0.597499981834247,0.6,0.6068965517241,0.6137931034483,0.6206896551724,
0.6275862068966,0.63000001912345,0.6344827586207,0.6413793103448,0.646249978636288,
0.648275862069,0.6551724137931,0.6620689655172,0.662500003736417,0.6689655172414,
0.6758620689655,0.678750012086376,0.6827586206897,0.6896551724138,0.694999980559646,
0.6965517241379,0.7034482758621,0.7103448275862,0.711250010792826,0.7172413793103,
0.7241379310345,0.727500001974747,0.7310344827586,0.7379310344828,0.74374998651526,
0.7448275862069,0.751724137931,0.7586206896552,0.760000017632353,0.7655172413793,
0.7724137931034,0.776249991358242,0.7793103448276,0.7862068965517,0.792499993894378,
0.7931034482759,0.8,0.8068965517241,0.808750021236051,0.8137931034483,0.8206896551724,
0.824999982946336,0.8275862068966,0.8344827586207,0.841249999285647,0.8413793103448,
0.848275862069,0.8551724137931,0.857500019919344,0.8620689655172,0.8689655172414,
0.873749978832139,0.8758620689655,0.8827586206897,0.8896551724138,0.890000002704037,
0.8965517241379,0.9034482758621,0.906250013661088,0.9103448275862,0.9172413793103,
0.922499979853961,0.9241379310345,0.9310344827586,0.9379310344828,0.938750009423416,
0.9448275862069,0.951724137931,0.955000003945986,0.9586206896552,0.9655172413793,
0.971249985227364,0.9724137931034,0.9793103448276,0.9862068965517,0.987500016386232,
0.9931034482759,0.999999999674344),.UNSPECIFIED.);
#2456=B_SPLINE_CURVE_WITH_KNOTS('',3,(#48947,#48948,#48949,#48950,#48951,
#48952,#48953,#48954,#48955,#48956,#48957,#48958,#48959,#48960,#48961,#48962,
#48963,#48964,#48965,#48966,#48967,#48968,#48969,#48970,#48971,#48972,#48973,
#48974,#48975,#48976,#48977,#48978,#48979,#48980,#48981,#48982,#48983,#48984,
#48985,#48986,#48987,#48988,#48989,#48990,#48991,#48992,#48993,#48994,#48995,
#48996,#48997,#48998,#48999,#49000,#49001,#49002,#49003,#49004,#49005,#49006,
#49007,#49008,#49009,#49010),.UNSPECIFIED.,.F.,.F.,(4,2,2,2,2,2,2,2,2,2,
2,2,2,2,2,2,2,2,2,2,2,2,2,2,2,2,2,2,2,2,2,4),(-1.66633732000905,-1.59703627011939,
-1.52852012575264,-1.48286496355783,-1.4338739966197,-1.40938609426276,
-1.36138358442955,-1.31255473680488,-1.26336425821289,-1.21403314958031,
-1.1641700898921,-1.06400329438633,-1.0149699430902,-0.965942177532495,
-0.917273319565972,-0.869153345373983,-0.844143351275243,-0.794731617877203,
-0.745484131964617,-0.644804715310458,-0.594705472366083,-0.545267901785368,
-0.496092822607313,-0.44725089796995,-0.398871422897544,-0.374356052946474,
-0.326915236742278,-0.277301516825421,-0.227751301391206,-0.128642088715264,
-0.0642903176182427,-1.08468575917311E-5),.UNSPECIFIED.);
#2457=B_SPLINE_CURVE_WITH_KNOTS('',3,(#49012,#49013,#49014,#49015,#49016,
#49017,#49018,#49019,#49020,#49021,#49022,#49023,#49024,#49025,#49026,#49027,
#49028,#49029,#49030,#49031,#49032,#49033,#49034,#49035,#49036,#49037,#49038,
#49039,#49040,#49041,#49042,#49043,#49044,#49045,#49046,#49047,#49048,#49049,
#49050,#49051,#49052,#49053,#49054,#49055,#49056,#49057,#49058,#49059,#49060,
#49061,#49062,#49063,#49064,#49065,#49066,#49067,#49068,#49069,#49070,#49071,
#49072,#49073,#49074,#49075,#49076,#49077,#49078,#49079,#49080,#49081,#49082,
#49083,#49084,#49085,#49086,#49087,#49088,#49089,#49090,#49091,#49092,#49093,
#49094,#49095,#49096,#49097,#49098,#49099,#49100,#49101,#49102,#49103,#49104,
#49105,#49106,#49107,#49108,#49109,#49110,#49111,#49112,#49113,#49114,#49115,
#49116,#49117,#49118,#49119,#49120,#49121,#49122,#49123,#49124,#49125,#49126,
#49127,#49128,#49129,#49130,#49131,#49132,#49133,#49134,#49135,#49136,#49137,
#49138,#49139,#49140,#49141,#49142,#49143,#49144,#49145,#49146,#49147,#49148,
#49149,#49150,#49151,#49152,#49153,#49154,#49155,#49156,#49157,#49158,#49159,
#49160,#49161,#49162,#49163,#49164,#49165,#49166,#49167,#49168,#49169,#49170,
#49171,#49172,#49173,#49174,#49175,#49176,#49177,#49178,#49179,#49180,#49181,
#49182,#49183,#49184,#49185,#49186,#49187,#49188,#49189,#49190,#49191,#49192,
#49193,#49194,#49195,#49196,#49197,#49198,#49199,#49200,#49201,#49202,#49203,
#49204,#49205,#49206,#49207,#49208,#49209,#49210,#49211,#49212,#49213,#49214,
#49215,#49216,#49217,#49218,#49219,#49220,#49221,#49222,#49223,#49224,#49225,
#49226,#49227,#49228,#49229,#49230,#49231,#49232,#49233,#49234,#49235,#49236,
#49237,#49238,#49239,#49240,#49241,#49242,#49243,#49244,#49245,#49246,#49247,
#49248,#49249,#49250,#49251,#49252,#49253,#49254,#49255,#49256,#49257,#49258,
#49259,#49260,#49261,#49262,#49263,#49264,#49265,#49266,#49267,#49268,#49269,
#49270,#49271,#49272,#49273,#49274,#49275,#49276,#49277,#49278,#49279,#49280,
#49281,#49282,#49283,#49284,#49285,#49286,#49287,#49288,#49289,#49290,#49291,
#49292,#49293,#49294,#49295,#49296,#49297,#49298,#49299,#49300,#49301,#49302,
#49303,#49304,#49305,#49306,#49307,#49308,#49309,#49310,#49311,#49312,#49313,
#49314,#49315,#49316,#49317,#49318,#49319,#49320,#49321,#49322,#49323,#49324,
#49325,#49326,#49327,#49328,#49329,#49330,#49331,#49332,#49333,#49334,#49335,
#49336,#49337,#49338,#49339,#49340,#49341,#49342,#49343,#49344,#49345,#49346,
#49347,#49348,#49349,#49350,#49351,#49352,#49353,#49354,#49355,#49356,#49357,
#49358,#49359,#49360,#49361,#49362,#49363,#49364,#49365,#49366,#49367,#49368,
#49369,#49370,#49371,#49372,#49373,#49374,#49375,#49376,#49377,#49378,#49379,
#49380,#49381,#49382,#49383,#49384,#49385,#49386,#49387,#49388,#49389,#49390,
#49391,#49392,#49393,#49394,#49395,#49396,#49397,#49398,#49399,#49400,#49401,
#49402,#49403,#49404,#49405,#49406,#49407,#49408,#49409,#49410,#49411,#49412,
#49413,#49414,#49415,#49416,#49417,#49418,#49419,#49420,#49421,#49422,#49423,
#49424,#49425,#49426,#49427,#49428,#49429,#49430,#49431,#49432,#49433,#49434,
#49435,#49436,#49437,#49438,#49439,#49440,#49441,#49442,#49443,#49444,#49445,
#49446,#49447,#49448,#49449,#49450,#49451,#49452,#49453,#49454,#49455,#49456,
#49457,#49458,#49459,#49460,#49461,#49462,#49463,#49464,#49465,#49466,#49467,
#49468,#49469,#49470,#49471,#49472,#49473,#49474,#49475,#49476,#49477,#49478,
#49479,#49480,#49481,#49482,#49483,#49484,#49485,#49486,#49487,#49488,#49489,
#49490,#49491,#49492,#49493,#49494,#49495,#49496,#49497,#49498,#49499,#49500,
#49501,#49502,#49503,#49504,#49505,#49506,#49507,#49508,#49509,#49510,#49511,
#49512,#49513,#49514,#49515,#49516,#49517,#49518,#49519,#49520,#49521,#49522,
#49523,#49524,#49525,#49526,#49527,#49528,#49529,#49530,#49531,#49532,#49533,
#49534,#49535,#49536,#49537,#49538,#49539,#49540,#49541,#49542,#49543,#49544,
#49545,#49546,#49547,#49548,#49549,#49550,#49551,#49552,#49553,#49554,#49555,
#49556,#49557,#49558,#49559,#49560,#49561,#49562,#49563,#49564,#49565,#49566,
#49567,#49568,#49569,#49570,#49571,#49572,#49573,#49574,#49575,#49576,#49577,
#49578,#49579,#49580,#49581,#49582,#49583,#49584,#49585,#49586,#49587,#49588,
#49589,#49590,#49591,#49592,#49593,#49594,#49595,#49596,#49597,#49598,#49599,
#49600,#49601,#49602,#49603,#49604,#49605,#49606,#49607,#49608,#49609,#49610,
#49611,#49612,#49613,#49614,#49615,#49616,#49617,#49618,#49619,#49620,#49621,
#49622,#49623,#49624),.UNSPECIFIED.,.F.,.F.,(4,3,3,3,3,3,3,3,3,3,3,3,3,
3,3,3,3,3,3,3,3,3,3,3,3,3,3,3,3,3,3,3,3,3,3,3,3,3,3,3,3,3,3,3,3,3,3,3,3,
3,3,3,3,3,3,3,3,3,3,3,3,3,3,3,3,3,3,3,3,3,3,3,3,3,3,3,3,3,3,3,3,3,3,3,3,
3,3,3,3,3,3,3,3,3,3,3,3,3,3,3,3,3,3,3,3,3,3,3,3,3,3,3,3,3,3,3,3,3,3,3,3,
3,3,3,3,3,3,3,3,3,3,3,3,3,3,3,3,3,3,3,3,3,3,3,3,3,3,3,3,3,3,3,3,3,3,3,3,
3,3,3,3,3,3,3,3,3,3,3,3,3,3,3,3,3,3,3,3,3,3,3,3,3,3,3,3,3,3,3,3,3,3,3,3,
3,3,3,3,3,3,3,3,3,3,3,4),(0.,0.006896551724138,0.0124999836137735,0.01379310344828,
0.02068965517241,0.02758620689655,0.0287500147726293,0.03448275862069,0.04137931034483,
0.0449999960540111,0.04827586206897,0.0551724137931,0.061249990576592,0.06206896551724,
0.06896551724138,0.07586206896552,0.077500020146031,0.08275862068966,0.08965517241379,
0.0937499863389159,0.09655172413793,0.1034482758621,0.109999997295967,0.1103448275862,
0.1172413793103,0.1241379310345,0.126250021167858,0.1310344827586,0.1379310344828,
0.142499980080653,0.1448275862069,0.151724137931,0.1586206896552,0.15875000071435,
0.1655172413793,0.1724137931034,0.175000017053664,0.1793103448276,0.1862068965517,
0.191249978763952,0.1931034482759,0.2,0.2068965517241,0.207500006105622,
0.2137931034483,0.2206896551724,0.223750008641754,0.2275862068966,0.2344827586207,
0.239999982367649,0.2413793103448,0.248275862069,0.2551724137931,0.256250013484739,
0.2620689655172,0.2689655172414,0.272499998025252,0.2758620689655,0.2827586206897,
0.288749989207176,0.2896551724138,0.2965517241379,0.3034482758621,0.305000019440357,
0.3103448275862,0.3172413793103,0.321249987913624,0.3241379310345,0.3310344827586,
0.337499996263584,0.3379310344828,0.3448275862069,0.351724137931,0.353750021363705,
0.3586206896552,0.3655172413793,0.369999980876542,0.3724137931034,0.3793103448276,
0.3862068965517,0.3931034482759,0.4,0.40250001816575,0.4068965517241,0.4137931034483,
0.418749978614372,0.4206896551724,0.4275862068966,0.4344827586207,0.435000004876983,
0.4413793103448,0.448275862069,0.451250010408905,0.4551724137931,0.4620689655172,
0.467499981401136,0.4689655172414,0.4758620689655,0.4827586206897,0.483750012153467,
0.4896551724138,0.4965517241379,0.5,0.5034482758621,0.5103448275862,0.516249987846536,
0.5172413793103,0.5241379310345,0.5310344827586,0.532500018598866,0.5379310344828,
0.5448275862069,0.548749989591093,0.551724137931,0.5586206896552,0.564999995123015,
0.5655172413793,0.5724137931034,0.5793103448276,0.581250021385624,0.5862068965517,
0.5931034482759,0.597499981834247,0.6,0.6068965517241,0.6137931034483,0.6206896551724,
0.6275862068966,0.63000001912345,0.6344827586207,0.6413793103448,0.646249978636288,
0.648275862069,0.6551724137931,0.6620689655172,0.662500003736417,0.6689655172414,
0.6758620689655,0.678750012086376,0.6827586206897,0.6896551724138,0.694999980559646,
0.6965517241379,0.7034482758621,0.7103448275862,0.711250010792826,0.7172413793103,
0.7241379310345,0.727500001974747,0.7310344827586,0.7379310344828,0.74374998651526,
0.7448275862069,0.751724137931,0.7586206896552,0.760000017632353,0.7655172413793,
0.7724137931034,0.776249991358242,0.7793103448276,0.7862068965517,0.792499993894378,
0.7931034482759,0.8,0.8068965517241,0.808750021236051,0.8137931034483,0.8206896551724,
0.824999982946336,0.8275862068966,0.8344827586207,0.841249999285647,0.8413793103448,
0.848275862069,0.8551724137931,0.857500019919344,0.8620689655172,0.8689655172414,
0.873749978832139,0.8758620689655,0.8827586206897,0.8896551724138,0.890000002704037,
0.8965517241379,0.9034482758621,0.906250013661088,0.9103448275862,0.9172413793103,
0.922499979853961,0.9241379310345,0.9310344827586,0.9379310344828,0.938750009423416,
0.9448275862069,0.951724137931,0.955000003945986,0.9586206896552,0.9655172413793,
0.971249985227364,0.9724137931034,0.9793103448276,0.9862068965517,0.987500016386232,
0.9931034482759,0.999999999699303),.UNSPECIFIED.);
#2458=B_SPLINE_CURVE_WITH_KNOTS('',3,(#49894,#49895,#49896,#49897,#49898,
#49899,#49900,#49901,#49902,#49903,#49904,#49905,#49906,#49907,#49908,#49909,
#49910,#49911,#49912,#49913,#49914,#49915,#49916,#49917,#49918,#49919,#49920,
#49921,#49922,#49923,#49924,#49925,#49926,#49927,#49928,#49929,#49930,#49931,
#49932,#49933,#49934,#49935,#49936,#49937,#49938,#49939,#49940,#49941,#49942,
#49943,#49944,#49945,#49946,#49947,#49948,#49949,#49950,#49951,#49952,#49953,
#49954,#49955,#49956,#49957,#49958,#49959,#49960,#49961,#49962,#49963,#49964,
#49965,#49966,#49967,#49968,#49969,#49970,#49971,#49972,#49973,#49974,#49975,
#49976,#49977,#49978,#49979,#49980,#49981,#49982,#49983,#49984,#49985,#49986,
#49987,#49988,#49989,#49990,#49991,#49992,#49993,#49994,#49995,#49996,#49997,
#49998,#49999,#50000,#50001,#50002,#50003,#50004,#50005,#50006,#50007,#50008,
#50009,#50010,#50011,#50012,#50013,#50014,#50015,#50016,#50017,#50018,#50019,
#50020,#50021,#50022,#50023,#50024,#50025,#50026,#50027,#50028,#50029,#50030,
#50031,#50032,#50033,#50034,#50035,#50036,#50037,#50038,#50039,#50040,#50041,
#50042,#50043,#50044,#50045,#50046,#50047,#50048,#50049,#50050,#50051,#50052,
#50053,#50054,#50055,#50056,#50057,#50058,#50059,#50060,#50061,#50062,#50063,
#50064,#50065,#50066,#50067,#50068,#50069,#50070,#50071,#50072,#50073,#50074,
#50075,#50076,#50077,#50078,#50079,#50080,#50081,#50082,#50083),
 .UNSPECIFIED.,.F.,.F.,(4,2,2,2,2,2,2,2,2,2,2,2,2,2,2,2,2,2,2,2,2,2,2,2,
2,2,2,2,2,2,2,2,2,2,2,2,2,2,2,2,2,2,2,2,2,2,2,2,2,2,2,2,2,2,2,2,2,2,2,2,
2,2,2,2,2,2,2,2,2,2,2,2,2,2,2,2,2,2,2,2,2,2,2,2,2,2,2,2,2,2,2,2,2,2,4),
(-12.5010893468563,-12.3955019246696,-12.29254455623,-12.1459237162089,
-12.0534009089294,-11.9236776502422,-11.7491077006647,-11.6772399648329,
-11.5712782716806,-11.3238756382021,-11.2051337123826,-11.1056993724438,
-11.0021239973504,-10.7378793159625,-10.5155966870519,-10.3512039322814,
-10.1466748655266,-9.87142699075404,-9.73709147703406,-9.53389602132558,
-9.31814598815267,-9.17117893543063,-9.01109017484306,-8.80905691073069,
-8.41805541817743,-8.12716271658195,-8.00669735542938,-7.8039680852172,
-7.53375845441259,-7.40232630908509,-7.27541859109228,-7.1062648398012,
-6.96164817241986,-6.79904573142915,-6.69501805425453,-6.51076918321285,
-6.23766454972543,-6.05716403248301,-5.87761455247391,-5.653672802988,-5.51404475617032,
-5.26873717693825,-5.05382167631166,-4.90073408060745,-4.81137902932328,
-4.51359899975272,-4.42504630749999,-4.34128325511,-4.25738441999853,-4.11551925816328,
-3.92192946120956,-3.72812417494571,-3.61710817639108,-3.40662038260933,
-3.16125849456072,-2.99827957516932,-2.84630234994494,-2.63994642266069,
-2.51541401577412,-2.4373640545864,-2.27085778902812,-2.18206961488083,
-2.10754515662402,-1.99262515056807,-1.85155851909128,-1.77732091277462,
-1.71535701253962,-1.6526902916784,-1.562493505486,-1.50083657181577,-1.46545499373709,
-1.40994218479656,-1.359563114224,-1.29488296358145,-1.26302820187884,-1.21758580791865,
-1.15676382139674,-1.07603643283981,-1.03198768531833,-0.973241214322041,
-0.90395132170858,-0.837813892070961,-0.769710721948455,-0.724142155412939,
-0.67612082666296,-0.625966063761364,-0.560562807638131,-0.497620494482934,
-0.4468543143013,-0.355950889046661,-0.292569617992569,-0.241516995465503,
-0.166846284360261,-0.0399205669991334,-5.63539519875474E-5),
 .UNSPECIFIED.);
#2459=B_SPLINE_CURVE_WITH_KNOTS('',3,(#50084,#50085,#50086,#50087,#50088,
#50089,#50090,#50091,#50092,#50093,#50094,#50095,#50096,#50097,#50098,#50099,
#50100,#50101,#50102,#50103,#50104,#50105,#50106,#50107,#50108,#50109,#50110,
#50111,#50112,#50113,#50114,#50115,#50116,#50117,#50118,#50119,#50120,#50121,
#50122,#50123,#50124,#50125,#50126,#50127,#50128,#50129,#50130,#50131,#50132,
#50133,#50134,#50135,#50136,#50137,#50138,#50139,#50140,#50141,#50142,#50143,
#50144,#50145,#50146,#50147,#50148,#50149,#50150,#50151,#50152,#50153,#50154,
#50155,#50156,#50157,#50158,#50159,#50160,#50161,#50162,#50163,#50164,#50165,
#50166,#50167,#50168,#50169,#50170,#50171,#50172,#50173,#50174,#50175,#50176,
#50177,#50178,#50179,#50180,#50181,#50182,#50183,#50184,#50185,#50186,#50187),
 .UNSPECIFIED.,.F.,.F.,(4,2,2,2,2,2,2,2,2,2,2,2,2,2,2,2,2,2,2,2,2,2,2,2,
2,2,2,2,2,2,2,2,2,2,2,2,2,2,2,2,2,2,2,2,2,2,2,2,2,2,2,4),(-5.72457039602614,
-5.67740959373671,-5.63122585579928,-5.55949891583999,-5.51613971115158,
-5.47294026658525,-5.38759086497003,-5.34869162708517,-5.30945877254513,
-5.22227376857796,-5.16149754031448,-5.11547880467284,-5.06672492745363,
-4.9564919053269,-4.89278834378409,-4.82903674184974,-4.69584725936334,
-4.63115794223737,-4.56625122927357,-4.42357125813279,-4.34725616502263,
-4.26987365048767,-4.1158488390985,-4.03705650559149,-3.9049361991664,-3.8267107788816,
-3.74890540080541,-3.56871767260129,-3.48072229414968,-3.257626156076,-3.12571880576179,
-2.99213032376785,-2.75262686455332,-2.64193775641107,-2.53021199520972,
-2.31081713723528,-2.19937460680053,-1.98583275220802,-1.76266385660368,
-1.65123683467011,-1.43290388293514,-1.32316089943354,-1.21496827736271,
-0.993191000517704,-0.883789162915291,-0.774073723773991,-0.561001501856556,
-0.453917196237877,-0.353256981724687,-0.17227205692989,-0.0868655698498306,
-3.32283829430584E-6),.UNSPECIFIED.);
#2460=B_SPLINE_CURVE_WITH_KNOTS('',3,(#50328,#50329,#50330,#50331,#50332,
#50333,#50334,#50335,#50336,#50337,#50338,#50339,#50340,#50341,#50342,#50343,
#50344,#50345,#50346,#50347,#50348,#50349,#50350,#50351,#50352,#50353,#50354,
#50355,#50356,#50357,#50358,#50359,#50360,#50361,#50362,#50363,#50364,#50365,
#50366,#50367,#50368,#50369,#50370,#50371,#50372,#50373,#50374,#50375,#50376,
#50377,#50378,#50379,#50380,#50381,#50382,#50383,#50384,#50385,#50386,#50387,
#50388,#50389,#50390,#50391,#50392,#50393,#50394,#50395,#50396,#50397,#50398,
#50399,#50400,#50401,#50402,#50403,#50404,#50405,#50406,#50407,#50408,#50409,
#50410,#50411,#50412,#50413,#50414,#50415,#50416,#50417,#50418,#50419,#50420,
#50421,#50422,#50423,#50424,#50425,#50426,#50427,#50428,#50429,#50430,#50431,
#50432,#50433,#50434,#50435,#50436,#50437,#50438,#50439,#50440,#50441,#50442,
#50443,#50444,#50445,#50446,#50447,#50448,#50449,#50450,#50451,#50452,#50453,
#50454,#50455,#50456,#50457,#50458,#50459,#50460,#50461,#50462,#50463,#50464,
#50465,#50466,#50467,#50468,#50469,#50470,#50471,#50472,#50473,#50474,#50475,
#50476,#50477,#50478,#50479,#50480,#50481,#50482,#50483,#50484,#50485,#50486,
#50487,#50488,#50489,#50490,#50491,#50492,#50493,#50494,#50495,#50496,#50497,
#50498,#50499),.UNSPECIFIED.,.F.,.F.,(4,2,2,2,2,2,2,2,2,2,2,2,2,2,2,2,2,
2,2,2,2,2,2,2,2,2,2,2,2,2,2,2,2,2,2,2,2,2,2,2,2,2,2,2,2,2,2,2,2,2,2,2,2,
2,2,2,2,2,2,2,2,2,2,2,2,2,2,2,2,2,2,2,2,2,2,2,2,2,2,2,2,2,2,2,2,4),(0.000470698768311942,
0.148321453566357,0.317425857543853,0.436101923702642,0.557844942473512,
0.744678636579374,0.855687791842655,0.9076686119342,0.983660372768557,1.0725845720498,
1.12117238638503,1.2178861382758,1.27910492119424,1.31465770016191,1.34870198596797,
1.41444082490198,1.45852650913111,1.53071781722442,1.56634174180461,1.6216854737005,
1.66350990999233,1.72858009368055,1.77623273819062,1.83294115633519,1.87503221650589,
1.95031796433434,2.02516118191607,2.09873098639522,2.17430958552449,2.23710534751301,
2.29662438387701,2.44410295517342,2.6462228959603,2.89691576438539,3.0543071171469,
3.20520804542532,3.34590083749761,3.53109280663704,3.66876538880978,3.74839244187486,
3.89972766502862,4.03103446017813,4.10749792180876,4.23142124648352,4.31252932960002,
4.46142079174021,4.54933535333564,4.6710448490143,4.74136792982459,4.89446451461515,
5.00598172369279,5.12745759051139,5.20868840672564,5.33920348711798,5.58984772231306,
5.71210658233482,5.88394566206482,6.19877568160708,6.45985913569223,6.67667688005281,
6.77822327741072,6.87703056315368,6.98871985461782,7.0873938977894,7.16085653401938,
7.32786847784497,7.41628138031729,7.47331330577707,7.54654259779913,7.62125918027395,
7.68880174806676,7.764248864466,7.82221895060197,7.91842932475137,7.98331302303493,
8.07813386136645,8.12849570087089,8.18024002119065,8.26551377880065,8.41891269762442,
8.49837485663615,8.58182636321036,8.69126476283946,8.80338860033424,8.95484442293788,
9.18218359913891),.UNSPECIFIED.);
#2461=B_SPLINE_CURVE_WITH_KNOTS('',3,(#51178,#51179,#51180,#51181,#51182,
#51183,#51184,#51185,#51186,#51187,#51188,#51189,#51190,#51191,#51192,#51193,
#51194,#51195,#51196,#51197,#51198,#51199,#51200,#51201,#51202,#51203,#51204,
#51205,#51206,#51207,#51208,#51209,#51210,#51211,#51212,#51213,#51214,#51215,
#51216,#51217,#51218,#51219,#51220,#51221,#51222,#51223,#51224,#51225,#51226,
#51227,#51228,#51229,#51230,#51231,#51232,#51233,#51234,#51235,#51236,#51237,
#51238,#51239,#51240,#51241,#51242,#51243,#51244,#51245,#51246,#51247,#51248,
#51249,#51250,#51251,#51252,#51253,#51254,#51255,#51256,#51257,#51258,#51259,
#51260,#51261,#51262,#51263,#51264,#51265,#51266,#51267,#51268,#51269,#51270,
#51271,#51272,#51273,#51274,#51275,#51276,#51277,#51278,#51279,#51280,#51281,
#51282,#51283,#51284,#51285,#51286,#51287,#51288,#51289,#51290,#51291,#51292,
#51293,#51294,#51295,#51296,#51297,#51298,#51299,#51300,#51301,#51302,#51303,
#51304,#51305,#51306,#51307,#51308,#51309,#51310,#51311,#51312,#51313,#51314,
#51315,#51316,#51317,#51318,#51319,#51320,#51321,#51322,#51323,#51324,#51325,
#51326,#51327,#51328,#51329,#51330,#51331,#51332,#51333,#51334,#51335,#51336,
#51337,#51338,#51339,#51340,#51341,#51342,#51343,#51344,#51345,#51346,#51347,
#51348,#51349,#51350,#51351,#51352,#51353,#51354,#51355,#51356,#51357,#51358,
#51359,#51360,#51361,#51362,#51363,#51364,#51365,#51366,#51367,#51368,#51369,
#51370,#51371,#51372,#51373,#51374,#51375,#51376,#51377,#51378,#51379,#51380,
#51381,#51382,#51383,#51384,#51385,#51386,#51387,#51388,#51389,#51390,#51391,
#51392,#51393,#51394,#51395,#51396,#51397,#51398,#51399,#51400,#51401,#51402,
#51403,#51404,#51405,#51406,#51407,#51408,#51409,#51410,#51411,#51412,#51413,
#51414,#51415,#51416,#51417,#51418,#51419,#51420,#51421,#51422,#51423,#51424,
#51425,#51426,#51427,#51428,#51429,#51430,#51431,#51432,#51433,#51434,#51435,
#51436,#51437,#51438,#51439,#51440,#51441,#51442,#51443,#51444,#51445,#51446,
#51447,#51448,#51449,#51450,#51451,#51452,#51453,#51454,#51455,#51456,#51457,
#51458,#51459,#51460,#51461,#51462,#51463,#51464,#51465,#51466,#51467,#51468,
#51469,#51470,#51471,#51472,#51473,#51474,#51475,#51476,#51477,#51478,#51479,
#51480,#51481,#51482,#51483,#51484,#51485,#51486,#51487,#51488,#51489,#51490,
#51491,#51492,#51493,#51494,#51495,#51496,#51497,#51498,#51499,#51500,#51501,
#51502,#51503,#51504,#51505,#51506,#51507,#51508,#51509,#51510,#51511,#51512,
#51513,#51514,#51515,#51516,#51517,#51518,#51519,#51520,#51521,#51522,#51523,
#51524,#51525,#51526,#51527,#51528,#51529,#51530,#51531,#51532,#51533,#51534,
#51535,#51536,#51537,#51538,#51539,#51540,#51541,#51542,#51543,#51544,#51545,
#51546,#51547,#51548,#51549,#51550,#51551,#51552,#51553,#51554,#51555,#51556,
#51557,#51558,#51559,#51560,#51561,#51562,#51563,#51564,#51565,#51566,#51567,
#51568,#51569,#51570,#51571,#51572,#51573,#51574,#51575,#51576,#51577,#51578,
#51579,#51580,#51581,#51582,#51583,#51584,#51585,#51586,#51587,#51588,#51589,
#51590,#51591,#51592,#51593,#51594,#51595,#51596,#51597,#51598,#51599,#51600,
#51601,#51602,#51603,#51604,#51605,#51606,#51607,#51608,#51609,#51610,#51611,
#51612,#51613,#51614,#51615,#51616,#51617,#51618,#51619,#51620,#51621,#51622,
#51623,#51624,#51625,#51626,#51627,#51628,#51629,#51630,#51631,#51632,#51633,
#51634,#51635,#51636,#51637,#51638,#51639,#51640,#51641,#51642,#51643,#51644,
#51645,#51646,#51647,#51648,#51649,#51650,#51651,#51652,#51653,#51654,#51655,
#51656,#51657,#51658,#51659,#51660,#51661,#51662,#51663,#51664,#51665,#51666,
#51667,#51668,#51669,#51670,#51671,#51672,#51673,#51674,#51675,#51676,#51677,
#51678,#51679,#51680,#51681,#51682,#51683,#51684,#51685,#51686,#51687,#51688,
#51689,#51690,#51691,#51692,#51693,#51694,#51695,#51696,#51697,#51698,#51699,
#51700,#51701,#51702,#51703,#51704,#51705,#51706,#51707,#51708,#51709,#51710,
#51711,#51712,#51713,#51714,#51715,#51716,#51717,#51718,#51719,#51720,#51721,
#51722,#51723,#51724,#51725,#51726,#51727,#51728,#51729,#51730,#51731,#51732,
#51733,#51734,#51735,#51736,#51737,#51738,#51739,#51740,#51741,#51742,#51743,
#51744,#51745,#51746,#51747,#51748,#51749,#51750,#51751,#51752,#51753,#51754,
#51755,#51756,#51757,#51758,#51759,#51760,#51761,#51762,#51763,#51764,#51765,
#51766,#51767,#51768,#51769,#51770,#51771,#51772,#51773,#51774,#51775,#51776,
#51777,#51778,#51779,#51780,#51781,#51782,#51783,#51784,#51785,#51786,#51787,
#51788,#51789,#51790),.UNSPECIFIED.,.F.,.F.,(4,3,3,3,3,3,3,3,3,3,3,3,3,
3,3,3,3,3,3,3,3,3,3,3,3,3,3,3,3,3,3,3,3,3,3,3,3,3,3,3,3,3,3,3,3,3,3,3,3,
3,3,3,3,3,3,3,3,3,3,3,3,3,3,3,3,3,3,3,3,3,3,3,3,3,3,3,3,3,3,3,3,3,3,3,3,
3,3,3,3,3,3,3,3,3,3,3,3,3,3,3,3,3,3,3,3,3,3,3,3,3,3,3,3,3,3,3,3,3,3,3,3,
3,3,3,3,3,3,3,3,3,3,3,3,3,3,3,3,3,3,3,3,3,3,3,3,3,3,3,3,3,3,3,3,3,3,3,3,
3,3,3,3,3,3,3,3,3,3,3,3,3,3,3,3,3,3,3,3,3,3,3,3,3,3,3,3,3,3,3,3,3,3,3,3,
3,3,3,3,3,3,3,3,3,3,3,4),(3.00696909155215E-10,0.006896551724138,0.0124999836137833,
0.01379310344828,0.02068965517241,0.02758620689655,0.0287500147726358,0.03448275862069,
0.04137931034483,0.0449999960540127,0.04827586206897,0.0551724137931,0.061249990576592,
0.06206896551724,0.06896551724138,0.07586206896552,0.0775000201460335,0.08275862068966,
0.08965517241379,0.0937499863389232,0.09655172413793,0.1034482758621,0.109999997295967,
0.1103448275862,0.1172413793103,0.1241379310345,0.126250021167855,0.1310344827586,
0.1379310344828,0.142499980080655,0.1448275862069,0.151724137931,0.1586206896552,
0.15875000071435,0.1655172413793,0.1724137931034,0.17500001705366,0.1793103448276,
0.1862068965517,0.191249978763953,0.1931034482759,0.2,0.2068965517241,0.207500006105615,
0.2137931034483,0.2206896551724,0.223750008641753,0.2275862068966,0.2344827586207,
0.239999982367645,0.2413793103448,0.248275862069,0.2551724137931,0.256250013484737,
0.2620689655172,0.2689655172414,0.272499998025251,0.2758620689655,0.2827586206897,
0.288749989207179,0.2896551724138,0.2965517241379,0.3034482758621,0.305000019440364,
0.3103448275862,0.3172413793103,0.321249987913626,0.3241379310345,0.3310344827586,
0.337499996263586,0.3379310344828,0.3448275862069,0.351724137931,0.353750021363703,
0.3586206896552,0.3655172413793,0.369999980876539,0.3724137931034,0.3793103448276,
0.3862068965517,0.3931034482759,0.4,0.40250001816575,0.4068965517241,0.4137931034483,
0.41874997861438,0.4206896551724,0.4275862068966,0.4344827586207,0.435000004876984,
0.4413793103448,0.448275862069,0.451250010408905,0.4551724137931,0.4620689655172,
0.46749998140113,0.4689655172414,0.4758620689655,0.4827586206897,0.483750012153462,
0.4896551724138,0.4965517241379,0.499999999999995,0.5034482758621,0.5103448275862,
0.516249987846535,0.5172413793103,0.5241379310345,0.5310344827586,0.532500018598869,
0.5379310344828,0.5448275862069,0.548749989591095,0.551724137931,0.5586206896552,
0.564999995123012,0.5655172413793,0.5724137931034,0.5793103448276,0.581250021385624,
0.5862068965517,0.5931034482759,0.597499981834243,0.6,0.6068965517241,0.6137931034483,
0.6206896551724,0.6275862068966,0.630000019123452,0.6344827586207,0.6413793103448,
0.646249978636291,0.648275862069,0.6551724137931,0.6620689655172,0.662500003736419,
0.6689655172414,0.6758620689655,0.678750012086381,0.6827586206897,0.6896551724138,
0.694999980559641,0.6965517241379,0.7034482758621,0.7103448275862,0.711250010792824,
0.7172413793103,0.7241379310345,0.727500001974746,0.7310344827586,0.7379310344828,
0.743749986515264,0.7448275862069,0.751724137931,0.7586206896552,0.760000017632363,
0.7655172413793,0.7724137931034,0.776249991358243,0.7793103448276,0.7862068965517,
0.792499993894376,0.7931034482759,0.8,0.8068965517241,0.808750021236045,
0.8137931034483,0.8206896551724,0.82499998294634,0.8275862068966,0.8344827586207,
0.841249999285646,0.8413793103448,0.848275862069,0.8551724137931,0.85750001991935,
0.8620689655172,0.8689655172414,0.873749978832143,0.8758620689655,0.8827586206897,
0.8896551724138,0.890000002704033,0.8965517241379,0.9034482758621,0.906250013661082,
0.9103448275862,0.9172413793103,0.922499979853959,0.9241379310345,0.9310344827586,
0.9379310344828,0.938750009423415,0.9448275862069,0.951724137931,0.955000003945983,
0.9586206896552,0.9655172413793,0.971249985227355,0.9724137931034,0.9793103448276,
0.9862068965517,0.98750001638623,0.9931034482759,0.999999999124025),
 .UNSPECIFIED.);
#2462=LINE('',#12550,#2927);
#2463=LINE('',#12605,#2928);
#2464=LINE('',#12607,#2929);
#2465=LINE('',#12611,#2930);
#2466=LINE('',#12721,#2931);
#2467=LINE('',#12836,#2932);
#2468=LINE('',#12951,#2933);
#2469=LINE('',#13141,#2934);
#2470=LINE('',#13143,#2935);
#2471=LINE('',#13371,#2936);
#2472=LINE('',#13853,#2937);
#2473=LINE('',#14221,#2938);
#2474=LINE('',#14765,#2939);
#2475=LINE('',#15454,#2940);
#2476=LINE('',#15516,#2941);
#2477=LINE('',#15790,#2942);
#2478=LINE('',#16117,#2943);
#2479=LINE('',#16368,#2944);
#2480=LINE('',#16621,#2945);
#2481=LINE('',#17003,#2946);
#2482=LINE('',#17201,#2947);
#2483=LINE('',#17507,#2948);
#2484=LINE('',#17869,#2949);
#2485=LINE('',#18581,#2950);
#2486=LINE('',#18686,#2951);
#2487=LINE('',#18828,#2952);
#2488=LINE('',#18977,#2953);
#2489=LINE('',#19177,#2954);
#2490=LINE('',#19179,#2955);
#2491=LINE('',#19181,#2956);
#2492=LINE('',#19183,#2957);
#2493=LINE('',#19185,#2958);
#2494=LINE('',#19186,#2959);
#2495=LINE('',#19189,#2960);
#2496=LINE('',#19191,#2961);
#2497=LINE('',#19192,#2962);
#2498=LINE('',#19195,#2963);
#2499=LINE('',#19196,#2964);
#2500=LINE('',#19199,#2965);
#2501=LINE('',#19200,#2966);
#2502=LINE('',#19203,#2967);
#2503=LINE('',#19204,#2968);
#2504=LINE('',#19207,#2969);
#2505=LINE('',#19208,#2970);
#2506=LINE('',#19210,#2971);
#2507=LINE('',#19216,#2972);
#2508=LINE('',#19412,#2973);
#2509=LINE('',#19413,#2974);
#2510=LINE('',#19415,#2975);
#2511=LINE('',#19416,#2976);
#2512=LINE('',#19418,#2977);
#2513=LINE('',#19419,#2978);
#2514=LINE('',#19421,#2979);
#2515=LINE('',#19422,#2980);
#2516=LINE('',#19424,#2981);
#2517=LINE('',#19425,#2982);
#2518=LINE('',#19427,#2983);
#2519=LINE('',#19428,#2984);
#2520=LINE('',#19430,#2985);
#2521=LINE('',#19431,#2986);
#2522=LINE('',#19433,#2987);
#2523=LINE('',#19434,#2988);
#2524=LINE('',#19436,#2989);
#2525=LINE('',#19437,#2990);
#2526=LINE('',#19439,#2991);
#2527=LINE('',#19440,#2992);
#2528=LINE('',#19442,#2993);
#2529=LINE('',#19443,#2994);
#2530=LINE('',#19445,#2995);
#2531=LINE('',#19446,#2996);
#2532=LINE('',#19448,#2997);
#2533=LINE('',#19449,#2998);
#2534=LINE('',#19451,#2999);
#2535=LINE('',#19452,#3000);
#2536=LINE('',#19454,#3001);
#2537=LINE('',#19455,#3002);
#2538=LINE('',#19457,#3003);
#2539=LINE('',#19458,#3004);
#2540=LINE('',#19460,#3005);
#2541=LINE('',#19474,#3006);
#2542=LINE('',#19475,#3007);
#2543=LINE('',#19496,#3008);
#2544=LINE('',#19498,#3009);
#2545=LINE('',#19500,#3010);
#2546=LINE('',#19503,#3011);
#2547=LINE('',#19518,#3012);
#2548=LINE('',#19519,#3013);
#2549=LINE('',#19540,#3014);
#2550=LINE('',#19541,#3015);
#2551=LINE('',#19542,#3016);
#2552=LINE('',#19547,#3017);
#2553=LINE('',#19561,#3018);
#2554=LINE('',#19562,#3019);
#2555=LINE('',#19583,#3020);
#2556=LINE('',#19585,#3021);
#2557=LINE('',#19587,#3022);
#2558=LINE('',#19590,#3023);
#2559=LINE('',#19604,#3024);
#2560=LINE('',#19605,#3025);
#2561=LINE('',#19626,#3026);
#2562=LINE('',#19628,#3027);
#2563=LINE('',#19630,#3028);
#2564=LINE('',#19633,#3029);
#2565=LINE('',#19647,#3030);
#2566=LINE('',#19648,#3031);
#2567=LINE('',#19669,#3032);
#2568=LINE('',#19671,#3033);
#2569=LINE('',#19673,#3034);
#2570=LINE('',#19676,#3035);
#2571=LINE('',#19690,#3036);
#2572=LINE('',#19691,#3037);
#2573=LINE('',#19712,#3038);
#2574=LINE('',#19714,#3039);
#2575=LINE('',#19716,#3040);
#2576=LINE('',#19719,#3041);
#2577=LINE('',#19733,#3042);
#2578=LINE('',#19734,#3043);
#2579=LINE('',#19755,#3044);
#2580=LINE('',#19757,#3045);
#2581=LINE('',#19759,#3046);
#2582=LINE('',#19762,#3047);
#2583=LINE('',#19776,#3048);
#2584=LINE('',#19777,#3049);
#2585=LINE('',#19798,#3050);
#2586=LINE('',#19800,#3051);
#2587=LINE('',#19802,#3052);
#2588=LINE('',#19805,#3053);
#2589=LINE('',#19819,#3054);
#2590=LINE('',#19820,#3055);
#2591=LINE('',#19841,#3056);
#2592=LINE('',#19843,#3057);
#2593=LINE('',#19845,#3058);
#2594=LINE('',#19848,#3059);
#2595=LINE('',#19862,#3060);
#2596=LINE('',#19863,#3061);
#2597=LINE('',#19884,#3062);
#2598=LINE('',#19886,#3063);
#2599=LINE('',#19888,#3064);
#2600=LINE('',#19891,#3065);
#2601=LINE('',#19905,#3066);
#2602=LINE('',#19906,#3067);
#2603=LINE('',#19927,#3068);
#2604=LINE('',#19929,#3069);
#2605=LINE('',#19931,#3070);
#2606=LINE('',#19934,#3071);
#2607=LINE('',#19948,#3072);
#2608=LINE('',#19949,#3073);
#2609=LINE('',#19970,#3074);
#2610=LINE('',#19972,#3075);
#2611=LINE('',#19974,#3076);
#2612=LINE('',#19977,#3077);
#2613=LINE('',#19991,#3078);
#2614=LINE('',#19992,#3079);
#2615=LINE('',#20013,#3080);
#2616=LINE('',#20015,#3081);
#2617=LINE('',#20017,#3082);
#2618=LINE('',#20020,#3083);
#2619=LINE('',#20034,#3084);
#2620=LINE('',#20035,#3085);
#2621=LINE('',#20056,#3086);
#2622=LINE('',#20058,#3087);
#2623=LINE('',#20060,#3088);
#2624=LINE('',#20063,#3089);
#2625=LINE('',#20077,#3090);
#2626=LINE('',#20078,#3091);
#2627=LINE('',#20099,#3092);
#2628=LINE('',#20101,#3093);
#2629=LINE('',#20103,#3094);
#2630=LINE('',#20106,#3095);
#2631=LINE('',#20121,#3096);
#2632=LINE('',#20122,#3097);
#2633=LINE('',#20143,#3098);
#2634=LINE('',#20144,#3099);
#2635=LINE('',#20145,#3100);
#2636=LINE('',#20155,#3101);
#2637=LINE('',#20157,#3102);
#2638=LINE('',#20159,#3103);
#2639=LINE('',#20161,#3104);
#2640=LINE('',#20163,#3105);
#2641=LINE('',#20164,#3106);
#2642=LINE('',#20167,#3107);
#2643=LINE('',#20173,#3108);
#2644=LINE('',#20283,#3109);
#2645=LINE('',#20286,#3110);
#2646=LINE('',#20288,#3111);
#2647=LINE('',#20289,#3112);
#2648=LINE('',#20292,#3113);
#2649=LINE('',#20293,#3114);
#2650=LINE('',#20296,#3115);
#2651=LINE('',#20297,#3116);
#2652=LINE('',#20300,#3117);
#2653=LINE('',#20301,#3118);
#2654=LINE('',#20304,#3119);
#2655=LINE('',#20305,#3120);
#2656=LINE('',#20307,#3121);
#2657=LINE('',#20318,#3122);
#2658=LINE('',#20413,#3123);
#2659=LINE('',#20756,#3124);
#2660=LINE('',#21075,#3125);
#2661=LINE('',#21470,#3126);
#2662=LINE('',#21613,#3127);
#2663=LINE('',#22000,#3128);
#2664=LINE('',#22387,#3129);
#2665=LINE('',#23027,#3130);
#2666=LINE('',#23029,#3131);
#2667=LINE('',#23201,#3132);
#2668=LINE('',#23640,#3133);
#2669=LINE('',#24017,#3134);
#2670=LINE('',#24158,#3135);
#2671=LINE('',#24300,#3136);
#2672=LINE('',#24674,#3137);
#2673=LINE('',#25146,#3138);
#2674=LINE('',#25157,#3139);
#2675=LINE('',#25201,#3140);
#2676=LINE('',#25762,#3141);
#2677=LINE('',#26022,#3142);
#2678=LINE('',#26024,#3143);
#2679=LINE('',#26376,#3144);
#2680=LINE('',#26649,#3145);
#2681=LINE('',#26909,#3146);
#2682=LINE('',#27169,#3147);
#2683=LINE('',#27484,#3148);
#2684=LINE('',#27744,#3149);
#2685=LINE('',#28004,#3150);
#2686=LINE('',#28772,#3151);
#2687=LINE('',#28925,#3152);
#2688=LINE('',#29157,#3153);
#2689=LINE('',#29159,#3154);
#2690=LINE('',#29160,#3155);
#2691=LINE('',#29164,#3156);
#2692=LINE('',#29168,#3157);
#2693=LINE('',#29172,#3158);
#2694=LINE('',#29176,#3159);
#2695=LINE('',#29180,#3160);
#2696=LINE('',#29183,#3161);
#2697=LINE('',#29187,#3162);
#2698=LINE('',#29191,#3163);
#2699=LINE('',#29195,#3164);
#2700=LINE('',#29199,#3165);
#2701=LINE('',#29203,#3166);
#2702=LINE('',#29207,#3167);
#2703=LINE('',#29211,#3168);
#2704=LINE('',#29212,#3169);
#2705=LINE('',#29213,#3170);
#2706=LINE('',#29216,#3171);
#2707=LINE('',#29218,#3172);
#2708=LINE('',#29222,#3173);
#2709=LINE('',#29224,#3174);
#2710=LINE('',#29228,#3175);
#2711=LINE('',#29230,#3176);
#2712=LINE('',#29234,#3177);
#2713=LINE('',#29237,#3178);
#2714=LINE('',#29238,#3179);
#2715=LINE('',#29240,#3180);
#2716=LINE('',#29242,#3181);
#2717=LINE('',#29245,#3182);
#2718=LINE('',#29246,#3183);
#2719=LINE('',#29248,#3184);
#2720=LINE('',#29250,#3185);
#2721=LINE('',#29253,#3186);
#2722=LINE('',#29255,#3187);
#2723=LINE('',#29257,#3188);
#2724=LINE('',#29259,#3189);
#2725=LINE('',#29261,#3190);
#2726=LINE('',#29263,#3191);
#2727=LINE('',#29265,#3192);
#2728=LINE('',#29267,#3193);
#2729=LINE('',#29269,#3194);
#2730=LINE('',#29272,#3195);
#2731=LINE('',#29274,#3196);
#2732=LINE('',#29280,#3197);
#2733=LINE('',#29314,#3198);
#2734=LINE('',#29351,#3199);
#2735=LINE('',#29389,#3200);
#2736=LINE('',#29395,#3201);
#2737=LINE('',#29402,#3202);
#2738=LINE('',#29413,#3203);
#2739=LINE('',#29421,#3204);
#2740=LINE('',#29760,#3205);
#2741=LINE('',#29797,#3206);
#2742=LINE('',#31283,#3207);
#2743=LINE('',#32204,#3208);
#2744=LINE('',#32367,#3209);
#2745=LINE('',#32401,#3210);
#2746=LINE('',#32405,#3211);
#2747=LINE('',#32406,#3212);
#2748=LINE('',#32441,#3213);
#2749=LINE('',#32648,#3214);
#2750=LINE('',#32749,#3215);
#2751=LINE('',#32900,#3216);
#2752=LINE('',#32904,#3217);
#2753=LINE('',#32905,#3218);
#2754=LINE('',#33007,#3219);
#2755=LINE('',#33588,#3220);
#2756=LINE('',#33652,#3221);
#2757=LINE('',#33656,#3222);
#2758=LINE('',#33663,#3223);
#2759=LINE('',#34535,#3224);
#2760=LINE('',#34539,#3225);
#2761=LINE('',#34543,#3226);
#2762=LINE('',#34547,#3227);
#2763=LINE('',#34551,#3228);
#2764=LINE('',#34555,#3229);
#2765=LINE('',#34559,#3230);
#2766=LINE('',#34563,#3231);
#2767=LINE('',#34567,#3232);
#2768=LINE('',#34571,#3233);
#2769=LINE('',#34575,#3234);
#2770=LINE('',#34578,#3235);
#2771=LINE('',#34581,#3236);
#2772=LINE('',#34585,#3237);
#2773=LINE('',#34602,#3238);
#2774=LINE('',#34680,#3239);
#2775=LINE('',#34941,#3240);
#2776=LINE('',#35370,#3241);
#2777=LINE('',#35631,#3242);
#2778=LINE('',#36046,#3243);
#2779=LINE('',#36305,#3244);
#2780=LINE('',#36720,#3245);
#2781=LINE('',#36983,#3246);
#2782=LINE('',#37400,#3247);
#2783=LINE('',#37657,#3248);
#2784=LINE('',#38072,#3249);
#2785=LINE('',#39089,#3250);
#2786=LINE('',#39230,#3251);
#2787=LINE('',#39371,#3252);
#2788=LINE('',#39512,#3253);
#2789=LINE('',#39653,#3254);
#2790=LINE('',#39803,#3255);
#2791=LINE('',#39806,#3256);
#2792=LINE('',#39809,#3257);
#2793=LINE('',#39810,#3258);
#2794=LINE('',#39814,#3259);
#2795=LINE('',#39818,#3260);
#2796=LINE('',#39821,#3261);
#2797=LINE('',#39825,#3262);
#2798=LINE('',#39829,#3263);
#2799=LINE('',#39833,#3264);
#2800=LINE('',#39837,#3265);
#2801=LINE('',#39841,#3266);
#2802=LINE('',#39845,#3267);
#2803=LINE('',#39849,#3268);
#2804=LINE('',#39853,#3269);
#2805=LINE('',#39856,#3270);
#2806=LINE('',#39857,#3271);
#2807=LINE('',#39859,#3272);
#2808=LINE('',#39861,#3273);
#2809=LINE('',#39863,#3274);
#2810=LINE('',#39865,#3275);
#2811=LINE('',#39867,#3276);
#2812=LINE('',#39869,#3277);
#2813=LINE('',#39871,#3278);
#2814=LINE('',#39873,#3279);
#2815=LINE('',#39875,#3280);
#2816=LINE('',#39877,#3281);
#2817=LINE('',#39879,#3282);
#2818=LINE('',#39881,#3283);
#2819=LINE('',#39883,#3284);
#2820=LINE('',#39885,#3285);
#2821=LINE('',#39887,#3286);
#2822=LINE('',#39889,#3287);
#2823=LINE('',#39892,#3288);
#2824=LINE('',#39894,#3289);
#2825=LINE('',#39896,#3290);
#2826=LINE('',#39902,#3291);
#2827=LINE('',#39904,#3292);
#2828=LINE('',#39906,#3293);
#2829=LINE('',#39920,#3294);
#2830=LINE('',#39933,#3295);
#2831=LINE('',#39942,#3296);
#2832=LINE('',#39947,#3297);
#2833=LINE('',#39970,#3298);
#2834=LINE('',#40327,#3299);
#2835=LINE('',#40513,#3300);
#2836=LINE('',#40660,#3301);
#2837=LINE('',#40913,#3302);
#2838=LINE('',#41165,#3303);
#2839=LINE('',#41597,#3304);
#2840=LINE('',#42029,#3305);
#2841=LINE('',#42391,#3306);
#2842=LINE('',#43224,#3307);
#2843=LINE('',#43377,#3308);
#2844=LINE('',#43431,#3309);
#2845=LINE('',#43600,#3310);
#2846=LINE('',#43632,#3311);
#2847=LINE('',#43634,#3312);
#2848=LINE('',#43640,#3313);
#2849=LINE('',#43644,#3314);
#2850=LINE('',#43649,#3315);
#2851=LINE('',#43655,#3316);
#2852=LINE('',#43659,#3317);
#2853=LINE('',#43663,#3318);
#2854=LINE('',#43669,#3319);
#2855=LINE('',#44053,#3320);
#2856=LINE('',#44054,#3321);
#2857=LINE('',#44060,#3322);
#2858=LINE('',#44064,#3323);
#2859=LINE('',#44065,#3324);
#2860=LINE('',#44073,#3325);
#2861=LINE('',#44078,#3326);
#2862=LINE('',#44081,#3327);
#2863=LINE('',#44085,#3328);
#2864=LINE('',#44096,#3329);
#2865=LINE('',#44099,#3330);
#2866=LINE('',#44104,#3331);
#2867=LINE('',#44108,#3332);
#2868=LINE('',#44136,#3333);
#2869=LINE('',#44499,#3334);
#2870=LINE('',#44543,#3335);
#2871=LINE('',#44547,#3336);
#2872=LINE('',#45184,#3337);
#2873=LINE('',#45200,#3338);
#2874=LINE('',#45202,#3339);
#2875=LINE('',#45205,#3340);
#2876=LINE('',#45211,#3341);
#2877=LINE('',#45218,#3342);
#2878=LINE('',#45219,#3343);
#2879=LINE('',#45225,#3344);
#2880=LINE('',#45229,#3345);
#2881=LINE('',#45232,#3346);
#2882=LINE('',#45233,#3347);
#2883=LINE('',#45235,#3348);
#2884=LINE('',#45236,#3349);
#2885=LINE('',#45240,#3350);
#2886=LINE('',#45241,#3351);
#2887=LINE('',#45532,#3352);
#2888=LINE('',#45533,#3353);
#2889=LINE('',#45534,#3354);
#2890=LINE('',#45593,#3355);
#2891=LINE('',#45708,#3356);
#2892=LINE('',#45710,#3357);
#2893=LINE('',#46032,#3358);
#2894=LINE('',#46033,#3359);
#2895=LINE('',#46055,#3360);
#2896=LINE('',#46206,#3361);
#2897=LINE('',#46384,#3362);
#2898=LINE('',#46385,#3363);
#2899=LINE('',#46388,#3364);
#2900=LINE('',#46392,#3365);
#2901=LINE('',#46396,#3366);
#2902=LINE('',#46400,#3367);
#2903=LINE('',#46404,#3368);
#2904=LINE('',#46407,#3369);
#2905=LINE('',#46412,#3370);
#2906=LINE('',#46441,#3371);
#2907=LINE('',#47625,#3372);
#2908=LINE('',#48062,#3373);
#2909=LINE('',#48677,#3374);
#2910=LINE('',#49625,#3375);
#2911=LINE('',#50640,#3376);
#2912=LINE('',#50909,#3377);
#2913=LINE('',#52060,#3378);
#2914=LINE('',#52062,#3379);
#2915=LINE('',#52064,#3380);
#2916=LINE('',#52066,#3381);
#2917=LINE('',#52068,#3382);
#2918=LINE('',#52070,#3383);
#2919=LINE('',#52072,#3384);
#2920=LINE('',#52074,#3385);
#2921=LINE('',#52076,#3386);
#2922=LINE('',#52078,#3387);
#2923=LINE('',#52093,#3388);
#2924=LINE('',#52099,#3389);
#2925=LINE('',#52108,#3390);
#2926=LINE('',#52117,#3391);
#2927=VECTOR('',#10216,2.25);
#2928=VECTOR('',#10217,2.25);
#2929=VECTOR('',#10220,1.176);
#2930=VECTOR('',#10223,2.25);
#2931=VECTOR('',#10226,2.25);
#2932=VECTOR('',#10229,2.25);
#2933=VECTOR('',#10232,2.25);
#2934=VECTOR('',#10237,2.25);
#2935=VECTOR('',#10240,1.176);
#2936=VECTOR('',#10241,0.939826579747624);
#2937=VECTOR('',#10244,0.939826579747624);
#2938=VECTOR('',#10245,0.245);
#2939=VECTOR('',#10246,0.245);
#2940=VECTOR('',#10251,0.2381569860407);
#2941=VECTOR('',#10254,0.3125);
#2942=VECTOR('',#10257,0.281746931364498);
#2943=VECTOR('',#10258,0.281746931364498);
#2944=VECTOR('',#10259,0.1682530686355);
#2945=VECTOR('',#10260,0.1682530686355);
#2946=VECTOR('',#10261,0.281746931364498);
#2947=VECTOR('',#10262,0.281746931364498);
#2948=VECTOR('',#10263,0.281746931364491);
#2949=VECTOR('',#10264,0.281746931364491);
#2950=VECTOR('',#10267,0.238156986040692);
#2951=VECTOR('',#10272,0.1375);
#2952=VECTOR('',#10275,0.1682530686355);
#2953=VECTOR('',#10286,3.5);
#2954=VECTOR('',#10487,2.54034118443391);
#2955=VECTOR('',#10488,2.54034118443391);
#2956=VECTOR('',#10489,2.540341184434);
#2957=VECTOR('',#10490,2.54034118443391);
#2958=VECTOR('',#10491,2.54034118443391);
#2959=VECTOR('',#10492,2.540341184434);
#2960=VECTOR('',#10495,4.4);
#2961=VECTOR('',#10496,2.54034118443391);
#2962=VECTOR('',#10497,4.4);
#2963=VECTOR('',#10500,2.54034118443391);
#2964=VECTOR('',#10501,4.4);
#2965=VECTOR('',#10504,2.540341184434);
#2966=VECTOR('',#10505,4.4);
#2967=VECTOR('',#10508,2.54034118443391);
#2968=VECTOR('',#10509,4.4);
#2969=VECTOR('',#10512,2.54034118443391);
#2970=VECTOR('',#10513,4.4);
#2971=VECTOR('',#10516,2.540341184434);
#2972=VECTOR('',#10523,3.5);
#2973=VECTOR('',#10722,5.8);
#2974=VECTOR('',#10723,5.8);
#2975=VECTOR('',#10726,5.8);
#2976=VECTOR('',#10727,5.8);
#2977=VECTOR('',#10730,5.8);
#2978=VECTOR('',#10731,5.8);
#2979=VECTOR('',#10734,5.8);
#2980=VECTOR('',#10735,5.8);
#2981=VECTOR('',#10738,5.8);
#2982=VECTOR('',#10739,5.8);
#2983=VECTOR('',#10742,5.8);
#2984=VECTOR('',#10743,5.8);
#2985=VECTOR('',#10746,5.8);
#2986=VECTOR('',#10747,5.8);
#2987=VECTOR('',#10750,5.8);
#2988=VECTOR('',#10751,5.8);
#2989=VECTOR('',#10754,5.8);
#2990=VECTOR('',#10755,5.8);
#2991=VECTOR('',#10758,5.8);
#2992=VECTOR('',#10759,5.8);
#2993=VECTOR('',#10762,5.8);
#2994=VECTOR('',#10763,5.8);
#2995=VECTOR('',#10766,5.8);
#2996=VECTOR('',#10767,5.8);
#2997=VECTOR('',#10770,5.8);
#2998=VECTOR('',#10771,5.8);
#2999=VECTOR('',#10774,5.8);
#3000=VECTOR('',#10775,5.8);
#3001=VECTOR('',#10778,5.8);
#3002=VECTOR('',#10779,5.8);
#3003=VECTOR('',#10782,5.8);
#3004=VECTOR('',#10783,5.8);
#3005=VECTOR('',#10786,5.8);
#3006=VECTOR('',#10789,1.486313498852);
#3007=VECTOR('',#10790,1.486313498852);
#3008=VECTOR('',#10799,1.486313498852);
#3009=VECTOR('',#10802,1.486313498852);
#3010=VECTOR('',#10805,5.8);
#3011=VECTOR('',#10810,5.8);
#3012=VECTOR('',#10813,1.486313498852);
#3013=VECTOR('',#10814,1.486313498852);
#3014=VECTOR('',#10823,1.486313498852);
#3015=VECTOR('',#10824,5.8);
#3016=VECTOR('',#10825,1.486313498852);
#3017=VECTOR('',#10834,5.8);
#3018=VECTOR('',#10837,1.486313498852);
#3019=VECTOR('',#10838,1.486313498852);
#3020=VECTOR('',#10847,1.486313498852);
#3021=VECTOR('',#10850,1.486313498852);
#3022=VECTOR('',#10853,5.8);
#3023=VECTOR('',#10858,5.8);
#3024=VECTOR('',#10861,1.486313498852);
#3025=VECTOR('',#10862,1.486313498852);
#3026=VECTOR('',#10871,1.486313498852);
#3027=VECTOR('',#10874,1.486313498852);
#3028=VECTOR('',#10877,5.8);
#3029=VECTOR('',#10882,5.8);
#3030=VECTOR('',#10885,1.486313498852);
#3031=VECTOR('',#10886,1.486313498852);
#3032=VECTOR('',#10895,1.486313498852);
#3033=VECTOR('',#10898,1.486313498852);
#3034=VECTOR('',#10901,5.8);
#3035=VECTOR('',#10906,5.8);
#3036=VECTOR('',#10909,1.486313498852);
#3037=VECTOR('',#10910,1.486313498852);
#3038=VECTOR('',#10919,1.486313498852);
#3039=VECTOR('',#10922,1.486313498852);
#3040=VECTOR('',#10925,5.8);
#3041=VECTOR('',#10930,5.8);
#3042=VECTOR('',#10933,1.486313498852);
#3043=VECTOR('',#10934,1.486313498852);
#3044=VECTOR('',#10943,1.486313498852);
#3045=VECTOR('',#10946,1.486313498852);
#3046=VECTOR('',#10949,5.8);
#3047=VECTOR('',#10954,5.8);
#3048=VECTOR('',#10957,1.486313498852);
#3049=VECTOR('',#10958,1.486313498852);
#3050=VECTOR('',#10967,1.486313498852);
#3051=VECTOR('',#10970,1.486313498852);
#3052=VECTOR('',#10973,5.8);
#3053=VECTOR('',#10978,5.8);
#3054=VECTOR('',#10981,1.486313498852);
#3055=VECTOR('',#10982,1.486313498852);
#3056=VECTOR('',#10991,1.486313498852);
#3057=VECTOR('',#10994,1.486313498852);
#3058=VECTOR('',#10997,5.8);
#3059=VECTOR('',#11002,5.8);
#3060=VECTOR('',#11005,1.486313498852);
#3061=VECTOR('',#11006,1.486313498852);
#3062=VECTOR('',#11015,1.486313498852);
#3063=VECTOR('',#11018,1.486313498852);
#3064=VECTOR('',#11021,5.8);
#3065=VECTOR('',#11026,5.8);
#3066=VECTOR('',#11029,1.486313498852);
#3067=VECTOR('',#11030,1.486313498852);
#3068=VECTOR('',#11039,1.486313498852);
#3069=VECTOR('',#11042,1.486313498852);
#3070=VECTOR('',#11045,5.8);
#3071=VECTOR('',#11050,5.8);
#3072=VECTOR('',#11053,1.486313498852);
#3073=VECTOR('',#11054,1.486313498852);
#3074=VECTOR('',#11063,1.486313498852);
#3075=VECTOR('',#11066,1.486313498852);
#3076=VECTOR('',#11069,5.8);
#3077=VECTOR('',#11074,5.8);
#3078=VECTOR('',#11077,1.486313498852);
#3079=VECTOR('',#11078,1.486313498852);
#3080=VECTOR('',#11087,1.486313498852);
#3081=VECTOR('',#11090,1.486313498852);
#3082=VECTOR('',#11093,5.8);
#3083=VECTOR('',#11098,5.8);
#3084=VECTOR('',#11101,1.486313498852);
#3085=VECTOR('',#11102,1.486313498852);
#3086=VECTOR('',#11111,1.486313498852);
#3087=VECTOR('',#11114,1.486313498852);
#3088=VECTOR('',#11117,5.8);
#3089=VECTOR('',#11122,5.8);
#3090=VECTOR('',#11125,1.486313498852);
#3091=VECTOR('',#11126,1.486313498852);
#3092=VECTOR('',#11135,1.486313498852);
#3093=VECTOR('',#11138,1.486313498852);
#3094=VECTOR('',#11141,5.8);
#3095=VECTOR('',#11146,5.8);
#3096=VECTOR('',#11149,1.486313498852);
#3097=VECTOR('',#11150,1.486313498852);
#3098=VECTOR('',#11159,1.486313498852);
#3099=VECTOR('',#11160,5.8);
#3100=VECTOR('',#11161,1.486313498852);
#3101=VECTOR('',#11174,2.42487113059592);
#3102=VECTOR('',#11175,2.424871130596);
#3103=VECTOR('',#11176,2.42487113059592);
#3104=VECTOR('',#11177,2.42487113059592);
#3105=VECTOR('',#11178,2.424871130596);
#3106=VECTOR('',#11179,2.42487113059592);
#3107=VECTOR('',#11182,3.);
#3108=VECTOR('',#11189,3.);
#3109=VECTOR('',#11202,0.9);
#3110=VECTOR('',#11205,4.4);
#3111=VECTOR('',#11206,2.42487113059592);
#3112=VECTOR('',#11207,4.4);
#3113=VECTOR('',#11210,2.424871130596);
#3114=VECTOR('',#11211,4.4);
#3115=VECTOR('',#11214,2.42487113059592);
#3116=VECTOR('',#11215,4.4);
#3117=VECTOR('',#11218,2.42487113059592);
#3118=VECTOR('',#11219,4.4);
#3119=VECTOR('',#11222,2.424871130596);
#3120=VECTOR('',#11223,4.4);
#3121=VECTOR('',#11226,2.42487113059592);
#3122=VECTOR('',#11231,0.1596734338228);
#3123=VECTOR('',#11234,0.09218749999999);
#3124=VECTOR('',#11235,0.384529946162085);
#3125=VECTOR('',#11236,0.384529946162085);
#3126=VECTOR('',#11237,0.1154700538379);
#3127=VECTOR('',#11238,0.1154700538379);
#3128=VECTOR('',#11239,0.1154700538379);
#3129=VECTOR('',#11240,0.1154700538379);
#3130=VECTOR('',#11243,0.1596734338228);
#3131=VECTOR('',#11244,0.4078125);
#3132=VECTOR('',#11249,0.384529946162085);
#3133=VECTOR('',#11252,0.384529946162085);
#3134=VECTOR('',#11253,0.384529946162088);
#3135=VECTOR('',#11254,0.384529946162088);
#3136=VECTOR('',#11255,0.384529946162088);
#3137=VECTOR('',#11256,0.384529946162088);
#3138=VECTOR('',#11269,1.6);
#3139=VECTOR('',#11284,1.393148400081);
#3140=VECTOR('',#11293,0.02886751345948);
#3141=VECTOR('',#11296,0.05773502691896);
#3142=VECTOR('',#11297,0.442264973080985);
#3143=VECTOR('',#11298,0.442264973080985);
#3144=VECTOR('',#11301,0.442264973080985);
#3145=VECTOR('',#11302,0.442264973080985);
#3146=VECTOR('',#11303,0.05773502691896);
#3147=VECTOR('',#11304,0.442264973080985);
#3148=VECTOR('',#11305,0.442264973080985);
#3149=VECTOR('',#11306,0.05773502691896);
#3150=VECTOR('',#11307,0.442264973080985);
#3151=VECTOR('',#11320,0.290824116479001);
#3152=VECTOR('',#11329,3.);
#3153=VECTOR('',#11350,1.48424358004605);
#3154=VECTOR('',#11351,0.2394366603764);
#3155=VECTOR('',#11352,1.48424358004605);
#3156=VECTOR('',#11357,1.50481684780505);
#3157=VECTOR('',#11360,0.4019026509541);
#3158=VECTOR('',#11363,0.2394366603764);
#3159=VECTOR('',#11366,0.4019026509541);
#3160=VECTOR('',#11369,0.4019026509541);
#3161=VECTOR('',#11372,0.4019026509541);
#3162=VECTOR('',#11375,0.4019026509541);
#3163=VECTOR('',#11378,0.2394366603764);
#3164=VECTOR('',#11381,0.4019026509541);
#3165=VECTOR('',#11384,0.4019026509541);
#3166=VECTOR('',#11387,0.2394366603764);
#3167=VECTOR('',#11390,0.4019026509541);
#3168=VECTOR('',#11395,0.2218939514837);
#3169=VECTOR('',#11396,1.50481684780505);
#3170=VECTOR('',#11397,1.51143779167605);
#3171=VECTOR('',#11400,0.2218939514837);
#3172=VECTOR('',#11401,0.2218939514837);
#3173=VECTOR('',#11406,0.2218939514837);
#3174=VECTOR('',#11407,0.2218939514837);
#3175=VECTOR('',#11412,0.2218939514837);
#3176=VECTOR('',#11413,0.2218939514837);
#3177=VECTOR('',#11418,0.2218939514837);
#3178=VECTOR('',#11423,1.51143779167605);
#3179=VECTOR('',#11424,1.50481684780505);
#3180=VECTOR('',#11427,1.48424358004605);
#3181=VECTOR('',#11430,1.48424358004605);
#3182=VECTOR('',#11435,1.48424358004605);
#3183=VECTOR('',#11436,1.48424358004605);
#3184=VECTOR('',#11439,1.50481684780505);
#3185=VECTOR('',#11442,1.51143779167605);
#3186=VECTOR('',#11447,1.50481684780505);
#3187=VECTOR('',#11450,1.51143779167605);
#3188=VECTOR('',#11453,1.51143779167605);
#3189=VECTOR('',#11456,1.50481684780505);
#3190=VECTOR('',#11459,1.48424358004605);
#3191=VECTOR('',#11462,1.48424358004605);
#3192=VECTOR('',#11465,1.50481684780505);
#3193=VECTOR('',#11468,1.51143779167605);
#3194=VECTOR('',#11471,1.51143779167605);
#3195=VECTOR('',#11476,1.51143779167605);
#3196=VECTOR('',#11479,1.50481684780505);
#3197=VECTOR('',#11486,0.6826696020578);
#3198=VECTOR('',#11487,4.991813260128);
#3199=VECTOR('',#11488,0.6826695987007);
#3200=VECTOR('',#11495,0.7035430188284);
#3201=VECTOR('',#11502,0.7035430205274);
#3202=VECTOR('',#11509,0.7035430198318);
#3203=VECTOR('',#11522,0.703543023457);
#3204=VECTOR('',#11531,0.6826696018365);
#3205=VECTOR('',#11564,4.991813260138);
#3206=VECTOR('',#11565,0.6826695985817);
#3207=VECTOR('',#11622,4.875081924963);
#3208=VECTOR('',#11707,10.);
#3209=VECTOR('',#11708,10.);
#3210=VECTOR('',#11709,10.);
#3211=VECTOR('',#11714,10.);
#3212=VECTOR('',#11715,4.493663028249);
#3213=VECTOR('',#11718,10.);
#3214=VECTOR('',#11721,10.);
#3215=VECTOR('',#11726,4.875081924964);
#3216=VECTOR('',#11731,10.);
#3217=VECTOR('',#11736,10.);
#3218=VECTOR('',#11737,4.49366302825);
#3219=VECTOR('',#11744,4.515053245399);
#3220=VECTOR('',#11751,4.5150532454);
#3221=VECTOR('',#11766,1.925);
#3222=VECTOR('',#11771,1.25);
#3223=VECTOR('',#11780,2.5);
#3224=VECTOR('',#11807,0.4519026509541);
#3225=VECTOR('',#11810,0.3019026509541);
#3226=VECTOR('',#11813,0.4519026509541);
#3227=VECTOR('',#11816,0.4519026509541);
#3228=VECTOR('',#11819,0.3019026509541);
#3229=VECTOR('',#11822,0.4519026509541);
#3230=VECTOR('',#11825,0.4519026509541);
#3231=VECTOR('',#11828,0.3019026509541);
#3232=VECTOR('',#11831,0.4519026509541);
#3233=VECTOR('',#11834,0.4519026509541);
#3234=VECTOR('',#11837,0.3019026509541);
#3235=VECTOR('',#11840,0.4519026509541);
#3236=VECTOR('',#11843,2.35);
#3237=VECTOR('',#11848,1.725);
#3238=VECTOR('',#11863,1.175);
#3239=VECTOR('',#11868,0.45);
#3240=VECTOR('',#11869,0.323316150746213);
#3241=VECTOR('',#11870,0.323316150746213);
#3242=VECTOR('',#11871,0.32331615074619);
#3243=VECTOR('',#11872,0.32331615074619);
#3244=VECTOR('',#11873,0.323316150746185);
#3245=VECTOR('',#11874,0.323316150746185);
#3246=VECTOR('',#11875,0.323316150746214);
#3247=VECTOR('',#11876,0.323316150746214);
#3248=VECTOR('',#11877,0.3233161507462);
#3249=VECTOR('',#11878,0.3233161507462);
#3250=VECTOR('',#11881,0.1266838492538);
#3251=VECTOR('',#11882,0.1266838492538);
#3252=VECTOR('',#11883,0.1266838492538);
#3253=VECTOR('',#11884,0.1266838492538);
#3254=VECTOR('',#11885,0.1266838492538);
#3255=VECTOR('',#11890,1.20915023334004);
#3256=VECTOR('',#11893,1.20915023334004);
#3257=VECTOR('',#11896,1.20915023334004);
#3258=VECTOR('',#11897,0.4519026509541);
#3259=VECTOR('',#11900,0.4519026509541);
#3260=VECTOR('',#11903,0.09192985849191);
#3261=VECTOR('',#11906,0.4519026509541);
#3262=VECTOR('',#11909,0.09192985849191);
#3263=VECTOR('',#11912,0.4519026509541);
#3264=VECTOR('',#11915,0.4519026509541);
#3265=VECTOR('',#11918,0.09192985849191);
#3266=VECTOR('',#11921,0.4519026509541);
#3267=VECTOR('',#11924,0.4519026509541);
#3268=VECTOR('',#11927,0.09192985849191);
#3269=VECTOR('',#11930,0.4519026509541);
#3270=VECTOR('',#11935,1.20915023334004);
#3271=VECTOR('',#11936,1.20915023334004);
#3272=VECTOR('',#11939,1.20915023334004);
#3273=VECTOR('',#11942,1.20915023334004);
#3274=VECTOR('',#11945,1.20915023334004);
#3275=VECTOR('',#11948,1.20915023334004);
#3276=VECTOR('',#11951,1.20915023334004);
#3277=VECTOR('',#11954,1.20915023334004);
#3278=VECTOR('',#11957,1.20915023334004);
#3279=VECTOR('',#11960,1.20915023334004);
#3280=VECTOR('',#11963,1.20915023334004);
#3281=VECTOR('',#11966,1.20915023334004);
#3282=VECTOR('',#11969,1.20915023334004);
#3283=VECTOR('',#11972,1.20915023334004);
#3284=VECTOR('',#11975,1.20915023334004);
#3285=VECTOR('',#11978,1.20915023334004);
#3286=VECTOR('',#11981,1.20915023334004);
#3287=VECTOR('',#11984,1.20915023334004);
#3288=VECTOR('',#11989,1.20915023334004);
#3289=VECTOR('',#11992,1.20915023334004);
#3290=VECTOR('',#11995,1.20915023334004);
#3291=VECTOR('',#12002,8.999999999839);
#3292=VECTOR('',#12003,15.48856626783);
#3293=VECTOR('',#12004,5.09731398179822);
#3294=VECTOR('',#12005,2.18647853617101);
#3295=VECTOR('',#12022,5.);
#3296=VECTOR('',#12033,4.);
#3297=VECTOR('',#12038,4.);
#3298=VECTOR('',#12039,0.75);
#3299=VECTOR('',#12042,0.461880215351696);
#3300=VECTOR('',#12043,0.461880215351696);
#3301=VECTOR('',#12044,0.2881197846483);
#3302=VECTOR('',#12045,0.2881197846483);
#3303=VECTOR('',#12046,0.461880215351696);
#3304=VECTOR('',#12047,0.461880215351696);
#3305=VECTOR('',#12048,0.461880215351684);
#3306=VECTOR('',#12049,0.461880215351684);
#3307=VECTOR('',#12050,0.2881197846483);
#3308=VECTOR('',#12059,6.);
#3309=VECTOR('',#12068,6.75);
#3310=VECTOR('',#12073,2.473089489284);
#3311=VECTOR('',#12074,15.15835238946);
#3312=VECTOR('',#12075,10.99999999936);
#3313=VECTOR('',#12080,4.78408308320006);
#3314=VECTOR('',#12083,4.78408308319393);
#3315=VECTOR('',#12088,2.22834709131601);
#3316=VECTOR('',#12095,1.25);
#3317=VECTOR('',#12098,3.38573837870217);
#3318=VECTOR('',#12101,3.38573819298811);
#3319=VECTOR('',#12108,4.78408308337184);
#3320=VECTOR('',#12125,1.5);
#3321=VECTOR('',#12126,1.5);
#3322=VECTOR('',#12135,4.78408308309884);
#3323=VECTOR('',#12140,1.5);
#3324=VECTOR('',#12141,4.78408308336584);
#3325=VECTOR('',#12154,1.5);
#3326=VECTOR('',#12161,4.78408308310784);
#3327=VECTOR('',#12166,1.5);
#3328=VECTOR('',#12171,1.5);
#3329=VECTOR('',#12186,8.85);
#3330=VECTOR('',#12189,8.85);
#3331=VECTOR('',#12196,2.22834723186102);
#3332=VECTOR('',#12201,2.18647846971201);
#3333=VECTOR('',#12202,3.745592232445);
#3334=VECTOR('',#12211,2.459549577106);
#3335=VECTOR('',#12218,8.13705833981064);
#3336=VECTOR('',#12221,8.16003640112219);
#3337=VECTOR('',#12236,15.16332099539);
#3338=VECTOR('',#12245,11.);
#3339=VECTOR('',#12246,5.85);
#3340=VECTOR('',#12249,8.999999999998);
#3341=VECTOR('',#12256,3.6);
#3342=VECTOR('',#12265,3.23);
#3343=VECTOR('',#12266,3.23);
#3344=VECTOR('',#12271,2.503692708007);
#3345=VECTOR('',#12274,2.453282759045);
#3346=VECTOR('',#12277,2.450330288028);
#3347=VECTOR('',#12278,2.494111584205);
#3348=VECTOR('',#12281,7.36244219026491);
#3349=VECTOR('',#12282,7.35020412958116);
#3350=VECTOR('',#12287,3.745592232442);
#3351=VECTOR('',#12288,7.31329808179909);
#3352=VECTOR('',#12301,5.10538702111419);
#3353=VECTOR('',#12302,8.10150600096205);
#3354=VECTOR('',#12303,7.22099758100766);
#3355=VECTOR('',#12308,8.10459673698465);
#3356=VECTOR('',#12315,3.838901255888);
#3357=VECTOR('',#12316,3.83784463984698);
#3358=VECTOR('',#12329,5.849999999044);
#3359=VECTOR('',#12330,15.49166557366);
#3360=VECTOR('',#12367,4.);
#3361=VECTOR('',#12388,3.125);
#3362=VECTOR('',#12397,1.239616396338);
#3363=VECTOR('',#12398,1.239616396338);
#3364=VECTOR('',#12401,4.61880215351685);
#3365=VECTOR('',#12404,4.618802153517);
#3366=VECTOR('',#12407,4.61880215351685);
#3367=VECTOR('',#12410,4.61880215351685);
#3368=VECTOR('',#12413,4.618802153517);
#3369=VECTOR('',#12416,4.61880215351685);
#3370=VECTOR('',#12421,4.);
#3371=VECTOR('',#12422,0.75);
#3372=VECTOR('',#12425,0.531162247654508);
#3373=VECTOR('',#12426,0.531162247654478);
#3374=VECTOR('',#12427,0.531162247654508);
#3375=VECTOR('',#12428,0.531162247654478);
#3376=VECTOR('',#12429,0.2188377523455);
#3377=VECTOR('',#12430,0.2188377523455);
#3378=VECTOR('',#12433,1.239616396338);
#3379=VECTOR('',#12436,1.239616396338);
#3380=VECTOR('',#12439,1.239616396338);
#3381=VECTOR('',#12442,1.239616396338);
#3382=VECTOR('',#12445,1.239616396338);
#3383=VECTOR('',#12448,1.239616396338);
#3384=VECTOR('',#12451,1.239616396338);
#3385=VECTOR('',#12454,1.239616396338);
#3386=VECTOR('',#12457,1.239616396338);
#3387=VECTOR('',#12460,1.239616396338);
#3388=VECTOR('',#12481,2.5);
#3389=VECTOR('',#12490,3.8);
#3390=VECTOR('',#12501,6.65);
#3391=VECTOR('',#12512,5.65);
#3392=VERTEX_POINT('',#12548);
#3393=VERTEX_POINT('',#12549);
#3394=VERTEX_POINT('',#12551);
#3395=VERTEX_POINT('',#12604);
#3396=VERTEX_POINT('',#12609);
#3397=VERTEX_POINT('',#12610);
#3398=VERTEX_POINT('',#12719);
#3399=VERTEX_POINT('',#12720);
#3400=VERTEX_POINT('',#12722);
#3401=VERTEX_POINT('',#12834);
#3402=VERTEX_POINT('',#12835);
#3403=VERTEX_POINT('',#12891);
#3404=VERTEX_POINT('',#12949);
#3405=VERTEX_POINT('',#12950);
#3406=VERTEX_POINT('',#13059);
#3407=VERTEX_POINT('',#13066);
#3408=VERTEX_POINT('',#13073);
#3409=VERTEX_POINT('',#13087);
#3410=VERTEX_POINT('',#13140);
#3411=VERTEX_POINT('',#13284);
#3412=VERTEX_POINT('',#13512);
#3413=VERTEX_POINT('',#13606);
#3414=VERTEX_POINT('',#13613);
#3415=VERTEX_POINT('',#13766);
#3416=VERTEX_POINT('',#14220);
#3417=VERTEX_POINT('',#15450);
#3418=VERTEX_POINT('',#15451);
#3419=VERTEX_POINT('',#15453);
#3420=VERTEX_POINT('',#15455);
#3421=VERTEX_POINT('',#15475);
#3422=VERTEX_POINT('',#15518);
#3423=VERTEX_POINT('',#15525);
#3424=VERTEX_POINT('',#15678);
#3425=VERTEX_POINT('',#15789);
#3426=VERTEX_POINT('',#16061);
#3427=VERTEX_POINT('',#16116);
#3428=VERTEX_POINT('',#16509);
#3429=VERTEX_POINT('',#16620);
#3430=VERTEX_POINT('',#16872);
#3431=VERTEX_POINT('',#17144);
#3432=VERTEX_POINT('',#17342);
#3433=VERTEX_POINT('',#17455);
#3434=VERTEX_POINT('',#17506);
#3435=VERTEX_POINT('',#17758);
#3436=VERTEX_POINT('',#18010);
#3437=VERTEX_POINT('',#18139);
#3438=VERTEX_POINT('',#18146);
#3439=VERTEX_POINT('',#18401);
#3440=VERTEX_POINT('',#18402);
#3441=VERTEX_POINT('',#18580);
#3442=VERTEX_POINT('',#18582);
#3443=VERTEX_POINT('',#18970);
#3444=VERTEX_POINT('',#18973);
#3445=VERTEX_POINT('',#18974);
#3446=VERTEX_POINT('',#18979);
#3447=VERTEX_POINT('',#18983);
#3448=VERTEX_POINT('',#18984);
#3449=VERTEX_POINT('',#18986);
#3450=VERTEX_POINT('',#18988);
#3451=VERTEX_POINT('',#18990);
#3452=VERTEX_POINT('',#18992);
#3453=VERTEX_POINT('',#18994);
#3454=VERTEX_POINT('',#18996);
#3455=VERTEX_POINT('',#18998);
#3456=VERTEX_POINT('',#19000);
#3457=VERTEX_POINT('',#19002);
#3458=VERTEX_POINT('',#19004);
#3459=VERTEX_POINT('',#19006);
#3460=VERTEX_POINT('',#19008);
#3461=VERTEX_POINT('',#19010);
#3462=VERTEX_POINT('',#19012);
#3463=VERTEX_POINT('',#19014);
#3464=VERTEX_POINT('',#19016);
#3465=VERTEX_POINT('',#19018);
#3466=VERTEX_POINT('',#19020);
#3467=VERTEX_POINT('',#19022);
#3468=VERTEX_POINT('',#19024);
#3469=VERTEX_POINT('',#19026);
#3470=VERTEX_POINT('',#19028);
#3471=VERTEX_POINT('',#19030);
#3472=VERTEX_POINT('',#19032);
#3473=VERTEX_POINT('',#19034);
#3474=VERTEX_POINT('',#19036);
#3475=VERTEX_POINT('',#19038);
#3476=VERTEX_POINT('',#19040);
#3477=VERTEX_POINT('',#19042);
#3478=VERTEX_POINT('',#19044);
#3479=VERTEX_POINT('',#19046);
#3480=VERTEX_POINT('',#19048);
#3481=VERTEX_POINT('',#19050);
#3482=VERTEX_POINT('',#19052);
#3483=VERTEX_POINT('',#19054);
#3484=VERTEX_POINT('',#19056);
#3485=VERTEX_POINT('',#19058);
#3486=VERTEX_POINT('',#19060);
#3487=VERTEX_POINT('',#19062);
#3488=VERTEX_POINT('',#19064);
#3489=VERTEX_POINT('',#19066);
#3490=VERTEX_POINT('',#19068);
#3491=VERTEX_POINT('',#19070);
#3492=VERTEX_POINT('',#19072);
#3493=VERTEX_POINT('',#19074);
#3494=VERTEX_POINT('',#19076);
#3495=VERTEX_POINT('',#19078);
#3496=VERTEX_POINT('',#19080);
#3497=VERTEX_POINT('',#19082);
#3498=VERTEX_POINT('',#19084);
#3499=VERTEX_POINT('',#19086);
#3500=VERTEX_POINT('',#19088);
#3501=VERTEX_POINT('',#19090);
#3502=VERTEX_POINT('',#19092);
#3503=VERTEX_POINT('',#19094);
#3504=VERTEX_POINT('',#19096);
#3505=VERTEX_POINT('',#19098);
#3506=VERTEX_POINT('',#19100);
#3507=VERTEX_POINT('',#19102);
#3508=VERTEX_POINT('',#19104);
#3509=VERTEX_POINT('',#19106);
#3510=VERTEX_POINT('',#19108);
#3511=VERTEX_POINT('',#19110);
#3512=VERTEX_POINT('',#19112);
#3513=VERTEX_POINT('',#19114);
#3514=VERTEX_POINT('',#19116);
#3515=VERTEX_POINT('',#19118);
#3516=VERTEX_POINT('',#19120);
#3517=VERTEX_POINT('',#19122);
#3518=VERTEX_POINT('',#19124);
#3519=VERTEX_POINT('',#19126);
#3520=VERTEX_POINT('',#19128);
#3521=VERTEX_POINT('',#19130);
#3522=VERTEX_POINT('',#19132);
#3523=VERTEX_POINT('',#19134);
#3524=VERTEX_POINT('',#19136);
#3525=VERTEX_POINT('',#19138);
#3526=VERTEX_POINT('',#19140);
#3527=VERTEX_POINT('',#19142);
#3528=VERTEX_POINT('',#19144);
#3529=VERTEX_POINT('',#19146);
#3530=VERTEX_POINT('',#19148);
#3531=VERTEX_POINT('',#19150);
#3532=VERTEX_POINT('',#19152);
#3533=VERTEX_POINT('',#19154);
#3534=VERTEX_POINT('',#19156);
#3535=VERTEX_POINT('',#19158);
#3536=VERTEX_POINT('',#19160);
#3537=VERTEX_POINT('',#19162);
#3538=VERTEX_POINT('',#19164);
#3539=VERTEX_POINT('',#19166);
#3540=VERTEX_POINT('',#19168);
#3541=VERTEX_POINT('',#19170);
#3542=VERTEX_POINT('',#19172);
#3543=VERTEX_POINT('',#19175);
#3544=VERTEX_POINT('',#19176);
#3545=VERTEX_POINT('',#19178);
#3546=VERTEX_POINT('',#19180);
#3547=VERTEX_POINT('',#19182);
#3548=VERTEX_POINT('',#19184);
#3549=VERTEX_POINT('',#19188);
#3550=VERTEX_POINT('',#19190);
#3551=VERTEX_POINT('',#19194);
#3552=VERTEX_POINT('',#19198);
#3553=VERTEX_POINT('',#19202);
#3554=VERTEX_POINT('',#19206);
#3555=VERTEX_POINT('',#19212);
#3556=VERTEX_POINT('',#19215);
#3557=VERTEX_POINT('',#19219);
#3558=VERTEX_POINT('',#19220);
#3559=VERTEX_POINT('',#19222);
#3560=VERTEX_POINT('',#19224);
#3561=VERTEX_POINT('',#19226);
#3562=VERTEX_POINT('',#19228);
#3563=VERTEX_POINT('',#19230);
#3564=VERTEX_POINT('',#19232);
#3565=VERTEX_POINT('',#19234);
#3566=VERTEX_POINT('',#19236);
#3567=VERTEX_POINT('',#19238);
#3568=VERTEX_POINT('',#19240);
#3569=VERTEX_POINT('',#19242);
#3570=VERTEX_POINT('',#19244);
#3571=VERTEX_POINT('',#19246);
#3572=VERTEX_POINT('',#19248);
#3573=VERTEX_POINT('',#19250);
#3574=VERTEX_POINT('',#19252);
#3575=VERTEX_POINT('',#19254);
#3576=VERTEX_POINT('',#19256);
#3577=VERTEX_POINT('',#19258);
#3578=VERTEX_POINT('',#19260);
#3579=VERTEX_POINT('',#19262);
#3580=VERTEX_POINT('',#19264);
#3581=VERTEX_POINT('',#19266);
#3582=VERTEX_POINT('',#19268);
#3583=VERTEX_POINT('',#19270);
#3584=VERTEX_POINT('',#19272);
#3585=VERTEX_POINT('',#19274);
#3586=VERTEX_POINT('',#19276);
#3587=VERTEX_POINT('',#19278);
#3588=VERTEX_POINT('',#19280);
#3589=VERTEX_POINT('',#19282);
#3590=VERTEX_POINT('',#19284);
#3591=VERTEX_POINT('',#19286);
#3592=VERTEX_POINT('',#19288);
#3593=VERTEX_POINT('',#19290);
#3594=VERTEX_POINT('',#19292);
#3595=VERTEX_POINT('',#19294);
#3596=VERTEX_POINT('',#19296);
#3597=VERTEX_POINT('',#19298);
#3598=VERTEX_POINT('',#19300);
#3599=VERTEX_POINT('',#19302);
#3600=VERTEX_POINT('',#19304);
#3601=VERTEX_POINT('',#19306);
#3602=VERTEX_POINT('',#19308);
#3603=VERTEX_POINT('',#19310);
#3604=VERTEX_POINT('',#19312);
#3605=VERTEX_POINT('',#19314);
#3606=VERTEX_POINT('',#19316);
#3607=VERTEX_POINT('',#19318);
#3608=VERTEX_POINT('',#19320);
#3609=VERTEX_POINT('',#19322);
#3610=VERTEX_POINT('',#19324);
#3611=VERTEX_POINT('',#19326);
#3612=VERTEX_POINT('',#19328);
#3613=VERTEX_POINT('',#19330);
#3614=VERTEX_POINT('',#19332);
#3615=VERTEX_POINT('',#19334);
#3616=VERTEX_POINT('',#19336);
#3617=VERTEX_POINT('',#19338);
#3618=VERTEX_POINT('',#19340);
#3619=VERTEX_POINT('',#19342);
#3620=VERTEX_POINT('',#19344);
#3621=VERTEX_POINT('',#19346);
#3622=VERTEX_POINT('',#19348);
#3623=VERTEX_POINT('',#19350);
#3624=VERTEX_POINT('',#19352);
#3625=VERTEX_POINT('',#19354);
#3626=VERTEX_POINT('',#19356);
#3627=VERTEX_POINT('',#19358);
#3628=VERTEX_POINT('',#19360);
#3629=VERTEX_POINT('',#19362);
#3630=VERTEX_POINT('',#19364);
#3631=VERTEX_POINT('',#19366);
#3632=VERTEX_POINT('',#19368);
#3633=VERTEX_POINT('',#19370);
#3634=VERTEX_POINT('',#19372);
#3635=VERTEX_POINT('',#19374);
#3636=VERTEX_POINT('',#19376);
#3637=VERTEX_POINT('',#19378);
#3638=VERTEX_POINT('',#19380);
#3639=VERTEX_POINT('',#19382);
#3640=VERTEX_POINT('',#19384);
#3641=VERTEX_POINT('',#19386);
#3642=VERTEX_POINT('',#19388);
#3643=VERTEX_POINT('',#19390);
#3644=VERTEX_POINT('',#19392);
#3645=VERTEX_POINT('',#19394);
#3646=VERTEX_POINT('',#19396);
#3647=VERTEX_POINT('',#19398);
#3648=VERTEX_POINT('',#19400);
#3649=VERTEX_POINT('',#19402);
#3650=VERTEX_POINT('',#19404);
#3651=VERTEX_POINT('',#19406);
#3652=VERTEX_POINT('',#19408);
#3653=VERTEX_POINT('',#19462);
#3654=VERTEX_POINT('',#19463);
#3655=VERTEX_POINT('',#19477);
#3656=VERTEX_POINT('',#19479);
#3657=VERTEX_POINT('',#19505);
#3658=VERTEX_POINT('',#19506);
#3659=VERTEX_POINT('',#19521);
#3660=VERTEX_POINT('',#19522);
#3661=VERTEX_POINT('',#19549);
#3662=VERTEX_POINT('',#19550);
#3663=VERTEX_POINT('',#19564);
#3664=VERTEX_POINT('',#19566);
#3665=VERTEX_POINT('',#19592);
#3666=VERTEX_POINT('',#19593);
#3667=VERTEX_POINT('',#19607);
#3668=VERTEX_POINT('',#19609);
#3669=VERTEX_POINT('',#19635);
#3670=VERTEX_POINT('',#19636);
#3671=VERTEX_POINT('',#19650);
#3672=VERTEX_POINT('',#19652);
#3673=VERTEX_POINT('',#19678);
#3674=VERTEX_POINT('',#19679);
#3675=VERTEX_POINT('',#19693);
#3676=VERTEX_POINT('',#19695);
#3677=VERTEX_POINT('',#19721);
#3678=VERTEX_POINT('',#19722);
#3679=VERTEX_POINT('',#19736);
#3680=VERTEX_POINT('',#19738);
#3681=VERTEX_POINT('',#19764);
#3682=VERTEX_POINT('',#19765);
#3683=VERTEX_POINT('',#19779);
#3684=VERTEX_POINT('',#19781);
#3685=VERTEX_POINT('',#19807);
#3686=VERTEX_POINT('',#19808);
#3687=VERTEX_POINT('',#19822);
#3688=VERTEX_POINT('',#19824);
#3689=VERTEX_POINT('',#19850);
#3690=VERTEX_POINT('',#19851);
#3691=VERTEX_POINT('',#19865);
#3692=VERTEX_POINT('',#19867);
#3693=VERTEX_POINT('',#19893);
#3694=VERTEX_POINT('',#19894);
#3695=VERTEX_POINT('',#19908);
#3696=VERTEX_POINT('',#19910);
#3697=VERTEX_POINT('',#19936);
#3698=VERTEX_POINT('',#19937);
#3699=VERTEX_POINT('',#19951);
#3700=VERTEX_POINT('',#19953);
#3701=VERTEX_POINT('',#19979);
#3702=VERTEX_POINT('',#19980);
#3703=VERTEX_POINT('',#19994);
#3704=VERTEX_POINT('',#19996);
#3705=VERTEX_POINT('',#20022);
#3706=VERTEX_POINT('',#20023);
#3707=VERTEX_POINT('',#20037);
#3708=VERTEX_POINT('',#20039);
#3709=VERTEX_POINT('',#20065);
#3710=VERTEX_POINT('',#20066);
#3711=VERTEX_POINT('',#20080);
#3712=VERTEX_POINT('',#20082);
#3713=VERTEX_POINT('',#20108);
#3714=VERTEX_POINT('',#20109);
#3715=VERTEX_POINT('',#20124);
#3716=VERTEX_POINT('',#20125);
#3717=VERTEX_POINT('',#20151);
#3718=VERTEX_POINT('',#20153);
#3719=VERTEX_POINT('',#20154);
#3720=VERTEX_POINT('',#20156);
#3721=VERTEX_POINT('',#20158);
#3722=VERTEX_POINT('',#20160);
#3723=VERTEX_POINT('',#20162);
#3724=VERTEX_POINT('',#20166);
#3725=VERTEX_POINT('',#20170);
#3726=VERTEX_POINT('',#20172);
#3727=VERTEX_POINT('',#20177);
#3728=VERTEX_POINT('',#20224);
#3729=VERTEX_POINT('',#20225);
#3730=VERTEX_POINT('',#20280);
#3731=VERTEX_POINT('',#20285);
#3732=VERTEX_POINT('',#20287);
#3733=VERTEX_POINT('',#20291);
#3734=VERTEX_POINT('',#20295);
#3735=VERTEX_POINT('',#20299);
#3736=VERTEX_POINT('',#20303);
#3737=VERTEX_POINT('',#20309);
#3738=VERTEX_POINT('',#20310);
#3739=VERTEX_POINT('',#20315);
#3740=VERTEX_POINT('',#20317);
#3741=VERTEX_POINT('',#20319);
#3742=VERTEX_POINT('',#20330);
#3743=VERTEX_POINT('',#20400);
#3744=VERTEX_POINT('',#20554);
#3745=VERTEX_POINT('',#20755);
#3746=VERTEX_POINT('',#21021);
#3747=VERTEX_POINT('',#21074);
#3748=VERTEX_POINT('',#21611);
#3749=VERTEX_POINT('',#21612);
#3750=VERTEX_POINT('',#21998);
#3751=VERTEX_POINT('',#21999);
#3752=VERTEX_POINT('',#22385);
#3753=VERTEX_POINT('',#22386);
#3754=VERTEX_POINT('',#22772);
#3755=VERTEX_POINT('',#22773);
#3756=VERTEX_POINT('',#23025);
#3757=VERTEX_POINT('',#23026);
#3758=VERTEX_POINT('',#23028);
#3759=VERTEX_POINT('',#23043);
#3760=VERTEX_POINT('',#23054);
#3761=VERTEX_POINT('',#23200);
#3762=VERTEX_POINT('',#23587);
#3763=VERTEX_POINT('',#23781);
#3764=VERTEX_POINT('',#23966);
#3765=VERTEX_POINT('',#24299);
#3766=VERTEX_POINT('',#24625);
#3767=VERTEX_POINT('',#25140);
#3768=VERTEX_POINT('',#25142);
#3769=VERTEX_POINT('',#25145);
#3770=VERTEX_POINT('',#25149);
#3771=VERTEX_POINT('',#25155);
#3772=VERTEX_POINT('',#25156);
#3773=VERTEX_POINT('',#25158);
#3774=VERTEX_POINT('',#25177);
#3775=VERTEX_POINT('',#25178);
#3776=VERTEX_POINT('',#25200);
#3777=VERTEX_POINT('',#25202);
#3778=VERTEX_POINT('',#25204);
#3779=VERTEX_POINT('',#25362);
#3780=VERTEX_POINT('',#25761);
#3781=VERTEX_POINT('',#26021);
#3782=VERTEX_POINT('',#26023);
#3783=VERTEX_POINT('',#26025);
#3784=VERTEX_POINT('',#26068);
#3785=VERTEX_POINT('',#26517);
#3786=VERTEX_POINT('',#26648);
#3787=VERTEX_POINT('',#26908);
#3788=VERTEX_POINT('',#27168);
#3789=VERTEX_POINT('',#27352);
#3790=VERTEX_POINT('',#27483);
#3791=VERTEX_POINT('',#27743);
#3792=VERTEX_POINT('',#28003);
#3793=VERTEX_POINT('',#28187);
#3794=VERTEX_POINT('',#28304);
#3795=VERTEX_POINT('',#28309);
#3796=VERTEX_POINT('',#28324);
#3797=VERTEX_POINT('',#28589);
#3798=VERTEX_POINT('',#28590);
#3799=VERTEX_POINT('',#28639);
#3800=VERTEX_POINT('',#28765);
#3801=VERTEX_POINT('',#28768);
#3802=VERTEX_POINT('',#28921);
#3803=VERTEX_POINT('',#28924);
#3804=VERTEX_POINT('',#28926);
#3805=VERTEX_POINT('',#28956);
#3806=VERTEX_POINT('',#28957);
#3807=VERTEX_POINT('',#28964);
#3808=VERTEX_POINT('',#28980);
#3809=VERTEX_POINT('',#28985);
#3810=VERTEX_POINT('',#28987);
#3811=VERTEX_POINT('',#28992);
#3812=VERTEX_POINT('',#29008);
#3813=VERTEX_POINT('',#29013);
#3814=VERTEX_POINT('',#29015);
#3815=VERTEX_POINT('',#29031);
#3816=VERTEX_POINT('',#29036);
#3817=VERTEX_POINT('',#29038);
#3818=VERTEX_POINT('',#29043);
#3819=VERTEX_POINT('',#29059);
#3820=VERTEX_POINT('',#29066);
#3821=VERTEX_POINT('',#29082);
#3822=VERTEX_POINT('',#29087);
#3823=VERTEX_POINT('',#29089);
#3824=VERTEX_POINT('',#29094);
#3825=VERTEX_POINT('',#29110);
#3826=VERTEX_POINT('',#29112);
#3827=VERTEX_POINT('',#29128);
#3828=VERTEX_POINT('',#29133);
#3829=VERTEX_POINT('',#29135);
#3830=VERTEX_POINT('',#29156);
#3831=VERTEX_POINT('',#29158);
#3832=VERTEX_POINT('',#29162);
#3833=VERTEX_POINT('',#29166);
#3834=VERTEX_POINT('',#29167);
#3835=VERTEX_POINT('',#29169);
#3836=VERTEX_POINT('',#29171);
#3837=VERTEX_POINT('',#29173);
#3838=VERTEX_POINT('',#29175);
#3839=VERTEX_POINT('',#29177);
#3840=VERTEX_POINT('',#29179);
#3841=VERTEX_POINT('',#29182);
#3842=VERTEX_POINT('',#29184);
#3843=VERTEX_POINT('',#29186);
#3844=VERTEX_POINT('',#29188);
#3845=VERTEX_POINT('',#29190);
#3846=VERTEX_POINT('',#29192);
#3847=VERTEX_POINT('',#29194);
#3848=VERTEX_POINT('',#29196);
#3849=VERTEX_POINT('',#29198);
#3850=VERTEX_POINT('',#29200);
#3851=VERTEX_POINT('',#29202);
#3852=VERTEX_POINT('',#29204);
#3853=VERTEX_POINT('',#29206);
#3854=VERTEX_POINT('',#29210);
#3855=VERTEX_POINT('',#29215);
#3856=VERTEX_POINT('',#29217);
#3857=VERTEX_POINT('',#29221);
#3858=VERTEX_POINT('',#29223);
#3859=VERTEX_POINT('',#29227);
#3860=VERTEX_POINT('',#29229);
#3861=VERTEX_POINT('',#29233);
#3862=VERTEX_POINT('',#29278);
#3863=VERTEX_POINT('',#29279);
#3864=VERTEX_POINT('',#29281);
#3865=VERTEX_POINT('',#29313);
#3866=VERTEX_POINT('',#29315);
#3867=VERTEX_POINT('',#29350);
#3868=VERTEX_POINT('',#29352);
#3869=VERTEX_POINT('',#29361);
#3870=VERTEX_POINT('',#29363);
#3871=VERTEX_POINT('',#29370);
#3872=VERTEX_POINT('',#29377);
#3873=VERTEX_POINT('',#29387);
#3874=VERTEX_POINT('',#29388);
#3875=VERTEX_POINT('',#29393);
#3876=VERTEX_POINT('',#29394);
#3877=VERTEX_POINT('',#29396);
#3878=VERTEX_POINT('',#29400);
#3879=VERTEX_POINT('',#29401);
#3880=VERTEX_POINT('',#29403);
#3881=VERTEX_POINT('',#29407);
#3882=VERTEX_POINT('',#29411);
#3883=VERTEX_POINT('',#29412);
#3884=VERTEX_POINT('',#29414);
#3885=VERTEX_POINT('',#29418);
#3886=VERTEX_POINT('',#29420);
#3887=VERTEX_POINT('',#29467);
#3888=VERTEX_POINT('',#29505);
#3889=VERTEX_POINT('',#29517);
#3890=VERTEX_POINT('',#29519);
#3891=VERTEX_POINT('',#29558);
#3892=VERTEX_POINT('',#29590);
#3893=VERTEX_POINT('',#29624);
#3894=VERTEX_POINT('',#29626);
#3895=VERTEX_POINT('',#29665);
#3896=VERTEX_POINT('',#29700);
#3897=VERTEX_POINT('',#29702);
#3898=VERTEX_POINT('',#29739);
#3899=VERTEX_POINT('',#29759);
#3900=VERTEX_POINT('',#29761);
#3901=VERTEX_POINT('',#29796);
#3902=VERTEX_POINT('',#29798);
#3903=VERTEX_POINT('',#29800);
#3904=VERTEX_POINT('',#29802);
#3905=VERTEX_POINT('',#29933);
#3906=VERTEX_POINT('',#29942);
#3907=VERTEX_POINT('',#29943);
#3908=VERTEX_POINT('',#30005);
#3909=VERTEX_POINT('',#30031);
#3910=VERTEX_POINT('',#30093);
#3911=VERTEX_POINT('',#30122);
#3912=VERTEX_POINT('',#30153);
#3913=VERTEX_POINT('',#30215);
#3914=VERTEX_POINT('',#30217);
#3915=VERTEX_POINT('',#30246);
#3916=VERTEX_POINT('',#30334);
#3917=VERTEX_POINT('',#30336);
#3918=VERTEX_POINT('',#30368);
#3919=VERTEX_POINT('',#30407);
#3920=VERTEX_POINT('',#30408);
#3921=VERTEX_POINT('',#30440);
#3922=VERTEX_POINT('',#30447);
#3923=VERTEX_POINT('',#30449);
#3924=VERTEX_POINT('',#30451);
#3925=VERTEX_POINT('',#30565);
#3926=VERTEX_POINT('',#30707);
#3927=VERTEX_POINT('',#30709);
#3928=VERTEX_POINT('',#30768);
#3929=VERTEX_POINT('',#30832);
#3930=VERTEX_POINT('',#30909);
#3931=VERTEX_POINT('',#31062);
#3932=VERTEX_POINT('',#31101);
#3933=VERTEX_POINT('',#31136);
#3934=VERTEX_POINT('',#31179);
#3935=VERTEX_POINT('',#31220);
#3936=VERTEX_POINT('',#31239);
#3937=VERTEX_POINT('',#31324);
#3938=VERTEX_POINT('',#31326);
#3939=VERTEX_POINT('',#31400);
#3940=VERTEX_POINT('',#31451);
#3941=VERTEX_POINT('',#31456);
#3942=VERTEX_POINT('',#31458);
#3943=VERTEX_POINT('',#31527);
#3944=VERTEX_POINT('',#31808);
#3945=VERTEX_POINT('',#31956);
#3946=VERTEX_POINT('',#31961);
#3947=VERTEX_POINT('',#32088);
#3948=VERTEX_POINT('',#32090);
#3949=VERTEX_POINT('',#32160);
#3950=VERTEX_POINT('',#32162);
#3951=VERTEX_POINT('',#32203);
#3952=VERTEX_POINT('',#32205);
#3953=VERTEX_POINT('',#32213);
#3954=VERTEX_POINT('',#32353);
#3955=VERTEX_POINT('',#32400);
#3956=VERTEX_POINT('',#32404);
#3957=VERTEX_POINT('',#32439);
#3958=VERTEX_POINT('',#32443);
#3959=VERTEX_POINT('',#32453);
#3960=VERTEX_POINT('',#32485);
#3961=VERTEX_POINT('',#32493);
#3962=VERTEX_POINT('',#32633);
#3963=VERTEX_POINT('',#32647);
#3964=VERTEX_POINT('',#32705);
#3965=VERTEX_POINT('',#32748);
#3966=VERTEX_POINT('',#32899);
#3967=VERTEX_POINT('',#32903);
#3968=VERTEX_POINT('',#32975);
#3969=VERTEX_POINT('',#33006);
#3970=VERTEX_POINT('',#33198);
#3971=VERTEX_POINT('',#33394);
#3972=VERTEX_POINT('',#33589);
#3973=VERTEX_POINT('',#33590);
#3974=VERTEX_POINT('',#33605);
#3975=VERTEX_POINT('',#33616);
#3976=VERTEX_POINT('',#33643);
#3977=VERTEX_POINT('',#33649);
#3978=VERTEX_POINT('',#33650);
#3979=VERTEX_POINT('',#33655);
#3980=VERTEX_POINT('',#33659);
#3981=VERTEX_POINT('',#33662);
#3982=VERTEX_POINT('',#34529);
#3983=VERTEX_POINT('',#34531);
#3984=VERTEX_POINT('',#34532);
#3985=VERTEX_POINT('',#34534);
#3986=VERTEX_POINT('',#34536);
#3987=VERTEX_POINT('',#34538);
#3988=VERTEX_POINT('',#34540);
#3989=VERTEX_POINT('',#34542);
#3990=VERTEX_POINT('',#34544);
#3991=VERTEX_POINT('',#34546);
#3992=VERTEX_POINT('',#34548);
#3993=VERTEX_POINT('',#34550);
#3994=VERTEX_POINT('',#34552);
#3995=VERTEX_POINT('',#34554);
#3996=VERTEX_POINT('',#34556);
#3997=VERTEX_POINT('',#34558);
#3998=VERTEX_POINT('',#34560);
#3999=VERTEX_POINT('',#34562);
#4000=VERTEX_POINT('',#34564);
#4001=VERTEX_POINT('',#34566);
#4002=VERTEX_POINT('',#34568);
#4003=VERTEX_POINT('',#34570);
#4004=VERTEX_POINT('',#34572);
#4005=VERTEX_POINT('',#34574);
#4006=VERTEX_POINT('',#34576);
#4007=VERTEX_POINT('',#34580);
#4008=VERTEX_POINT('',#34584);
#4009=VERTEX_POINT('',#34588);
#4010=VERTEX_POINT('',#34590);
#4011=VERTEX_POINT('',#34594);
#4012=VERTEX_POINT('',#34595);
#4013=VERTEX_POINT('',#34600);
#4014=VERTEX_POINT('',#34605);
#4015=VERTEX_POINT('',#34821);
#4016=VERTEX_POINT('',#34940);
#4017=VERTEX_POINT('',#34942);
#4018=VERTEX_POINT('',#35203);
#4019=VERTEX_POINT('',#35248);
#4020=VERTEX_POINT('',#35255);
#4021=VERTEX_POINT('',#35511);
#4022=VERTEX_POINT('',#35630);
#4023=VERTEX_POINT('',#35886);
#4024=VERTEX_POINT('',#35931);
#4025=VERTEX_POINT('',#36187);
#4026=VERTEX_POINT('',#36304);
#4027=VERTEX_POINT('',#36560);
#4028=VERTEX_POINT('',#36605);
#4029=VERTEX_POINT('',#36861);
#4030=VERTEX_POINT('',#36982);
#4031=VERTEX_POINT('',#37238);
#4032=VERTEX_POINT('',#37285);
#4033=VERTEX_POINT('',#37541);
#4034=VERTEX_POINT('',#37656);
#4035=VERTEX_POINT('',#37912);
#4036=VERTEX_POINT('',#37957);
#4037=VERTEX_POINT('',#38213);
#4038=VERTEX_POINT('',#38312);
#4039=VERTEX_POINT('',#38339);
#4040=VERTEX_POINT('',#38692);
#4041=VERTEX_POINT('',#39802);
#4042=VERTEX_POINT('',#39804);
#4043=VERTEX_POINT('',#39808);
#4044=VERTEX_POINT('',#39812);
#4045=VERTEX_POINT('',#39813);
#4046=VERTEX_POINT('',#39815);
#4047=VERTEX_POINT('',#39817);
#4048=VERTEX_POINT('',#39819);
#4049=VERTEX_POINT('',#39822);
#4050=VERTEX_POINT('',#39824);
#4051=VERTEX_POINT('',#39826);
#4052=VERTEX_POINT('',#39828);
#4053=VERTEX_POINT('',#39830);
#4054=VERTEX_POINT('',#39832);
#4055=VERTEX_POINT('',#39834);
#4056=VERTEX_POINT('',#39836);
#4057=VERTEX_POINT('',#39838);
#4058=VERTEX_POINT('',#39840);
#4059=VERTEX_POINT('',#39842);
#4060=VERTEX_POINT('',#39844);
#4061=VERTEX_POINT('',#39846);
#4062=VERTEX_POINT('',#39848);
#4063=VERTEX_POINT('',#39850);
#4064=VERTEX_POINT('',#39852);
#4065=VERTEX_POINT('',#39900);
#4066=VERTEX_POINT('',#39901);
#4067=VERTEX_POINT('',#39903);
#4068=VERTEX_POINT('',#39905);
#4069=VERTEX_POINT('',#39907);
#4070=VERTEX_POINT('',#39919);
#4071=VERTEX_POINT('',#39922);
#4072=VERTEX_POINT('',#39925);
#4073=VERTEX_POINT('',#39926);
#4074=VERTEX_POINT('',#39931);
#4075=VERTEX_POINT('',#39935);
#4076=VERTEX_POINT('',#39938);
#4077=VERTEX_POINT('',#39939);
#4078=VERTEX_POINT('',#39944);
#4079=VERTEX_POINT('',#39946);
#4080=VERTEX_POINT('',#39948);
#4081=VERTEX_POINT('',#39969);
#4082=VERTEX_POINT('',#40066);
#4083=VERTEX_POINT('',#40081);
#4084=VERTEX_POINT('',#40275);
#4085=VERTEX_POINT('',#40326);
#4086=VERTEX_POINT('',#40328);
#4087=VERTEX_POINT('',#40337);
#4088=VERTEX_POINT('',#40444);
#4089=VERTEX_POINT('',#40473);
#4090=VERTEX_POINT('',#40512);
#4091=VERTEX_POINT('',#40801);
#4092=VERTEX_POINT('',#40912);
#4093=VERTEX_POINT('',#41164);
#4094=VERTEX_POINT('',#41486);
#4095=VERTEX_POINT('',#41738);
#4096=VERTEX_POINT('',#41917);
#4097=VERTEX_POINT('',#42028);
#4098=VERTEX_POINT('',#42280);
#4099=VERTEX_POINT('',#42532);
#4100=VERTEX_POINT('',#42967);
#4101=VERTEX_POINT('',#43373);
#4102=VERTEX_POINT('',#43376);
#4103=VERTEX_POINT('',#43379);
#4104=VERTEX_POINT('',#43380);
#4105=VERTEX_POINT('',#43427);
#4106=VERTEX_POINT('',#43430);
#4107=VERTEX_POINT('',#43434);
#4108=VERTEX_POINT('',#43435);
#4109=VERTEX_POINT('',#43599);
#4110=VERTEX_POINT('',#43601);
#4111=VERTEX_POINT('',#43612);
#4112=VERTEX_POINT('',#43622);
#4113=VERTEX_POINT('',#43631);
#4114=VERTEX_POINT('',#43633);
#4115=VERTEX_POINT('',#43635);
#4116=VERTEX_POINT('',#43637);
#4117=VERTEX_POINT('',#43639);
#4118=VERTEX_POINT('',#43641);
#4119=VERTEX_POINT('',#43643);
#4120=VERTEX_POINT('',#43645);
#4121=VERTEX_POINT('',#43647);
#4122=VERTEX_POINT('',#43650);
#4123=VERTEX_POINT('',#43653);
#4124=VERTEX_POINT('',#43657);
#4125=VERTEX_POINT('',#43658);
#4126=VERTEX_POINT('',#43660);
#4127=VERTEX_POINT('',#43662);
#4128=VERTEX_POINT('',#43666);
#4129=VERTEX_POINT('',#43668);
#4130=VERTEX_POINT('',#43821);
#4131=VERTEX_POINT('',#43823);
#4132=VERTEX_POINT('',#43840);
#4133=VERTEX_POINT('',#43903);
#4134=VERTEX_POINT('',#43904);
#4135=VERTEX_POINT('',#44050);
#4136=VERTEX_POINT('',#44051);
#4137=VERTEX_POINT('',#44059);
#4138=VERTEX_POINT('',#44063);
#4139=VERTEX_POINT('',#44071);
#4140=VERTEX_POINT('',#44077);
#4141=VERTEX_POINT('',#44083);
#4142=VERTEX_POINT('',#44089);
#4143=VERTEX_POINT('',#44093);
#4144=VERTEX_POINT('',#44095);
#4145=VERTEX_POINT('',#44097);
#4146=VERTEX_POINT('',#44103);
#4147=VERTEX_POINT('',#44107);
#4148=VERTEX_POINT('',#44109);
#4149=VERTEX_POINT('',#44135);
#4150=VERTEX_POINT('',#44249);
#4151=VERTEX_POINT('',#44368);
#4152=VERTEX_POINT('',#44370);
#4153=VERTEX_POINT('',#44472);
#4154=VERTEX_POINT('',#44498);
#4155=VERTEX_POINT('',#44533);
#4156=VERTEX_POINT('',#44542);
#4157=VERTEX_POINT('',#44544);
#4158=VERTEX_POINT('',#44546);
#4159=VERTEX_POINT('',#44548);
#4160=VERTEX_POINT('',#44559);
#4161=VERTEX_POINT('',#44594);
#4162=VERTEX_POINT('',#44753);
#4163=VERTEX_POINT('',#44883);
#4164=VERTEX_POINT('',#44972);
#4165=VERTEX_POINT('',#44974);
#4166=VERTEX_POINT('',#45112);
#4167=VERTEX_POINT('',#45182);
#4168=VERTEX_POINT('',#45194);
#4169=VERTEX_POINT('',#45195);
#4170=VERTEX_POINT('',#45201);
#4171=VERTEX_POINT('',#45203);
#4172=VERTEX_POINT('',#45206);
#4173=VERTEX_POINT('',#45209);
#4174=VERTEX_POINT('',#45213);
#4175=VERTEX_POINT('',#45216);
#4176=VERTEX_POINT('',#45221);
#4177=VERTEX_POINT('',#45222);
#4178=VERTEX_POINT('',#45224);
#4179=VERTEX_POINT('',#45226);
#4180=VERTEX_POINT('',#45228);
#4181=VERTEX_POINT('',#45230);
#4182=VERTEX_POINT('',#45239);
#4183=VERTEX_POINT('',#45324);
#4184=VERTEX_POINT('',#45431);
#4185=VERTEX_POINT('',#45513);
#4186=VERTEX_POINT('',#45531);
#4187=VERTEX_POINT('',#45537);
#4188=VERTEX_POINT('',#45647);
#4189=VERTEX_POINT('',#45709);
#4190=VERTEX_POINT('',#45745);
#4191=VERTEX_POINT('',#45888);
#4192=VERTEX_POINT('',#46031);
#4193=VERTEX_POINT('',#46049);
#4194=VERTEX_POINT('',#46051);
#4195=VERTEX_POINT('',#46054);
#4196=VERTEX_POINT('',#46058);
#4197=VERTEX_POINT('',#46064);
#4198=VERTEX_POINT('',#46065);
#4199=VERTEX_POINT('',#46070);
#4200=VERTEX_POINT('',#46165);
#4201=VERTEX_POINT('',#46170);
#4202=VERTEX_POINT('',#46201);
#4203=VERTEX_POINT('',#46204);
#4204=VERTEX_POINT('',#46208);
#4205=VERTEX_POINT('',#46237);
#4206=VERTEX_POINT('',#46238);
#4207=VERTEX_POINT('',#46249);
#4208=VERTEX_POINT('',#46261);
#4209=VERTEX_POINT('',#46272);
#4210=VERTEX_POINT('',#46284);
#4211=VERTEX_POINT('',#46295);
#4212=VERTEX_POINT('',#46307);
#4213=VERTEX_POINT('',#46318);
#4214=VERTEX_POINT('',#46330);
#4215=VERTEX_POINT('',#46341);
#4216=VERTEX_POINT('',#46351);
#4217=VERTEX_POINT('',#46358);
#4218=VERTEX_POINT('',#46381);
#4219=VERTEX_POINT('',#46382);
#4220=VERTEX_POINT('',#46387);
#4221=VERTEX_POINT('',#46389);
#4222=VERTEX_POINT('',#46391);
#4223=VERTEX_POINT('',#46393);
#4224=VERTEX_POINT('',#46395);
#4225=VERTEX_POINT('',#46397);
#4226=VERTEX_POINT('',#46399);
#4227=VERTEX_POINT('',#46401);
#4228=VERTEX_POINT('',#46403);
#4229=VERTEX_POINT('',#46405);
#4230=VERTEX_POINT('',#46408);
#4231=VERTEX_POINT('',#46411);
#4232=VERTEX_POINT('',#46413);
#4233=VERTEX_POINT('',#46440);
#4234=VERTEX_POINT('',#46489);
#4235=VERTEX_POINT('',#46496);
#4236=VERTEX_POINT('',#46777);
#4237=VERTEX_POINT('',#46778);
#4238=VERTEX_POINT('',#47011);
#4239=VERTEX_POINT('',#47894);
#4240=VERTEX_POINT('',#48061);
#4241=VERTEX_POINT('',#48063);
#4242=VERTEX_POINT('',#48946);
#4243=VERTEX_POINT('',#49011);
#4244=VERTEX_POINT('',#52082);
#4245=VERTEX_POINT('',#52087);
#4246=VERTEX_POINT('',#52089);
#4247=VERTEX_POINT('',#52092);
#4248=VERTEX_POINT('',#52096);
#4249=VERTEX_POINT('',#52102);
#4250=VERTEX_POINT('',#52104);
#4251=VERTEX_POINT('',#52107);
#4252=VERTEX_POINT('',#52111);
#4253=VERTEX_POINT('',#52114);
#4254=VERTEX_POINT('',#52115);
#4255=VERTEX_POINT('',#52120);
#4256=EDGE_CURVE('',#3392,#3393,#2462,.T.);
#4257=EDGE_CURVE('',#3392,#3394,#2094,.T.);
#4258=EDGE_CURVE('',#3394,#3395,#2463,.T.);
#4259=EDGE_CURVE('',#3395,#3395,#1627,.T.);
#4260=EDGE_CURVE('',#3394,#3393,#2464,.T.);
#4261=EDGE_CURVE('',#3396,#3397,#2465,.T.);
#4262=EDGE_CURVE('',#3396,#3392,#2095,.T.);
#4263=EDGE_CURVE('',#3393,#3397,#2096,.T.);
#4264=EDGE_CURVE('',#3398,#3399,#2466,.T.);
#4265=EDGE_CURVE('',#3398,#3400,#2097,.T.);
#4266=EDGE_CURVE('',#3400,#3396,#2098,.T.);
#4267=EDGE_CURVE('',#3397,#3399,#2099,.T.);
#4268=EDGE_CURVE('',#3401,#3402,#2467,.T.);
#4269=EDGE_CURVE('',#3401,#3398,#2100,.T.);
#4270=EDGE_CURVE('',#3399,#3403,#2101,.T.);
#4271=EDGE_CURVE('',#3403,#3402,#2102,.T.);
#4272=EDGE_CURVE('',#3404,#3405,#2468,.T.);
#4273=EDGE_CURVE('',#3404,#3401,#2103,.T.);
#4274=EDGE_CURVE('',#3402,#3405,#2104,.T.);
#4275=EDGE_CURVE('',#3406,#3394,#2105,.T.);
#4276=EDGE_CURVE('',#3407,#3406,#2106,.T.);
#4277=EDGE_CURVE('',#3408,#3407,#2107,.T.);
#4278=EDGE_CURVE('',#3393,#3408,#2108,.T.);
#4279=EDGE_CURVE('',#3405,#3409,#2109,.T.);
#4280=EDGE_CURVE('',#3410,#3409,#2469,.T.);
#4281=EDGE_CURVE('',#3410,#3410,#1628,.T.);
#4282=EDGE_CURVE('',#3404,#3409,#2470,.T.);
#4283=EDGE_CURVE('',#3408,#3411,#2110,.T.);
#4284=EDGE_CURVE('',#3403,#3411,#2471,.T.);
#4285=EDGE_CURVE('',#3411,#3412,#2111,.T.);
#4286=EDGE_CURVE('',#3409,#3412,#2112,.T.);
#4287=EDGE_CURVE('',#3412,#3413,#2113,.T.);
#4288=EDGE_CURVE('',#3413,#3414,#2114,.T.);
#4289=EDGE_CURVE('',#3414,#3404,#2115,.T.);
#4290=EDGE_CURVE('',#3415,#3414,#2116,.T.);
#4291=EDGE_CURVE('',#3415,#3400,#2472,.T.);
#4292=EDGE_CURVE('',#3406,#3415,#2117,.T.);
#4293=EDGE_CURVE('',#3416,#3415,#2473,.T.);
#4294=EDGE_CURVE('',#3407,#3416,#2118,.T.);
#4295=EDGE_CURVE('',#3411,#3416,#2474,.T.);
#4296=EDGE_CURVE('',#3416,#3413,#2119,.T.);
#4297=EDGE_CURVE('',#3417,#3418,#1629,.T.);
#4298=EDGE_CURVE('',#3418,#3419,#2475,.T.);
#4299=EDGE_CURVE('',#3420,#3419,#2120,.T.);
#4300=EDGE_CURVE('',#3420,#3417,#2121,.T.);
#4301=EDGE_CURVE('',#3421,#3417,#2122,.T.);
#4302=EDGE_CURVE('',#3418,#3421,#2476,.T.);
#4303=EDGE_CURVE('',#3422,#3421,#2123,.T.);
#4304=EDGE_CURVE('',#3423,#3422,#2124,.T.);
#4305=EDGE_CURVE('',#3419,#3423,#2125,.T.);
#4306=EDGE_CURVE('',#3423,#3424,#2126,.T.);
#4307=EDGE_CURVE('',#3425,#3424,#2477,.T.);
#4308=EDGE_CURVE('',#3421,#3425,#2127,.F.);
#4309=EDGE_CURVE('',#3425,#3426,#2128,.T.);
#4310=EDGE_CURVE('',#3427,#3426,#2478,.T.);
#4311=EDGE_CURVE('',#3422,#3427,#2129,.T.);
#4312=EDGE_CURVE('',#3424,#3427,#2479,.T.);
#4313=EDGE_CURVE('',#3427,#3428,#2130,.T.);
#4314=EDGE_CURVE('',#3429,#3428,#2480,.T.);
#4315=EDGE_CURVE('',#3424,#3429,#2131,.T.);
#4316=EDGE_CURVE('',#3426,#3430,#2132,.F.);
#4317=EDGE_CURVE('',#3430,#3429,#2481,.T.);
#4318=EDGE_CURVE('',#3430,#3431,#2133,.T.);
#4319=EDGE_CURVE('',#3428,#3431,#2482,.T.);
#4320=EDGE_CURVE('',#3431,#3432,#2134,.T.);
#4321=EDGE_CURVE('',#3432,#3433,#2135,.T.);
#4322=EDGE_CURVE('',#3434,#3433,#2483,.T.);
#4323=EDGE_CURVE('',#3428,#3434,#2136,.T.);
#4324=EDGE_CURVE('',#3429,#3435,#2137,.T.);
#4325=EDGE_CURVE('',#3432,#3435,#2484,.T.);
#4326=EDGE_CURVE('',#3435,#3436,#2138,.T.);
#4327=EDGE_CURVE('',#3436,#3437,#2139,.T.);
#4328=EDGE_CURVE('',#3438,#3437,#2140,.T.);
#4329=EDGE_CURVE('',#3433,#3438,#2141,.F.);
#4330=EDGE_CURVE('',#3439,#3440,#2142,.T.);
#4331=EDGE_CURVE('',#3434,#3440,#2143,.T.);
#4332=EDGE_CURVE('',#3438,#3439,#2144,.T.);
#4333=EDGE_CURVE('',#3441,#3437,#2485,.T.);
#4334=EDGE_CURVE('',#3442,#3436,#2145,.T.);
#4335=EDGE_CURVE('',#3440,#3442,#2146,.T.);
#4336=EDGE_CURVE('',#3439,#3441,#1630,.T.);
#4337=EDGE_CURVE('',#3441,#3438,#2486,.T.);
#4338=EDGE_CURVE('',#3435,#3434,#2487,.T.);
#4339=EDGE_CURVE('',#3443,#3443,#1631,.T.);
#4340=EDGE_CURVE('',#3444,#3445,#1632,.T.);
#4341=EDGE_CURVE('',#3445,#3444,#1633,.T.);
#4342=EDGE_CURVE('',#3445,#3443,#2488,.T.);
#4343=EDGE_CURVE('',#3446,#3444,#1634,.T.);
#4344=EDGE_CURVE('',#3447,#3448,#1635,.T.);
#4345=EDGE_CURVE('',#3448,#3449,#1636,.T.);
#4346=EDGE_CURVE('',#3449,#3450,#1637,.T.);
#4347=EDGE_CURVE('',#3450,#3451,#1638,.T.);
#4348=EDGE_CURVE('',#3451,#3452,#1639,.T.);
#4349=EDGE_CURVE('',#3452,#3453,#1640,.T.);
#4350=EDGE_CURVE('',#3453,#3454,#1641,.T.);
#4351=EDGE_CURVE('',#3454,#3455,#1642,.T.);
#4352=EDGE_CURVE('',#3455,#3456,#1643,.T.);
#4353=EDGE_CURVE('',#3456,#3457,#1644,.T.);
#4354=EDGE_CURVE('',#3457,#3458,#1645,.T.);
#4355=EDGE_CURVE('',#3458,#3459,#1646,.T.);
#4356=EDGE_CURVE('',#3459,#3460,#1647,.T.);
#4357=EDGE_CURVE('',#3460,#3461,#1648,.T.);
#4358=EDGE_CURVE('',#3461,#3462,#1649,.T.);
#4359=EDGE_CURVE('',#3462,#3463,#1650,.T.);
#4360=EDGE_CURVE('',#3463,#3464,#1651,.T.);
#4361=EDGE_CURVE('',#3464,#3465,#1652,.T.);
#4362=EDGE_CURVE('',#3465,#3466,#1653,.T.);
#4363=EDGE_CURVE('',#3466,#3467,#1654,.T.);
#4364=EDGE_CURVE('',#3467,#3468,#1655,.T.);
#4365=EDGE_CURVE('',#3468,#3469,#1656,.T.);
#4366=EDGE_CURVE('',#3469,#3470,#1657,.T.);
#4367=EDGE_CURVE('',#3470,#3471,#1658,.T.);
#4368=EDGE_CURVE('',#3471,#3472,#1659,.T.);
#4369=EDGE_CURVE('',#3472,#3473,#1660,.T.);
#4370=EDGE_CURVE('',#3473,#3474,#1661,.T.);
#4371=EDGE_CURVE('',#3474,#3475,#1662,.T.);
#4372=EDGE_CURVE('',#3475,#3476,#1663,.T.);
#4373=EDGE_CURVE('',#3476,#3477,#1664,.T.);
#4374=EDGE_CURVE('',#3477,#3478,#1665,.T.);
#4375=EDGE_CURVE('',#3478,#3479,#1666,.T.);
#4376=EDGE_CURVE('',#3479,#3480,#1667,.T.);
#4377=EDGE_CURVE('',#3480,#3481,#1668,.T.);
#4378=EDGE_CURVE('',#3481,#3482,#1669,.T.);
#4379=EDGE_CURVE('',#3482,#3483,#1670,.T.);
#4380=EDGE_CURVE('',#3483,#3484,#1671,.T.);
#4381=EDGE_CURVE('',#3484,#3485,#1672,.T.);
#4382=EDGE_CURVE('',#3485,#3486,#1673,.T.);
#4383=EDGE_CURVE('',#3486,#3487,#1674,.T.);
#4384=EDGE_CURVE('',#3487,#3488,#1675,.T.);
#4385=EDGE_CURVE('',#3488,#3489,#1676,.T.);
#4386=EDGE_CURVE('',#3489,#3490,#1677,.T.);
#4387=EDGE_CURVE('',#3490,#3491,#1678,.T.);
#4388=EDGE_CURVE('',#3491,#3492,#1679,.T.);
#4389=EDGE_CURVE('',#3492,#3493,#1680,.T.);
#4390=EDGE_CURVE('',#3493,#3494,#1681,.T.);
#4391=EDGE_CURVE('',#3494,#3495,#1682,.T.);
#4392=EDGE_CURVE('',#3495,#3496,#1683,.T.);
#4393=EDGE_CURVE('',#3496,#3497,#1684,.T.);
#4394=EDGE_CURVE('',#3497,#3498,#1685,.T.);
#4395=EDGE_CURVE('',#3498,#3499,#1686,.T.);
#4396=EDGE_CURVE('',#3499,#3500,#1687,.T.);
#4397=EDGE_CURVE('',#3500,#3501,#1688,.T.);
#4398=EDGE_CURVE('',#3501,#3502,#1689,.T.);
#4399=EDGE_CURVE('',#3502,#3503,#1690,.T.);
#4400=EDGE_CURVE('',#3503,#3504,#1691,.T.);
#4401=EDGE_CURVE('',#3504,#3505,#1692,.T.);
#4402=EDGE_CURVE('',#3505,#3506,#1693,.T.);
#4403=EDGE_CURVE('',#3506,#3507,#1694,.T.);
#4404=EDGE_CURVE('',#3507,#3508,#1695,.T.);
#4405=EDGE_CURVE('',#3508,#3509,#1696,.T.);
#4406=EDGE_CURVE('',#3509,#3510,#1697,.T.);
#4407=EDGE_CURVE('',#3510,#3511,#1698,.T.);
#4408=EDGE_CURVE('',#3511,#3512,#1699,.T.);
#4409=EDGE_CURVE('',#3512,#3513,#1700,.T.);
#4410=EDGE_CURVE('',#3513,#3514,#1701,.T.);
#4411=EDGE_CURVE('',#3514,#3515,#1702,.T.);
#4412=EDGE_CURVE('',#3515,#3516,#1703,.T.);
#4413=EDGE_CURVE('',#3516,#3517,#1704,.T.);
#4414=EDGE_CURVE('',#3517,#3518,#1705,.T.);
#4415=EDGE_CURVE('',#3518,#3519,#1706,.T.);
#4416=EDGE_CURVE('',#3519,#3520,#1707,.T.);
#4417=EDGE_CURVE('',#3520,#3521,#1708,.T.);
#4418=EDGE_CURVE('',#3521,#3522,#1709,.T.);
#4419=EDGE_CURVE('',#3522,#3523,#1710,.T.);
#4420=EDGE_CURVE('',#3523,#3524,#1711,.T.);
#4421=EDGE_CURVE('',#3524,#3525,#1712,.T.);
#4422=EDGE_CURVE('',#3525,#3526,#1713,.T.);
#4423=EDGE_CURVE('',#3526,#3527,#1714,.T.);
#4424=EDGE_CURVE('',#3527,#3528,#1715,.T.);
#4425=EDGE_CURVE('',#3528,#3529,#1716,.T.);
#4426=EDGE_CURVE('',#3529,#3530,#1717,.T.);
#4427=EDGE_CURVE('',#3530,#3531,#1718,.T.);
#4428=EDGE_CURVE('',#3531,#3532,#1719,.T.);
#4429=EDGE_CURVE('',#3532,#3533,#1720,.T.);
#4430=EDGE_CURVE('',#3533,#3534,#1721,.T.);
#4431=EDGE_CURVE('',#3534,#3535,#1722,.T.);
#4432=EDGE_CURVE('',#3535,#3536,#1723,.T.);
#4433=EDGE_CURVE('',#3536,#3537,#1724,.T.);
#4434=EDGE_CURVE('',#3537,#3538,#1725,.T.);
#4435=EDGE_CURVE('',#3538,#3539,#1726,.T.);
#4436=EDGE_CURVE('',#3539,#3540,#1727,.T.);
#4437=EDGE_CURVE('',#3540,#3541,#1728,.T.);
#4438=EDGE_CURVE('',#3541,#3542,#1729,.T.);
#4439=EDGE_CURVE('',#3542,#3447,#1730,.T.);
#4440=EDGE_CURVE('',#3543,#3544,#2489,.T.);
#4441=EDGE_CURVE('',#3545,#3543,#2490,.T.);
#4442=EDGE_CURVE('',#3546,#3545,#2491,.T.);
#4443=EDGE_CURVE('',#3547,#3546,#2492,.T.);
#4444=EDGE_CURVE('',#3548,#3547,#2493,.T.);
#4445=EDGE_CURVE('',#3544,#3548,#2494,.T.);
#4446=EDGE_CURVE('',#3544,#3549,#2495,.T.);
#4447=EDGE_CURVE('',#3550,#3549,#2496,.T.);
#4448=EDGE_CURVE('',#3543,#3550,#2497,.T.);
#4449=EDGE_CURVE('',#3551,#3550,#2498,.T.);
#4450=EDGE_CURVE('',#3545,#3551,#2499,.T.);
#4451=EDGE_CURVE('',#3552,#3551,#2500,.T.);
#4452=EDGE_CURVE('',#3546,#3552,#2501,.T.);
#4453=EDGE_CURVE('',#3553,#3552,#2502,.T.);
#4454=EDGE_CURVE('',#3547,#3553,#2503,.T.);
#4455=EDGE_CURVE('',#3554,#3553,#2504,.T.);
#4456=EDGE_CURVE('',#3548,#3554,#2505,.T.);
#4457=EDGE_CURVE('',#3549,#3554,#2506,.T.);
#4458=EDGE_CURVE('',#3555,#3555,#1731,.T.);
#4459=EDGE_CURVE('',#3555,#3556,#2507,.T.);
#4460=EDGE_CURVE('',#3556,#3556,#1732,.T.);
#4461=EDGE_CURVE('',#3557,#3558,#1733,.T.);
#4462=EDGE_CURVE('',#3559,#3558,#1734,.T.);
#4463=EDGE_CURVE('',#3560,#3559,#1735,.T.);
#4464=EDGE_CURVE('',#3561,#3560,#1736,.T.);
#4465=EDGE_CURVE('',#3562,#3561,#1737,.T.);
#4466=EDGE_CURVE('',#3563,#3562,#1738,.T.);
#4467=EDGE_CURVE('',#3563,#3564,#1739,.T.);
#4468=EDGE_CURVE('',#3565,#3564,#1740,.T.);
#4469=EDGE_CURVE('',#3566,#3565,#1741,.T.);
#4470=EDGE_CURVE('',#3567,#3566,#1742,.T.);
#4471=EDGE_CURVE('',#3568,#3567,#1743,.T.);
#4472=EDGE_CURVE('',#3569,#3568,#1744,.T.);
#4473=EDGE_CURVE('',#3569,#3570,#1745,.T.);
#4474=EDGE_CURVE('',#3571,#3570,#1746,.T.);
#4475=EDGE_CURVE('',#3572,#3571,#1747,.T.);
#4476=EDGE_CURVE('',#3573,#3572,#1748,.T.);
#4477=EDGE_CURVE('',#3574,#3573,#1749,.T.);
#4478=EDGE_CURVE('',#3575,#3574,#1750,.T.);
#4479=EDGE_CURVE('',#3575,#3576,#1751,.T.);
#4480=EDGE_CURVE('',#3577,#3576,#1752,.T.);
#4481=EDGE_CURVE('',#3578,#3577,#1753,.T.);
#4482=EDGE_CURVE('',#3579,#3578,#1754,.T.);
#4483=EDGE_CURVE('',#3580,#3579,#1755,.T.);
#4484=EDGE_CURVE('',#3581,#3580,#1756,.T.);
#4485=EDGE_CURVE('',#3581,#3582,#1757,.T.);
#4486=EDGE_CURVE('',#3583,#3582,#1758,.T.);
#4487=EDGE_CURVE('',#3584,#3583,#1759,.T.);
#4488=EDGE_CURVE('',#3585,#3584,#1760,.T.);
#4489=EDGE_CURVE('',#3586,#3585,#1761,.T.);
#4490=EDGE_CURVE('',#3587,#3586,#1762,.T.);
#4491=EDGE_CURVE('',#3587,#3588,#1763,.T.);
#4492=EDGE_CURVE('',#3589,#3588,#1764,.T.);
#4493=EDGE_CURVE('',#3590,#3589,#1765,.T.);
#4494=EDGE_CURVE('',#3591,#3590,#1766,.T.);
#4495=EDGE_CURVE('',#3592,#3591,#1767,.T.);
#4496=EDGE_CURVE('',#3593,#3592,#1768,.T.);
#4497=EDGE_CURVE('',#3593,#3594,#1769,.T.);
#4498=EDGE_CURVE('',#3595,#3594,#1770,.T.);
#4499=EDGE_CURVE('',#3596,#3595,#1771,.T.);
#4500=EDGE_CURVE('',#3597,#3596,#1772,.T.);
#4501=EDGE_CURVE('',#3598,#3597,#1773,.T.);
#4502=EDGE_CURVE('',#3599,#3598,#1774,.T.);
#4503=EDGE_CURVE('',#3599,#3600,#1775,.T.);
#4504=EDGE_CURVE('',#3601,#3600,#1776,.T.);
#4505=EDGE_CURVE('',#3602,#3601,#1777,.T.);
#4506=EDGE_CURVE('',#3603,#3602,#1778,.T.);
#4507=EDGE_CURVE('',#3604,#3603,#1779,.T.);
#4508=EDGE_CURVE('',#3605,#3604,#1780,.T.);
#4509=EDGE_CURVE('',#3605,#3606,#1781,.T.);
#4510=EDGE_CURVE('',#3607,#3606,#1782,.T.);
#4511=EDGE_CURVE('',#3608,#3607,#1783,.T.);
#4512=EDGE_CURVE('',#3609,#3608,#1784,.T.);
#4513=EDGE_CURVE('',#3610,#3609,#1785,.T.);
#4514=EDGE_CURVE('',#3611,#3610,#1786,.T.);
#4515=EDGE_CURVE('',#3611,#3612,#1787,.T.);
#4516=EDGE_CURVE('',#3613,#3612,#1788,.T.);
#4517=EDGE_CURVE('',#3614,#3613,#1789,.T.);
#4518=EDGE_CURVE('',#3615,#3614,#1790,.T.);
#4519=EDGE_CURVE('',#3616,#3615,#1791,.T.);
#4520=EDGE_CURVE('',#3617,#3616,#1792,.T.);
#4521=EDGE_CURVE('',#3617,#3618,#1793,.T.);
#4522=EDGE_CURVE('',#3619,#3618,#1794,.T.);
#4523=EDGE_CURVE('',#3620,#3619,#1795,.T.);
#4524=EDGE_CURVE('',#3621,#3620,#1796,.T.);
#4525=EDGE_CURVE('',#3622,#3621,#1797,.T.);
#4526=EDGE_CURVE('',#3623,#3622,#1798,.T.);
#4527=EDGE_CURVE('',#3623,#3624,#1799,.T.);
#4528=EDGE_CURVE('',#3625,#3624,#1800,.T.);
#4529=EDGE_CURVE('',#3626,#3625,#1801,.T.);
#4530=EDGE_CURVE('',#3627,#3626,#1802,.T.);
#4531=EDGE_CURVE('',#3628,#3627,#1803,.T.);
#4532=EDGE_CURVE('',#3629,#3628,#1804,.T.);
#4533=EDGE_CURVE('',#3629,#3630,#1805,.T.);
#4534=EDGE_CURVE('',#3631,#3630,#1806,.T.);
#4535=EDGE_CURVE('',#3632,#3631,#1807,.T.);
#4536=EDGE_CURVE('',#3633,#3632,#1808,.T.);
#4537=EDGE_CURVE('',#3634,#3633,#1809,.T.);
#4538=EDGE_CURVE('',#3635,#3634,#1810,.T.);
#4539=EDGE_CURVE('',#3635,#3636,#1811,.T.);
#4540=EDGE_CURVE('',#3637,#3636,#1812,.T.);
#4541=EDGE_CURVE('',#3638,#3637,#1813,.T.);
#4542=EDGE_CURVE('',#3639,#3638,#1814,.T.);
#4543=EDGE_CURVE('',#3640,#3639,#1815,.T.);
#4544=EDGE_CURVE('',#3641,#3640,#1816,.T.);
#4545=EDGE_CURVE('',#3641,#3642,#1817,.T.);
#4546=EDGE_CURVE('',#3643,#3642,#1818,.T.);
#4547=EDGE_CURVE('',#3644,#3643,#1819,.T.);
#4548=EDGE_CURVE('',#3645,#3644,#1820,.T.);
#4549=EDGE_CURVE('',#3646,#3645,#1821,.T.);
#4550=EDGE_CURVE('',#3647,#3646,#1822,.T.);
#4551=EDGE_CURVE('',#3647,#3648,#1823,.T.);
#4552=EDGE_CURVE('',#3649,#3648,#1824,.T.);
#4553=EDGE_CURVE('',#3650,#3649,#1825,.T.);
#4554=EDGE_CURVE('',#3651,#3650,#1826,.T.);
#4555=EDGE_CURVE('',#3652,#3651,#1827,.T.);
#4556=EDGE_CURVE('',#3557,#3652,#1828,.T.);
#4557=EDGE_CURVE('',#3564,#3531,#2508,.T.);
#4558=EDGE_CURVE('',#3563,#3532,#2509,.T.);
#4559=EDGE_CURVE('',#3570,#3525,#2510,.T.);
#4560=EDGE_CURVE('',#3569,#3526,#2511,.T.);
#4561=EDGE_CURVE('',#3576,#3519,#2512,.T.);
#4562=EDGE_CURVE('',#3575,#3520,#2513,.T.);
#4563=EDGE_CURVE('',#3582,#3513,#2514,.T.);
#4564=EDGE_CURVE('',#3581,#3514,#2515,.T.);
#4565=EDGE_CURVE('',#3588,#3507,#2516,.T.);
#4566=EDGE_CURVE('',#3587,#3508,#2517,.T.);
#4567=EDGE_CURVE('',#3594,#3501,#2518,.T.);
#4568=EDGE_CURVE('',#3593,#3502,#2519,.T.);
#4569=EDGE_CURVE('',#3600,#3495,#2520,.T.);
#4570=EDGE_CURVE('',#3599,#3496,#2521,.T.);
#4571=EDGE_CURVE('',#3606,#3489,#2522,.T.);
#4572=EDGE_CURVE('',#3605,#3490,#2523,.T.);
#4573=EDGE_CURVE('',#3612,#3483,#2524,.T.);
#4574=EDGE_CURVE('',#3611,#3484,#2525,.T.);
#4575=EDGE_CURVE('',#3618,#3477,#2526,.T.);
#4576=EDGE_CURVE('',#3617,#3478,#2527,.T.);
#4577=EDGE_CURVE('',#3624,#3471,#2528,.T.);
#4578=EDGE_CURVE('',#3623,#3472,#2529,.T.);
#4579=EDGE_CURVE('',#3630,#3465,#2530,.T.);
#4580=EDGE_CURVE('',#3629,#3466,#2531,.T.);
#4581=EDGE_CURVE('',#3636,#3459,#2532,.T.);
#4582=EDGE_CURVE('',#3635,#3460,#2533,.T.);
#4583=EDGE_CURVE('',#3642,#3453,#2534,.T.);
#4584=EDGE_CURVE('',#3641,#3454,#2535,.T.);
#4585=EDGE_CURVE('',#3557,#3538,#2536,.T.);
#4586=EDGE_CURVE('',#3558,#3537,#2537,.T.);
#4587=EDGE_CURVE('',#3648,#3447,#2538,.T.);
#4588=EDGE_CURVE('',#3647,#3448,#2539,.T.);
#4589=EDGE_CURVE('',#3530,#3565,#2540,.T.);
#4590=EDGE_CURVE('',#3653,#3654,#2147,.T.);
#4591=EDGE_CURVE('',#3654,#3566,#2541,.T.);
#4592=EDGE_CURVE('',#3529,#3653,#2542,.T.);
#4593=EDGE_CURVE('',#3655,#3653,#1829,.T.);
#4594=EDGE_CURVE('',#3656,#3655,#2148,.T.);
#4595=EDGE_CURVE('',#3654,#3656,#1830,.T.);
#4596=EDGE_CURVE('',#3528,#3655,#2543,.T.);
#4597=EDGE_CURVE('',#3656,#3567,#2544,.T.);
#4598=EDGE_CURVE('',#3527,#3568,#2545,.T.);
#4599=EDGE_CURVE('',#3533,#3562,#2546,.T.);
#4600=EDGE_CURVE('',#3657,#3658,#2149,.T.);
#4601=EDGE_CURVE('',#3534,#3658,#2547,.T.);
#4602=EDGE_CURVE('',#3657,#3561,#2548,.T.);
#4603=EDGE_CURVE('',#3659,#3660,#2150,.T.);
#4604=EDGE_CURVE('',#3658,#3659,#1831,.T.);
#4605=EDGE_CURVE('',#3660,#3657,#1832,.T.);
#4606=EDGE_CURVE('',#3660,#3560,#2549,.T.);
#4607=EDGE_CURVE('',#3536,#3559,#2550,.T.);
#4608=EDGE_CURVE('',#3535,#3659,#2551,.T.);
#4609=EDGE_CURVE('',#3524,#3571,#2552,.T.);
#4610=EDGE_CURVE('',#3661,#3662,#2151,.T.);
#4611=EDGE_CURVE('',#3662,#3572,#2553,.T.);
#4612=EDGE_CURVE('',#3523,#3661,#2554,.T.);
#4613=EDGE_CURVE('',#3663,#3661,#1833,.T.);
#4614=EDGE_CURVE('',#3664,#3663,#2152,.T.);
#4615=EDGE_CURVE('',#3662,#3664,#1834,.T.);
#4616=EDGE_CURVE('',#3522,#3663,#2555,.T.);
#4617=EDGE_CURVE('',#3664,#3573,#2556,.T.);
#4618=EDGE_CURVE('',#3521,#3574,#2557,.T.);
#4619=EDGE_CURVE('',#3518,#3577,#2558,.T.);
#4620=EDGE_CURVE('',#3665,#3666,#2153,.T.);
#4621=EDGE_CURVE('',#3666,#3578,#2559,.T.);
#4622=EDGE_CURVE('',#3517,#3665,#2560,.T.);
#4623=EDGE_CURVE('',#3667,#3665,#1835,.T.);
#4624=EDGE_CURVE('',#3668,#3667,#2154,.T.);
#4625=EDGE_CURVE('',#3666,#3668,#1836,.T.);
#4626=EDGE_CURVE('',#3516,#3667,#2561,.T.);
#4627=EDGE_CURVE('',#3668,#3579,#2562,.T.);
#4628=EDGE_CURVE('',#3515,#3580,#2563,.T.);
#4629=EDGE_CURVE('',#3512,#3583,#2564,.T.);
#4630=EDGE_CURVE('',#3669,#3670,#2155,.T.);
#4631=EDGE_CURVE('',#3670,#3584,#2565,.T.);
#4632=EDGE_CURVE('',#3511,#3669,#2566,.T.);
#4633=EDGE_CURVE('',#3671,#3669,#1837,.T.);
#4634=EDGE_CURVE('',#3672,#3671,#2156,.T.);
#4635=EDGE_CURVE('',#3670,#3672,#1838,.T.);
#4636=EDGE_CURVE('',#3510,#3671,#2567,.T.);
#4637=EDGE_CURVE('',#3672,#3585,#2568,.T.);
#4638=EDGE_CURVE('',#3509,#3586,#2569,.T.);
#4639=EDGE_CURVE('',#3506,#3589,#2570,.T.);
#4640=EDGE_CURVE('',#3673,#3674,#2157,.T.);
#4641=EDGE_CURVE('',#3674,#3590,#2571,.T.);
#4642=EDGE_CURVE('',#3505,#3673,#2572,.T.);
#4643=EDGE_CURVE('',#3675,#3673,#1839,.T.);
#4644=EDGE_CURVE('',#3676,#3675,#2158,.T.);
#4645=EDGE_CURVE('',#3674,#3676,#1840,.T.);
#4646=EDGE_CURVE('',#3504,#3675,#2573,.T.);
#4647=EDGE_CURVE('',#3676,#3591,#2574,.T.);
#4648=EDGE_CURVE('',#3503,#3592,#2575,.T.);
#4649=EDGE_CURVE('',#3500,#3595,#2576,.T.);
#4650=EDGE_CURVE('',#3677,#3678,#2159,.T.);
#4651=EDGE_CURVE('',#3678,#3596,#2577,.T.);
#4652=EDGE_CURVE('',#3499,#3677,#2578,.T.);
#4653=EDGE_CURVE('',#3679,#3677,#1841,.T.);
#4654=EDGE_CURVE('',#3680,#3679,#2160,.T.);
#4655=EDGE_CURVE('',#3678,#3680,#1842,.T.);
#4656=EDGE_CURVE('',#3498,#3679,#2579,.T.);
#4657=EDGE_CURVE('',#3680,#3597,#2580,.T.);
#4658=EDGE_CURVE('',#3497,#3598,#2581,.T.);
#4659=EDGE_CURVE('',#3494,#3601,#2582,.T.);
#4660=EDGE_CURVE('',#3681,#3682,#2161,.T.);
#4661=EDGE_CURVE('',#3682,#3602,#2583,.T.);
#4662=EDGE_CURVE('',#3493,#3681,#2584,.T.);
#4663=EDGE_CURVE('',#3683,#3681,#1843,.T.);
#4664=EDGE_CURVE('',#3684,#3683,#2162,.T.);
#4665=EDGE_CURVE('',#3682,#3684,#1844,.T.);
#4666=EDGE_CURVE('',#3492,#3683,#2585,.T.);
#4667=EDGE_CURVE('',#3684,#3603,#2586,.T.);
#4668=EDGE_CURVE('',#3491,#3604,#2587,.T.);
#4669=EDGE_CURVE('',#3488,#3607,#2588,.T.);
#4670=EDGE_CURVE('',#3685,#3686,#2163,.T.);
#4671=EDGE_CURVE('',#3686,#3608,#2589,.T.);
#4672=EDGE_CURVE('',#3487,#3685,#2590,.T.);
#4673=EDGE_CURVE('',#3687,#3685,#1845,.T.);
#4674=EDGE_CURVE('',#3688,#3687,#2164,.T.);
#4675=EDGE_CURVE('',#3686,#3688,#1846,.T.);
#4676=EDGE_CURVE('',#3486,#3687,#2591,.T.);
#4677=EDGE_CURVE('',#3688,#3609,#2592,.T.);
#4678=EDGE_CURVE('',#3485,#3610,#2593,.T.);
#4679=EDGE_CURVE('',#3482,#3613,#2594,.T.);
#4680=EDGE_CURVE('',#3689,#3690,#2165,.T.);
#4681=EDGE_CURVE('',#3690,#3614,#2595,.T.);
#4682=EDGE_CURVE('',#3481,#3689,#2596,.T.);
#4683=EDGE_CURVE('',#3691,#3689,#1847,.T.);
#4684=EDGE_CURVE('',#3692,#3691,#2166,.T.);
#4685=EDGE_CURVE('',#3690,#3692,#1848,.T.);
#4686=EDGE_CURVE('',#3480,#3691,#2597,.T.);
#4687=EDGE_CURVE('',#3692,#3615,#2598,.T.);
#4688=EDGE_CURVE('',#3479,#3616,#2599,.T.);
#4689=EDGE_CURVE('',#3476,#3619,#2600,.T.);
#4690=EDGE_CURVE('',#3693,#3694,#2167,.T.);
#4691=EDGE_CURVE('',#3694,#3620,#2601,.T.);
#4692=EDGE_CURVE('',#3475,#3693,#2602,.T.);
#4693=EDGE_CURVE('',#3695,#3693,#1849,.T.);
#4694=EDGE_CURVE('',#3696,#3695,#2168,.T.);
#4695=EDGE_CURVE('',#3694,#3696,#1850,.T.);
#4696=EDGE_CURVE('',#3474,#3695,#2603,.T.);
#4697=EDGE_CURVE('',#3696,#3621,#2604,.T.);
#4698=EDGE_CURVE('',#3473,#3622,#2605,.T.);
#4699=EDGE_CURVE('',#3470,#3625,#2606,.T.);
#4700=EDGE_CURVE('',#3697,#3698,#2169,.T.);
#4701=EDGE_CURVE('',#3698,#3626,#2607,.T.);
#4702=EDGE_CURVE('',#3469,#3697,#2608,.T.);
#4703=EDGE_CURVE('',#3699,#3697,#1851,.T.);
#4704=EDGE_CURVE('',#3700,#3699,#2170,.T.);
#4705=EDGE_CURVE('',#3698,#3700,#1852,.T.);
#4706=EDGE_CURVE('',#3468,#3699,#2609,.T.);
#4707=EDGE_CURVE('',#3700,#3627,#2610,.T.);
#4708=EDGE_CURVE('',#3467,#3628,#2611,.T.);
#4709=EDGE_CURVE('',#3464,#3631,#2612,.T.);
#4710=EDGE_CURVE('',#3701,#3702,#2171,.T.);
#4711=EDGE_CURVE('',#3702,#3632,#2613,.T.);
#4712=EDGE_CURVE('',#3463,#3701,#2614,.T.);
#4713=EDGE_CURVE('',#3703,#3701,#1853,.T.);
#4714=EDGE_CURVE('',#3704,#3703,#2172,.T.);
#4715=EDGE_CURVE('',#3702,#3704,#1854,.T.);
#4716=EDGE_CURVE('',#3462,#3703,#2615,.T.);
#4717=EDGE_CURVE('',#3704,#3633,#2616,.T.);
#4718=EDGE_CURVE('',#3461,#3634,#2617,.T.);
#4719=EDGE_CURVE('',#3458,#3637,#2618,.T.);
#4720=EDGE_CURVE('',#3705,#3706,#2173,.T.);
#4721=EDGE_CURVE('',#3706,#3638,#2619,.T.);
#4722=EDGE_CURVE('',#3457,#3705,#2620,.T.);
#4723=EDGE_CURVE('',#3707,#3705,#1855,.T.);
#4724=EDGE_CURVE('',#3708,#3707,#2174,.T.);
#4725=EDGE_CURVE('',#3706,#3708,#1856,.T.);
#4726=EDGE_CURVE('',#3456,#3707,#2621,.T.);
#4727=EDGE_CURVE('',#3708,#3639,#2622,.T.);
#4728=EDGE_CURVE('',#3455,#3640,#2623,.T.);
#4729=EDGE_CURVE('',#3452,#3643,#2624,.T.);
#4730=EDGE_CURVE('',#3709,#3710,#2175,.T.);
#4731=EDGE_CURVE('',#3710,#3644,#2625,.T.);
#4732=EDGE_CURVE('',#3451,#3709,#2626,.T.);
#4733=EDGE_CURVE('',#3711,#3709,#1857,.T.);
#4734=EDGE_CURVE('',#3712,#3711,#2176,.T.);
#4735=EDGE_CURVE('',#3710,#3712,#1858,.T.);
#4736=EDGE_CURVE('',#3450,#3711,#2627,.T.);
#4737=EDGE_CURVE('',#3712,#3645,#2628,.T.);
#4738=EDGE_CURVE('',#3449,#3646,#2629,.T.);
#4739=EDGE_CURVE('',#3539,#3652,#2630,.T.);
#4740=EDGE_CURVE('',#3713,#3714,#2177,.T.);
#4741=EDGE_CURVE('',#3540,#3714,#2631,.T.);
#4742=EDGE_CURVE('',#3713,#3651,#2632,.T.);
#4743=EDGE_CURVE('',#3715,#3716,#2178,.T.);
#4744=EDGE_CURVE('',#3714,#3715,#1859,.T.);
#4745=EDGE_CURVE('',#3716,#3713,#1860,.T.);
#4746=EDGE_CURVE('',#3716,#3650,#2633,.T.);
#4747=EDGE_CURVE('',#3542,#3649,#2634,.T.);
#4748=EDGE_CURVE('',#3541,#3715,#2635,.T.);
#4749=EDGE_CURVE('',#3717,#3717,#1861,.T.);
#4750=EDGE_CURVE('',#3718,#3719,#2636,.T.);
#4751=EDGE_CURVE('',#3720,#3718,#2637,.T.);
#4752=EDGE_CURVE('',#3721,#3720,#2638,.T.);
#4753=EDGE_CURVE('',#3722,#3721,#2639,.T.);
#4754=EDGE_CURVE('',#3723,#3722,#2640,.T.);
#4755=EDGE_CURVE('',#3719,#3723,#2641,.T.);
#4756=EDGE_CURVE('',#3717,#3724,#2642,.T.);
#4757=EDGE_CURVE('',#3724,#3724,#1862,.T.);
#4758=EDGE_CURVE('',#3725,#3725,#1863,.T.);
#4759=EDGE_CURVE('',#3725,#3726,#2643,.T.);
#4760=EDGE_CURVE('',#3726,#3726,#1864,.T.);
#4761=EDGE_CURVE('',#3724,#3725,#1865,.T.);
#4762=EDGE_CURVE('',#3727,#3727,#2179,.T.);
#4763=EDGE_CURVE('',#3728,#3729,#2180,.T.);
#4764=EDGE_CURVE('',#3729,#3728,#2181,.T.);
#4765=EDGE_CURVE('',#3726,#3730,#1866,.T.);
#4766=EDGE_CURVE('',#3729,#3727,#2644,.T.);
#4767=EDGE_CURVE('',#3719,#3731,#2645,.T.);
#4768=EDGE_CURVE('',#3732,#3731,#2646,.T.);
#4769=EDGE_CURVE('',#3718,#3732,#2647,.T.);
#4770=EDGE_CURVE('',#3733,#3732,#2648,.T.);
#4771=EDGE_CURVE('',#3720,#3733,#2649,.T.);
#4772=EDGE_CURVE('',#3734,#3733,#2650,.T.);
#4773=EDGE_CURVE('',#3721,#3734,#2651,.T.);
#4774=EDGE_CURVE('',#3735,#3734,#2652,.T.);
#4775=EDGE_CURVE('',#3722,#3735,#2653,.T.);
#4776=EDGE_CURVE('',#3736,#3735,#2654,.T.);
#4777=EDGE_CURVE('',#3723,#3736,#2655,.T.);
#4778=EDGE_CURVE('',#3731,#3736,#2656,.T.);
#4779=EDGE_CURVE('',#3737,#3738,#2182,.T.);
#4780=EDGE_CURVE('',#3739,#3737,#1867,.T.);
#4781=EDGE_CURVE('',#3739,#3740,#2657,.T.);
#4782=EDGE_CURVE('',#3741,#3740,#2183,.T.);
#4783=EDGE_CURVE('',#3742,#3741,#2184,.T.);
#4784=EDGE_CURVE('',#3738,#3742,#2185,.T.);
#4785=EDGE_CURVE('',#3743,#3737,#2186,.T.);
#4786=EDGE_CURVE('',#3743,#3739,#2658,.T.);
#4787=EDGE_CURVE('',#3744,#3742,#2187,.T.);
#4788=EDGE_CURVE('',#3744,#3745,#2659,.T.);
#4789=EDGE_CURVE('',#3745,#3743,#2188,.T.);
#4790=EDGE_CURVE('',#3743,#3740,#2189,.T.);
#4791=EDGE_CURVE('',#3745,#3746,#2190,.T.);
#4792=EDGE_CURVE('',#3746,#3747,#2660,.T.);
#4793=EDGE_CURVE('',#3747,#3741,#2191,.T.);
#4794=EDGE_CURVE('',#3747,#3744,#2661,.T.);
#4795=EDGE_CURVE('',#3748,#3749,#2662,.T.);
#4796=EDGE_CURVE('',#3749,#3744,#2192,.T.);
#4797=EDGE_CURVE('',#3748,#3747,#2193,.T.);
#4798=EDGE_CURVE('',#3750,#3751,#2663,.T.);
#4799=EDGE_CURVE('',#3751,#3749,#2194,.T.);
#4800=EDGE_CURVE('',#3750,#3748,#2195,.T.);
#4801=EDGE_CURVE('',#3752,#3753,#2664,.T.);
#4802=EDGE_CURVE('',#3753,#3751,#2196,.T.);
#4803=EDGE_CURVE('',#3752,#3750,#2197,.T.);
#4804=EDGE_CURVE('',#3754,#3755,#2198,.T.);
#4805=EDGE_CURVE('',#3755,#3753,#2199,.T.);
#4806=EDGE_CURVE('',#3754,#3752,#2200,.T.);
#4807=EDGE_CURVE('',#3756,#3757,#2665,.T.);
#4808=EDGE_CURVE('',#3756,#3758,#2666,.T.);
#4809=EDGE_CURVE('',#3755,#3758,#2201,.T.);
#4810=EDGE_CURVE('',#3757,#3754,#2202,.T.);
#4811=EDGE_CURVE('',#3759,#3757,#2203,.T.);
#4812=EDGE_CURVE('',#3759,#3760,#2204,.T.);
#4813=EDGE_CURVE('',#3760,#3756,#1868,.T.);
#4814=EDGE_CURVE('',#3761,#3752,#2667,.T.);
#4815=EDGE_CURVE('',#3758,#3761,#2205,.F.);
#4816=EDGE_CURVE('',#3758,#3760,#2206,.T.);
#4817=EDGE_CURVE('',#3761,#3762,#2207,.T.);
#4818=EDGE_CURVE('',#3753,#3762,#2668,.T.);
#4819=EDGE_CURVE('',#3762,#3763,#2208,.T.);
#4820=EDGE_CURVE('',#3763,#3764,#2209,.T.);
#4821=EDGE_CURVE('',#3751,#3764,#2669,.T.);
#4822=EDGE_CURVE('',#3763,#3750,#2670,.T.);
#4823=EDGE_CURVE('',#3765,#3748,#2671,.T.);
#4824=EDGE_CURVE('',#3764,#3765,#2210,.F.);
#4825=EDGE_CURVE('',#3765,#3766,#2211,.T.);
#4826=EDGE_CURVE('',#3749,#3766,#2672,.T.);
#4827=EDGE_CURVE('',#3766,#3746,#2212,.T.);
#4828=EDGE_CURVE('',#3767,#3767,#1869,.T.);
#4829=EDGE_CURVE('',#3768,#3768,#1870,.T.);
#4830=EDGE_CURVE('',#3768,#3769,#2673,.T.);
#4831=EDGE_CURVE('',#3769,#3769,#1871,.T.);
#4832=EDGE_CURVE('',#3770,#3770,#1872,.T.);
#4833=EDGE_CURVE('',#3770,#3767,#1873,.T.);
#4834=EDGE_CURVE('',#3771,#3772,#2674,.T.);
#4835=EDGE_CURVE('',#3773,#3771,#2213,.T.);
#4836=EDGE_CURVE('',#3773,#3772,#1874,.T.);
#4837=EDGE_CURVE('',#3774,#3775,#1875,.T.);
#4838=EDGE_CURVE('',#3775,#3774,#2214,.T.);
#4839=EDGE_CURVE('',#3776,#3774,#2675,.T.);
#4840=EDGE_CURVE('',#3776,#3777,#1876,.T.);
#4841=EDGE_CURVE('',#3778,#3777,#2215,.T.);
#4842=EDGE_CURVE('',#3775,#3778,#2216,.T.);
#4843=EDGE_CURVE('',#3778,#3779,#2217,.T.);
#4844=EDGE_CURVE('',#3779,#3780,#2676,.T.);
#4845=EDGE_CURVE('',#3776,#3780,#2218,.T.);
#4846=EDGE_CURVE('',#3781,#3776,#2677,.T.);
#4847=EDGE_CURVE('',#3780,#3782,#2678,.T.);
#4848=EDGE_CURVE('',#3782,#3783,#2219,.T.);
#4849=EDGE_CURVE('',#3784,#3783,#2220,.F.);
#4850=EDGE_CURVE('',#3781,#3784,#2221,.T.);
#4851=EDGE_CURVE('',#3777,#3781,#2222,.T.);
#4852=EDGE_CURVE('',#3783,#3779,#2679,.T.);
#4853=EDGE_CURVE('',#3782,#3785,#2223,.T.);
#4854=EDGE_CURVE('',#3785,#3786,#2680,.T.);
#4855=EDGE_CURVE('',#3779,#3786,#2224,.T.);
#4856=EDGE_CURVE('',#3786,#3787,#2681,.T.);
#4857=EDGE_CURVE('',#3780,#3787,#2225,.T.);
#4858=EDGE_CURVE('',#3787,#3788,#2682,.T.);
#4859=EDGE_CURVE('',#3788,#3785,#2226,.T.);
#4860=EDGE_CURVE('',#3788,#3789,#2227,.T.);
#4861=EDGE_CURVE('',#3789,#3790,#2683,.T.);
#4862=EDGE_CURVE('',#3786,#3790,#2228,.T.);
#4863=EDGE_CURVE('',#3790,#3791,#2684,.T.);
#4864=EDGE_CURVE('',#3787,#3791,#2229,.T.);
#4865=EDGE_CURVE('',#3791,#3792,#2685,.T.);
#4866=EDGE_CURVE('',#3792,#3789,#2230,.T.);
#4867=EDGE_CURVE('',#3792,#3793,#2231,.T.);
#4868=EDGE_CURVE('',#3794,#3793,#2232,.T.);
#4869=EDGE_CURVE('',#3795,#3794,#2233,.T.);
#4870=EDGE_CURVE('',#3795,#3796,#2234,.T.);
#4871=EDGE_CURVE('',#3790,#3796,#2235,.T.);
#4872=EDGE_CURVE('',#3797,#3798,#2236,.T.);
#4873=EDGE_CURVE('',#3797,#3773,#2237,.T.);
#4874=EDGE_CURVE('',#3771,#3794,#2238,.T.);
#4875=EDGE_CURVE('',#3791,#3799,#2239,.T.);
#4876=EDGE_CURVE('',#3799,#3798,#2240,.T.);
#4877=EDGE_CURVE('',#3800,#3798,#1877,.T.);
#4878=EDGE_CURVE('',#3772,#3800,#1878,.T.);
#4879=EDGE_CURVE('',#3772,#3801,#1879,.T.);
#4880=EDGE_CURVE('',#3801,#3801,#1880,.T.);
#4881=EDGE_CURVE('',#3800,#3795,#2686,.T.);
#4882=EDGE_CURVE('',#3796,#3799,#2241,.T.);
#4883=EDGE_CURVE('',#3802,#3802,#1881,.T.);
#4884=EDGE_CURVE('',#3802,#3803,#2687,.T.);
#4885=EDGE_CURVE('',#3803,#3804,#1882,.T.);
#4886=EDGE_CURVE('',#3804,#3803,#1883,.T.);
#4887=EDGE_CURVE('',#3805,#3806,#2242,.F.);
#4888=EDGE_CURVE('',#3806,#3807,#2243,.T.);
#4889=EDGE_CURVE('',#3807,#3808,#2244,.T.);
#4890=EDGE_CURVE('',#3809,#3808,#1884,.T.);
#4891=EDGE_CURVE('',#3809,#3810,#2245,.T.);
#4892=EDGE_CURVE('',#3810,#3811,#2246,.T.);
#4893=EDGE_CURVE('',#3811,#3812,#65,.T.);
#4894=EDGE_CURVE('',#3812,#3804,#63,.T.);
#4895=EDGE_CURVE('',#3812,#3813,#66,.T.);
#4896=EDGE_CURVE('',#3813,#3814,#2247,.T.);
#4897=EDGE_CURVE('',#3814,#3815,#2248,.T.);
#4898=EDGE_CURVE('',#3816,#3815,#1885,.T.);
#4899=EDGE_CURVE('',#3816,#3817,#2249,.T.);
#4900=EDGE_CURVE('',#3817,#3818,#2250,.T.);
#4901=EDGE_CURVE('',#3818,#3819,#2251,.T.);
#4902=EDGE_CURVE('',#3819,#3820,#2252,.T.);
#4903=EDGE_CURVE('',#3820,#3821,#2253,.T.);
#4904=EDGE_CURVE('',#3821,#3822,#1886,.T.);
#4905=EDGE_CURVE('',#3822,#3823,#2254,.T.);
#4906=EDGE_CURVE('',#3823,#3824,#2255,.T.);
#4907=EDGE_CURVE('',#3824,#3825,#67,.T.);
#4908=EDGE_CURVE('',#3825,#3826,#2256,.T.);
#4909=EDGE_CURVE('',#3826,#3827,#2257,.T.);
#4910=EDGE_CURVE('',#3827,#3828,#1887,.T.);
#4911=EDGE_CURVE('',#3828,#3829,#2258,.T.);
#4912=EDGE_CURVE('',#3829,#3805,#2259,.T.);
#4913=EDGE_CURVE('',#3811,#3830,#2688,.T.);
#4914=EDGE_CURVE('',#3831,#3830,#2689,.T.);
#4915=EDGE_CURVE('',#3813,#3831,#2690,.T.);
#4916=EDGE_CURVE('',#3830,#3832,#68,.T.);
#4917=EDGE_CURVE('',#3810,#3832,#2691,.T.);
#4918=EDGE_CURVE('',#3833,#3834,#2692,.T.);
#4919=EDGE_CURVE('',#3834,#3835,#69,.T.);
#4920=EDGE_CURVE('',#3835,#3836,#2693,.T.);
#4921=EDGE_CURVE('',#3836,#3837,#70,.T.);
#4922=EDGE_CURVE('',#3837,#3838,#2694,.T.);
#4923=EDGE_CURVE('',#3838,#3839,#71,.T.);
#4924=EDGE_CURVE('',#3839,#3840,#2695,.T.);
#4925=EDGE_CURVE('',#3840,#3831,#72,.T.);
#4926=EDGE_CURVE('',#3832,#3841,#2696,.T.);
#4927=EDGE_CURVE('',#3841,#3842,#73,.T.);
#4928=EDGE_CURVE('',#3842,#3843,#2697,.T.);
#4929=EDGE_CURVE('',#3843,#3844,#74,.T.);
#4930=EDGE_CURVE('',#3844,#3845,#2698,.T.);
#4931=EDGE_CURVE('',#3845,#3846,#75,.T.);
#4932=EDGE_CURVE('',#3846,#3847,#2699,.T.);
#4933=EDGE_CURVE('',#3847,#3848,#76,.T.);
#4934=EDGE_CURVE('',#3848,#3849,#2700,.T.);
#4935=EDGE_CURVE('',#3849,#3850,#77,.T.);
#4936=EDGE_CURVE('',#3850,#3851,#2701,.T.);
#4937=EDGE_CURVE('',#3851,#3852,#78,.T.);
#4938=EDGE_CURVE('',#3852,#3853,#2702,.T.);
#4939=EDGE_CURVE('',#3853,#3833,#79,.T.);
#4940=EDGE_CURVE('',#3854,#3821,#2703,.T.);
#4941=EDGE_CURVE('',#3820,#3834,#2704,.T.);
#4942=EDGE_CURVE('',#3833,#3854,#2705,.T.);
#4943=EDGE_CURVE('',#3816,#3855,#2706,.T.);
#4944=EDGE_CURVE('',#3856,#3815,#2707,.T.);
#4945=EDGE_CURVE('',#3856,#3855,#80,.T.);
#4946=EDGE_CURVE('',#3809,#3857,#2708,.T.);
#4947=EDGE_CURVE('',#3858,#3808,#2709,.T.);
#4948=EDGE_CURVE('',#3858,#3857,#81,.T.);
#4949=EDGE_CURVE('',#3828,#3859,#2710,.T.);
#4950=EDGE_CURVE('',#3860,#3827,#2711,.T.);
#4951=EDGE_CURVE('',#3860,#3859,#82,.T.);
#4952=EDGE_CURVE('',#3822,#3861,#2712,.T.);
#4953=EDGE_CURVE('',#3854,#3861,#83,.T.);
#4954=EDGE_CURVE('',#3838,#3855,#2713,.T.);
#4955=EDGE_CURVE('',#3817,#3837,#2714,.T.);
#4956=EDGE_CURVE('',#3818,#3836,#2715,.T.);
#4957=EDGE_CURVE('',#3819,#3835,#2716,.T.);
#4958=EDGE_CURVE('',#3824,#3851,#2717,.T.);
#4959=EDGE_CURVE('',#3825,#3850,#2718,.T.);
#4960=EDGE_CURVE('',#3823,#3852,#2719,.T.);
#4961=EDGE_CURVE('',#3853,#3861,#2720,.T.);
#4962=EDGE_CURVE('',#3826,#3849,#2721,.T.);
#4963=EDGE_CURVE('',#3848,#3860,#2722,.T.);
#4964=EDGE_CURVE('',#3847,#3859,#2723,.T.);
#4965=EDGE_CURVE('',#3829,#3846,#2724,.T.);
#4966=EDGE_CURVE('',#3805,#3845,#2725,.T.);
#4967=EDGE_CURVE('',#3806,#3844,#2726,.T.);
#4968=EDGE_CURVE('',#3807,#3843,#2727,.T.);
#4969=EDGE_CURVE('',#3842,#3858,#2728,.T.);
#4970=EDGE_CURVE('',#3841,#3857,#2729,.T.);
#4971=EDGE_CURVE('',#3839,#3856,#2730,.T.);
#4972=EDGE_CURVE('',#3814,#3840,#2731,.T.);
#4973=EDGE_CURVE('',#3862,#3863,#2732,.T.);
#4974=EDGE_CURVE('',#3863,#3864,#2260,.T.);
#4975=EDGE_CURVE('',#3865,#3864,#2733,.T.);
#4976=EDGE_CURVE('',#3865,#3866,#2261,.T.);
#4977=EDGE_CURVE('',#3866,#3867,#2734,.T.);
#4978=EDGE_CURVE('',#3867,#3868,#2262,.T.);
#4979=EDGE_CURVE('',#3868,#3869,#84,.T.);
#4980=EDGE_CURVE('',#3870,#3869,#2263,.T.);
#4981=EDGE_CURVE('',#3871,#3870,#2264,.T.);
#4982=EDGE_CURVE('',#3871,#3872,#85,.T.);
#4983=EDGE_CURVE('',#3872,#3862,#2265,.T.);
#4984=EDGE_CURVE('',#3873,#3874,#2735,.T.);
#4985=EDGE_CURVE('',#3863,#3874,#1888,.T.);
#4986=EDGE_CURVE('',#3862,#3873,#1889,.T.);
#4987=EDGE_CURVE('',#3875,#3876,#2736,.T.);
#4988=EDGE_CURVE('',#3877,#3876,#1890,.T.);
#4989=EDGE_CURVE('',#3877,#3875,#1891,.T.);
#4990=EDGE_CURVE('',#3878,#3879,#2737,.T.);
#4991=EDGE_CURVE('',#3879,#3880,#1892,.T.);
#4992=EDGE_CURVE('',#3878,#3880,#1893,.T.);
#4993=EDGE_CURVE('',#3881,#3873,#1894,.T.);
#4994=EDGE_CURVE('',#3881,#3874,#1895,.T.);
#4995=EDGE_CURVE('',#3882,#3883,#2738,.T.);
#4996=EDGE_CURVE('',#3882,#3884,#1896,.T.);
#4997=EDGE_CURVE('',#3883,#3884,#1897,.T.);
#4998=EDGE_CURVE('',#3885,#3875,#1898,.T.);
#4999=EDGE_CURVE('',#3885,#3886,#2739,.T.);
#5000=EDGE_CURVE('',#3876,#3886,#1899,.T.);
#5001=EDGE_CURVE('',#3876,#3887,#2266,.T.);
#5002=EDGE_CURVE('',#3886,#3888,#2267,.T.);
#5003=EDGE_CURVE('',#3887,#3888,#1900,.T.);
#5004=EDGE_CURVE('',#3887,#3889,#1901,.T.);
#5005=EDGE_CURVE('',#3890,#3889,#1902,.T.);
#5006=EDGE_CURVE('',#3877,#3890,#1903,.T.);
#5007=EDGE_CURVE('',#3891,#3877,#2268,.T.);
#5008=EDGE_CURVE('',#3892,#3890,#2269,.T.);
#5009=EDGE_CURVE('',#3891,#3892,#1904,.T.);
#5010=EDGE_CURVE('',#3875,#3893,#1905,.T.);
#5011=EDGE_CURVE('',#3891,#3894,#1906,.T.);
#5012=EDGE_CURVE('',#3894,#3893,#1907,.T.);
#5013=EDGE_CURVE('',#3885,#3895,#1908,.T.);
#5014=EDGE_CURVE('',#3895,#3893,#1909,.T.);
#5015=EDGE_CURVE('',#3895,#3896,#86,.T.);
#5016=EDGE_CURVE('',#3897,#3896,#1910,.T.);
#5017=EDGE_CURVE('',#3885,#3897,#2270,.T.);
#5018=EDGE_CURVE('',#3888,#3898,#2271,.T.);
#5019=EDGE_CURVE('',#3897,#3899,#2740,.T.);
#5020=EDGE_CURVE('',#3899,#3900,#2272,.T.);
#5021=EDGE_CURVE('',#3901,#3900,#2741,.T.);
#5022=EDGE_CURVE('',#3902,#3901,#87,.T.);
#5023=EDGE_CURVE('',#3903,#3902,#88,.T.);
#5024=EDGE_CURVE('',#3904,#3903,#2273,.T.);
#5025=EDGE_CURVE('',#3898,#3904,#2274,.T.);
#5026=EDGE_CURVE('',#3887,#3898,#2275,.T.);
#5027=EDGE_CURVE('',#3898,#3905,#1911,.T.);
#5028=EDGE_CURVE('',#3889,#3905,#2276,.T.);
#5029=EDGE_CURVE('',#3906,#3907,#2277,.T.);
#5030=EDGE_CURVE('',#3907,#3908,#2278,.T.);
#5031=EDGE_CURVE('',#3908,#3909,#2279,.T.);
#5032=EDGE_CURVE('',#3909,#3910,#2280,.T.);
#5033=EDGE_CURVE('',#3911,#3910,#1912,.T.);
#5034=EDGE_CURVE('',#3911,#3906,#2281,.T.);
#5035=EDGE_CURVE('',#3912,#3892,#2282,.T.);
#5036=EDGE_CURVE('',#3913,#3890,#1913,.T.);
#5037=EDGE_CURVE('',#3913,#3914,#2283,.T.);
#5038=EDGE_CURVE('',#3914,#3915,#2284,.T.);
#5039=EDGE_CURVE('',#3915,#3912,#2285,.T.);
#5040=EDGE_CURVE('',#3889,#3916,#1914,.T.);
#5041=EDGE_CURVE('',#3905,#3917,#2286,.T.);
#5042=EDGE_CURVE('',#3917,#3918,#2287,.T.);
#5043=EDGE_CURVE('',#3918,#3916,#2288,.T.);
#5044=EDGE_CURVE('',#3919,#3920,#2289,.T.);
#5045=EDGE_CURVE('',#3920,#3921,#2290,.T.);
#5046=EDGE_CURVE('',#3922,#3921,#1915,.T.);
#5047=EDGE_CURVE('',#3923,#3922,#1916,.T.);
#5048=EDGE_CURVE('',#3923,#3924,#2291,.T.);
#5049=EDGE_CURVE('',#3924,#3919,#2292,.T.);
#5050=EDGE_CURVE('',#3925,#3907,#2293,.T.);
#5051=EDGE_CURVE('',#3925,#3906,#1917,.T.);
#5052=EDGE_CURVE('',#3925,#3926,#1918,.T.);
#5053=EDGE_CURVE('',#3926,#3927,#2294,.T.);
#5054=EDGE_CURVE('',#3907,#3927,#1919,.T.);
#5055=EDGE_CURVE('',#3927,#3928,#2295,.T.);
#5056=EDGE_CURVE('',#3908,#3928,#1920,.T.);
#5057=EDGE_CURVE('',#3908,#3929,#2296,.T.);
#5058=EDGE_CURVE('',#3928,#3930,#2297,.T.);
#5059=EDGE_CURVE('',#3929,#3930,#1921,.T.);
#5060=EDGE_CURVE('',#3929,#3909,#1922,.T.);
#5061=EDGE_CURVE('',#3929,#3881,#2298,.T.);
#5062=EDGE_CURVE('',#3881,#3910,#1923,.T.);
#5063=EDGE_CURVE('',#3874,#3931,#1924,.T.);
#5064=EDGE_CURVE('',#3930,#3931,#1925,.T.);
#5065=EDGE_CURVE('',#3863,#3932,#1926,.T.);
#5066=EDGE_CURVE('',#3932,#3931,#1927,.T.);
#5067=EDGE_CURVE('',#3932,#3933,#89,.T.);
#5068=EDGE_CURVE('',#3864,#3933,#1928,.T.);
#5069=EDGE_CURVE('',#3864,#3934,#2299,.T.);
#5070=EDGE_CURVE('',#3933,#3935,#2300,.T.);
#5071=EDGE_CURVE('',#3934,#3935,#1929,.T.);
#5072=EDGE_CURVE('',#3936,#3865,#2301,.T.);
#5073=EDGE_CURVE('',#3936,#3934,#2742,.T.);
#5074=EDGE_CURVE('',#3936,#3937,#1930,.T.);
#5075=EDGE_CURVE('',#3937,#3938,#2302,.T.);
#5076=EDGE_CURVE('',#3865,#3938,#1931,.T.);
#5077=EDGE_CURVE('',#3866,#3939,#1932,.T.);
#5078=EDGE_CURVE('',#3938,#3939,#90,.T.);
#5079=EDGE_CURVE('',#3882,#3940,#1933,.T.);
#5080=EDGE_CURVE('',#3882,#3866,#1934,.T.);
#5081=EDGE_CURVE('',#3940,#3939,#1935,.T.);
#5082=EDGE_CURVE('',#3940,#3941,#1936,.T.);
#5083=EDGE_CURVE('',#3942,#3941,#1937,.T.);
#5084=EDGE_CURVE('',#3884,#3942,#2303,.T.);
#5085=EDGE_CURVE('',#3942,#3914,#1938,.T.);
#5086=EDGE_CURVE('',#3884,#3913,#1939,.T.);
#5087=EDGE_CURVE('',#3883,#3943,#2304,.T.);
#5088=EDGE_CURVE('',#3921,#3913,#1940,.T.);
#5089=EDGE_CURVE('',#3943,#3921,#1941,.T.);
#5090=EDGE_CURVE('',#3867,#3883,#1942,.T.);
#5091=EDGE_CURVE('',#3868,#3943,#1943,.T.);
#5092=EDGE_CURVE('',#3943,#3869,#2305,.T.);
#5093=EDGE_CURVE('',#3869,#3920,#1944,.T.);
#5094=EDGE_CURVE('',#3870,#3919,#1945,.T.);
#5095=EDGE_CURVE('',#3871,#3924,#1946,.T.);
#5096=EDGE_CURVE('',#3871,#3944,#2306,.T.);
#5097=EDGE_CURVE('',#3944,#3923,#1947,.T.);
#5098=EDGE_CURVE('',#3872,#3944,#1948,.T.);
#5099=EDGE_CURVE('',#3944,#3873,#2307,.T.);
#5100=EDGE_CURVE('',#3910,#3923,#1949,.T.);
#5101=EDGE_CURVE('',#3945,#3945,#1950,.T.);
#5102=EDGE_CURVE('',#3945,#3922,#1951,.T.);
#5103=EDGE_CURVE('',#3916,#3911,#1952,.T.);
#5104=EDGE_CURVE('',#3946,#3878,#2308,.T.);
#5105=EDGE_CURVE('',#3880,#3911,#1953,.T.);
#5106=EDGE_CURVE('',#3946,#3916,#1954,.T.);
#5107=EDGE_CURVE('',#3946,#3902,#1955,.T.);
#5108=EDGE_CURVE('',#3878,#3901,#1956,.T.);
#5109=EDGE_CURVE('',#3879,#3900,#1957,.T.);
#5110=EDGE_CURVE('',#3879,#3947,#1958,.T.);
#5111=EDGE_CURVE('',#3900,#3948,#1959,.T.);
#5112=EDGE_CURVE('',#3947,#3948,#1960,.T.);
#5113=EDGE_CURVE('',#3947,#3926,#1961,.T.);
#5114=EDGE_CURVE('',#3880,#3925,#2309,.T.);
#5115=EDGE_CURVE('',#3949,#3948,#91,.T.);
#5116=EDGE_CURVE('',#3950,#3949,#2310,.T.);
#5117=EDGE_CURVE('',#3951,#3950,#2743,.T.);
#5118=EDGE_CURVE('',#3952,#3951,#2311,.T.);
#5119=EDGE_CURVE('',#3953,#3952,#2312,.T.);
#5120=EDGE_CURVE('',#3954,#3953,#2313,.T.);
#5121=EDGE_CURVE('',#3935,#3954,#2744,.T.);
#5122=EDGE_CURVE('',#3934,#3955,#2745,.T.);
#5123=EDGE_CURVE('',#3955,#3954,#1962,.T.);
#5124=EDGE_CURVE('',#3956,#3936,#2746,.T.);
#5125=EDGE_CURVE('',#3956,#3955,#2747,.T.);
#5126=EDGE_CURVE('',#3956,#3957,#1963,.T.);
#5127=EDGE_CURVE('',#3957,#3937,#2748,.T.);
#5128=EDGE_CURVE('',#3958,#3894,#2314,.T.);
#5129=EDGE_CURVE('',#3959,#3958,#2315,.T.);
#5130=EDGE_CURVE('',#3941,#3959,#2316,.T.);
#5131=EDGE_CURVE('',#3960,#3957,#2317,.T.);
#5132=EDGE_CURVE('',#3961,#3960,#2318,.T.);
#5133=EDGE_CURVE('',#3962,#3961,#2319,.T.);
#5134=EDGE_CURVE('',#3963,#3962,#2749,.T.);
#5135=EDGE_CURVE('',#3896,#3963,#2320,.T.);
#5136=EDGE_CURVE('',#3897,#3964,#2321,.T.);
#5137=EDGE_CURVE('',#3964,#3963,#1964,.T.);
#5138=EDGE_CURVE('',#3964,#3965,#2750,.T.);
#5139=EDGE_CURVE('',#3965,#3899,#2322,.T.);
#5140=EDGE_CURVE('',#3965,#3950,#1965,.T.);
#5141=EDGE_CURVE('',#3899,#3949,#1966,.T.);
#5142=EDGE_CURVE('',#3966,#3965,#2751,.T.);
#5143=EDGE_CURVE('',#3966,#3951,#1967,.T.);
#5144=EDGE_CURVE('',#3964,#3967,#2752,.T.);
#5145=EDGE_CURVE('',#3967,#3966,#2753,.T.);
#5146=EDGE_CURVE('',#3967,#3962,#1968,.T.);
#5147=EDGE_CURVE('',#3967,#3968,#2323,.T.);
#5148=EDGE_CURVE('',#3968,#3961,#1969,.T.);
#5149=EDGE_CURVE('',#3968,#3969,#2754,.T.);
#5150=EDGE_CURVE('',#3969,#3966,#2324,.T.);
#5151=EDGE_CURVE('',#3969,#3952,#1970,.T.);
#5152=EDGE_CURVE('',#3970,#3969,#2325,.T.);
#5153=EDGE_CURVE('',#3970,#3953,#1971,.T.);
#5154=EDGE_CURVE('',#3968,#3971,#2326,.T.);
#5155=EDGE_CURVE('',#3971,#3970,#2755,.T.);
#5156=EDGE_CURVE('',#3972,#3973,#2327,.T.);
#5157=EDGE_CURVE('',#3973,#3974,#2328,.T.);
#5158=EDGE_CURVE('',#3974,#3975,#2329,.T.);
#5159=EDGE_CURVE('',#3975,#3972,#2330,.T.);
#5160=EDGE_CURVE('',#3972,#3976,#1972,.T.);
#5161=EDGE_CURVE('',#3976,#3973,#1973,.T.);
#5162=EDGE_CURVE('',#3975,#3974,#1974,.T.);
#5163=EDGE_CURVE('',#3977,#3978,#1975,.T.);
#5164=EDGE_CURVE('',#3978,#3976,#2756,.T.);
#5165=EDGE_CURVE('',#3978,#3977,#1976,.T.);
#5166=EDGE_CURVE('',#3977,#3979,#2757,.T.);
#5167=EDGE_CURVE('',#3979,#3979,#1977,.T.);
#5168=EDGE_CURVE('',#3980,#3980,#1978,.T.);
#5169=EDGE_CURVE('',#3980,#3981,#2758,.T.);
#5170=EDGE_CURVE('',#3981,#3981,#1979,.T.);
#5171=EDGE_CURVE('',#3971,#3960,#1980,.T.);
#5172=EDGE_CURVE('',#3971,#3956,#2331,.T.);
#5173=EDGE_CURVE('',#3955,#3970,#2332,.T.);
#5174=EDGE_CURVE('',#3942,#3915,#2333,.T.);
#5175=EDGE_CURVE('',#3915,#3959,#1981,.T.);
#5176=EDGE_CURVE('',#3912,#3958,#1982,.T.);
#5177=EDGE_CURVE('',#3912,#3891,#2334,.T.);
#5178=EDGE_CURVE('',#3903,#3946,#2335,.T.);
#5179=EDGE_CURVE('',#3903,#3918,#1983,.T.);
#5180=EDGE_CURVE('',#3904,#3917,#1984,.T.);
#5181=EDGE_CURVE('',#3982,#3982,#1985,.T.);
#5182=EDGE_CURVE('',#3983,#3984,#92,.T.);
#5183=EDGE_CURVE('',#3984,#3985,#2759,.T.);
#5184=EDGE_CURVE('',#3985,#3986,#93,.T.);
#5185=EDGE_CURVE('',#3986,#3987,#2760,.T.);
#5186=EDGE_CURVE('',#3987,#3988,#94,.T.);
#5187=EDGE_CURVE('',#3988,#3989,#2761,.T.);
#5188=EDGE_CURVE('',#3989,#3990,#95,.T.);
#5189=EDGE_CURVE('',#3990,#3991,#2762,.T.);
#5190=EDGE_CURVE('',#3991,#3992,#96,.T.);
#5191=EDGE_CURVE('',#3992,#3993,#2763,.T.);
#5192=EDGE_CURVE('',#3993,#3994,#97,.T.);
#5193=EDGE_CURVE('',#3994,#3995,#2764,.T.);
#5194=EDGE_CURVE('',#3995,#3996,#98,.T.);
#5195=EDGE_CURVE('',#3996,#3997,#2765,.T.);
#5196=EDGE_CURVE('',#3997,#3998,#99,.T.);
#5197=EDGE_CURVE('',#3998,#3999,#2766,.T.);
#5198=EDGE_CURVE('',#3999,#4000,#100,.T.);
#5199=EDGE_CURVE('',#4000,#4001,#2767,.T.);
#5200=EDGE_CURVE('',#4001,#4002,#101,.T.);
#5201=EDGE_CURVE('',#4002,#4003,#2768,.T.);
#5202=EDGE_CURVE('',#4003,#4004,#102,.T.);
#5203=EDGE_CURVE('',#4004,#4005,#2769,.T.);
#5204=EDGE_CURVE('',#4005,#4006,#103,.T.);
#5205=EDGE_CURVE('',#4006,#3983,#2770,.T.);
#5206=EDGE_CURVE('',#3982,#4007,#2771,.T.);
#5207=EDGE_CURVE('',#4007,#4007,#1986,.T.);
#5208=EDGE_CURVE('',#4007,#4008,#2772,.T.);
#5209=EDGE_CURVE('',#4008,#4008,#1987,.T.);
#5210=EDGE_CURVE('',#4008,#4009,#1988,.T.);
#5211=EDGE_CURVE('',#4009,#4010,#1989,.T.);
#5212=EDGE_CURVE('',#4010,#4009,#1990,.T.);
#5213=EDGE_CURVE('',#4011,#4012,#2336,.T.);
#5214=EDGE_CURVE('',#4011,#4013,#1991,.T.);
#5215=EDGE_CURVE('',#4013,#4010,#2773,.T.);
#5216=EDGE_CURVE('',#4013,#4012,#1992,.T.);
#5217=EDGE_CURVE('',#4014,#4012,#2337,.T.);
#5218=EDGE_CURVE('',#4014,#4011,#2774,.T.);
#5219=EDGE_CURVE('',#4015,#4014,#2338,.F.);
#5220=EDGE_CURVE('',#4016,#4015,#2775,.T.);
#5221=EDGE_CURVE('',#4016,#4017,#2339,.T.);
#5222=EDGE_CURVE('',#4017,#4011,#2340,.T.);
#5223=EDGE_CURVE('',#4018,#4015,#2341,.T.);
#5224=EDGE_CURVE('',#4014,#4019,#2342,.T.);
#5225=EDGE_CURVE('',#4020,#4019,#2343,.T.);
#5226=EDGE_CURVE('',#4018,#4020,#2776,.T.);
#5227=EDGE_CURVE('',#4021,#4018,#2344,.F.);
#5228=EDGE_CURVE('',#4022,#4021,#2777,.T.);
#5229=EDGE_CURVE('',#4022,#4016,#2345,.T.);
#5230=EDGE_CURVE('',#4023,#4021,#2346,.T.);
#5231=EDGE_CURVE('',#4024,#4020,#2347,.T.);
#5232=EDGE_CURVE('',#4023,#4024,#2778,.T.);
#5233=EDGE_CURVE('',#4025,#4023,#2348,.F.);
#5234=EDGE_CURVE('',#4026,#4025,#2779,.T.);
#5235=EDGE_CURVE('',#4026,#4022,#2349,.T.);
#5236=EDGE_CURVE('',#4027,#4025,#2350,.T.);
#5237=EDGE_CURVE('',#4028,#4024,#2351,.T.);
#5238=EDGE_CURVE('',#4027,#4028,#2780,.T.);
#5239=EDGE_CURVE('',#4029,#4027,#2352,.F.);
#5240=EDGE_CURVE('',#4030,#4029,#2781,.T.);
#5241=EDGE_CURVE('',#4030,#4026,#2353,.T.);
#5242=EDGE_CURVE('',#4031,#4029,#2354,.T.);
#5243=EDGE_CURVE('',#4032,#4028,#2355,.T.);
#5244=EDGE_CURVE('',#4031,#4032,#2782,.T.);
#5245=EDGE_CURVE('',#4033,#4031,#2356,.F.);
#5246=EDGE_CURVE('',#4034,#4033,#2783,.T.);
#5247=EDGE_CURVE('',#4034,#4030,#2357,.T.);
#5248=EDGE_CURVE('',#4035,#4033,#2358,.T.);
#5249=EDGE_CURVE('',#4036,#4032,#2359,.T.);
#5250=EDGE_CURVE('',#4035,#4036,#2784,.T.);
#5251=EDGE_CURVE('',#4037,#4035,#2360,.F.);
#5252=EDGE_CURVE('',#4038,#4037,#2361,.T.);
#5253=EDGE_CURVE('',#4039,#4038,#2362,.T.);
#5254=EDGE_CURVE('',#4039,#4034,#2363,.T.);
#5255=EDGE_CURVE('',#4040,#4036,#2364,.T.);
#5256=EDGE_CURVE('',#4038,#4040,#2365,.T.);
#5257=EDGE_CURVE('',#4040,#4039,#2366,.T.);
#5258=EDGE_CURVE('',#4036,#4034,#2785,.T.);
#5259=EDGE_CURVE('',#4032,#4030,#2786,.T.);
#5260=EDGE_CURVE('',#4028,#4026,#2787,.T.);
#5261=EDGE_CURVE('',#4024,#4022,#2788,.T.);
#5262=EDGE_CURVE('',#4020,#4016,#2789,.T.);
#5263=EDGE_CURVE('',#4019,#4017,#2367,.T.);
#5264=EDGE_CURVE('',#3983,#4041,#2790,.T.);
#5265=EDGE_CURVE('',#4042,#4041,#104,.T.);
#5266=EDGE_CURVE('',#3984,#4042,#2791,.T.);
#5267=EDGE_CURVE('',#4043,#4006,#2792,.T.);
#5268=EDGE_CURVE('',#4043,#4041,#2793,.T.);
#5269=EDGE_CURVE('',#4044,#4045,#2794,.T.);
#5270=EDGE_CURVE('',#4045,#4046,#105,.T.);
#5271=EDGE_CURVE('',#4046,#4047,#2795,.T.);
#5272=EDGE_CURVE('',#4047,#4048,#106,.T.);
#5273=EDGE_CURVE('',#4042,#4048,#2796,.T.);
#5274=EDGE_CURVE('',#4043,#4049,#107,.T.);
#5275=EDGE_CURVE('',#4050,#4049,#2797,.T.);
#5276=EDGE_CURVE('',#4050,#4051,#108,.T.);
#5277=EDGE_CURVE('',#4051,#4052,#2798,.T.);
#5278=EDGE_CURVE('',#4052,#4053,#109,.T.);
#5279=EDGE_CURVE('',#4054,#4053,#2799,.T.);
#5280=EDGE_CURVE('',#4054,#4055,#110,.T.);
#5281=EDGE_CURVE('',#4055,#4056,#2800,.T.);
#5282=EDGE_CURVE('',#4056,#4057,#111,.T.);
#5283=EDGE_CURVE('',#4057,#4058,#2801,.T.);
#5284=EDGE_CURVE('',#4058,#4059,#112,.T.);
#5285=EDGE_CURVE('',#4059,#4060,#2802,.T.);
#5286=EDGE_CURVE('',#4060,#4061,#113,.T.);
#5287=EDGE_CURVE('',#4062,#4061,#2803,.T.);
#5288=EDGE_CURVE('',#4062,#4063,#114,.T.);
#5289=EDGE_CURVE('',#4063,#4064,#2804,.T.);
#5290=EDGE_CURVE('',#4064,#4044,#115,.T.);
#5291=EDGE_CURVE('',#3989,#4044,#2805,.T.);
#5292=EDGE_CURVE('',#4045,#3988,#2806,.T.);
#5293=EDGE_CURVE('',#3990,#4064,#2807,.T.);
#5294=EDGE_CURVE('',#4063,#3991,#2808,.T.);
#5295=EDGE_CURVE('',#4062,#3992,#2809,.T.);
#5296=EDGE_CURVE('',#4061,#3993,#2810,.T.);
#5297=EDGE_CURVE('',#4060,#3994,#2811,.T.);
#5298=EDGE_CURVE('',#3995,#4059,#2812,.T.);
#5299=EDGE_CURVE('',#3996,#4058,#2813,.T.);
#5300=EDGE_CURVE('',#4057,#3997,#2814,.T.);
#5301=EDGE_CURVE('',#4056,#3998,#2815,.T.);
#5302=EDGE_CURVE('',#4055,#3999,#2816,.T.);
#5303=EDGE_CURVE('',#4054,#4000,#2817,.T.);
#5304=EDGE_CURVE('',#4001,#4053,#2818,.T.);
#5305=EDGE_CURVE('',#4002,#4052,#2819,.T.);
#5306=EDGE_CURVE('',#4051,#4003,#2820,.T.);
#5307=EDGE_CURVE('',#4050,#4004,#2821,.T.);
#5308=EDGE_CURVE('',#4049,#4005,#2822,.T.);
#5309=EDGE_CURVE('',#4046,#3987,#2823,.T.);
#5310=EDGE_CURVE('',#4047,#3986,#2824,.T.);
#5311=EDGE_CURVE('',#4048,#3985,#2825,.T.);
#5312=EDGE_CURVE('',#4065,#4066,#2826,.T.);
#5313=EDGE_CURVE('',#4065,#4067,#2827,.T.);
#5314=EDGE_CURVE('',#4068,#4067,#2828,.T.);
#5315=EDGE_CURVE('',#4069,#4068,#2368,.T.);
#5316=EDGE_CURVE('',#4070,#4069,#2829,.T.);
#5317=EDGE_CURVE('',#4066,#4070,#1993,.T.);
#5318=EDGE_CURVE('',#4071,#4071,#1994,.T.);
#5319=EDGE_CURVE('',#4072,#4073,#1995,.T.);
#5320=EDGE_CURVE('',#4073,#4072,#1996,.T.);
#5321=EDGE_CURVE('',#4073,#4071,#1997,.T.);
#5322=EDGE_CURVE('',#4074,#4074,#1998,.T.);
#5323=EDGE_CURVE('',#4074,#4072,#2830,.T.);
#5324=EDGE_CURVE('',#4075,#4075,#1999,.T.);
#5325=EDGE_CURVE('',#4076,#4077,#2000,.T.);
#5326=EDGE_CURVE('',#4077,#4076,#2001,.T.);
#5327=EDGE_CURVE('',#4077,#4075,#2831,.T.);
#5328=EDGE_CURVE('',#4078,#4078,#2002,.T.);
#5329=EDGE_CURVE('',#4078,#4079,#2832,.T.);
#5330=EDGE_CURVE('',#4080,#4079,#2369,.F.);
#5331=EDGE_CURVE('',#4081,#4080,#2833,.T.);
#5332=EDGE_CURVE('',#4079,#4081,#2370,.F.);
#5333=EDGE_CURVE('',#4076,#4082,#2371,.T.);
#5334=EDGE_CURVE('',#4083,#4076,#2372,.T.);
#5335=EDGE_CURVE('',#4082,#4083,#2373,.T.);
#5336=EDGE_CURVE('',#4082,#4084,#2374,.T.);
#5337=EDGE_CURVE('',#4085,#4084,#2834,.T.);
#5338=EDGE_CURVE('',#4086,#4085,#2375,.T.);
#5339=EDGE_CURVE('',#4087,#4086,#2376,.T.);
#5340=EDGE_CURVE('',#4076,#4087,#2377,.T.);
#5341=EDGE_CURVE('',#4085,#4088,#2378,.T.);
#5342=EDGE_CURVE('',#4089,#4088,#2379,.F.);
#5343=EDGE_CURVE('',#4090,#4089,#2835,.T.);
#5344=EDGE_CURVE('',#4083,#4090,#2380,.T.);
#5345=EDGE_CURVE('',#4084,#4090,#2836,.T.);
#5346=EDGE_CURVE('',#4090,#4091,#2381,.T.);
#5347=EDGE_CURVE('',#4092,#4091,#2837,.T.);
#5348=EDGE_CURVE('',#4084,#4092,#2382,.T.);
#5349=EDGE_CURVE('',#4093,#4092,#2838,.T.);
#5350=EDGE_CURVE('',#4089,#4093,#2383,.F.);
#5351=EDGE_CURVE('',#4093,#4094,#2384,.T.);
#5352=EDGE_CURVE('',#4091,#4094,#2839,.T.);
#5353=EDGE_CURVE('',#4094,#4095,#2385,.T.);
#5354=EDGE_CURVE('',#4095,#4096,#2386,.T.);
#5355=EDGE_CURVE('',#4097,#4096,#2840,.T.);
#5356=EDGE_CURVE('',#4091,#4097,#2387,.T.);
#5357=EDGE_CURVE('',#4092,#4098,#2388,.T.);
#5358=EDGE_CURVE('',#4095,#4098,#2841,.T.);
#5359=EDGE_CURVE('',#4098,#4099,#2389,.T.);
#5360=EDGE_CURVE('',#4080,#4099,#2390,.T.);
#5361=EDGE_CURVE('',#4096,#4080,#2391,.F.);
#5362=EDGE_CURVE('',#4100,#4081,#2392,.T.);
#5363=EDGE_CURVE('',#4097,#4100,#2393,.T.);
#5364=EDGE_CURVE('',#4098,#4097,#2842,.T.);
#5365=EDGE_CURVE('',#4099,#4100,#2394,.T.);
#5366=EDGE_CURVE('',#4101,#4101,#2003,.T.);
#5367=EDGE_CURVE('',#4101,#4102,#2843,.T.);
#5368=EDGE_CURVE('',#4102,#4102,#2004,.T.);
#5369=EDGE_CURVE('',#4103,#4104,#2395,.T.);
#5370=EDGE_CURVE('',#4104,#4103,#2396,.T.);
#5371=EDGE_CURVE('',#4105,#4105,#2005,.T.);
#5372=EDGE_CURVE('',#4105,#4106,#2844,.T.);
#5373=EDGE_CURVE('',#4106,#4106,#2006,.T.);
#5374=EDGE_CURVE('',#4107,#4108,#2397,.T.);
#5375=EDGE_CURVE('',#4109,#4107,#2845,.T.);
#5376=EDGE_CURVE('',#4110,#4109,#2398,.T.);
#5377=EDGE_CURVE('',#4111,#4110,#2399,.T.);
#5378=EDGE_CURVE('',#4112,#4111,#2400,.T.);
#5379=EDGE_CURVE('',#4113,#4112,#2846,.T.);
#5380=EDGE_CURVE('',#4114,#4113,#2847,.T.);
#5381=EDGE_CURVE('',#4115,#4114,#2007,.T.);
#5382=EDGE_CURVE('',#4116,#4115,#2008,.T.);
#5383=EDGE_CURVE('',#4117,#4116,#2848,.T.);
#5384=EDGE_CURVE('',#4118,#4117,#2009,.T.);
#5385=EDGE_CURVE('',#4119,#4118,#2849,.T.);
#5386=EDGE_CURVE('',#4120,#4119,#2010,.T.);
#5387=EDGE_CURVE('',#4121,#4120,#2011,.T.);
#5388=EDGE_CURVE('',#4108,#4121,#2850,.T.);
#5389=EDGE_CURVE('',#4122,#4122,#2012,.T.);
#5390=EDGE_CURVE('',#4123,#4123,#2013,.T.);
#5391=EDGE_CURVE('',#4123,#4122,#2851,.T.);
#5392=EDGE_CURVE('',#4124,#4125,#2852,.T.);
#5393=EDGE_CURVE('',#4125,#4126,#2014,.T.);
#5394=EDGE_CURVE('',#4126,#4127,#2853,.T.);
#5395=EDGE_CURVE('',#4127,#4124,#2015,.T.);
#5396=EDGE_CURVE('',#4124,#4128,#2016,.T.);
#5397=EDGE_CURVE('',#4129,#4128,#2854,.T.);
#5398=EDGE_CURVE('',#4125,#4129,#2401,.T.);
#5399=EDGE_CURVE('',#4125,#4130,#2017,.T.);
#5400=EDGE_CURVE('',#4129,#4131,#2018,.T.);
#5401=EDGE_CURVE('',#4130,#4131,#2402,.T.);
#5402=EDGE_CURVE('',#4126,#4132,#2019,.T.);
#5403=EDGE_CURVE('',#4130,#4132,#2020,.T.);
#5404=EDGE_CURVE('',#4133,#4134,#2021,.T.);
#5405=EDGE_CURVE('',#4133,#4126,#2403,.T.);
#5406=EDGE_CURVE('',#4134,#4132,#2404,.T.);
#5407=EDGE_CURVE('',#4135,#4136,#2022,.T.);
#5408=EDGE_CURVE('',#4136,#4133,#2855,.T.);
#5409=EDGE_CURVE('',#4134,#4135,#2856,.T.);
#5410=EDGE_CURVE('',#4135,#4120,#2023,.T.);
#5411=EDGE_CURVE('',#4136,#4119,#2024,.T.);
#5412=EDGE_CURVE('',#4136,#4137,#2857,.T.);
#5413=EDGE_CURVE('',#4137,#4118,#2025,.T.);
#5414=EDGE_CURVE('',#4137,#4138,#2858,.T.);
#5415=EDGE_CURVE('',#4138,#4133,#2859,.T.);
#5416=EDGE_CURVE('',#4127,#4138,#2026,.T.);
#5417=EDGE_CURVE('',#4138,#4128,#2027,.T.);
#5418=EDGE_CURVE('',#4137,#4139,#2028,.T.);
#5419=EDGE_CURVE('',#4139,#4128,#2860,.T.);
#5420=EDGE_CURVE('',#4139,#4117,#2029,.T.);
#5421=EDGE_CURVE('',#4139,#4140,#2861,.T.);
#5422=EDGE_CURVE('',#4140,#4116,#2030,.T.);
#5423=EDGE_CURVE('',#4129,#4140,#2862,.T.);
#5424=EDGE_CURVE('',#4140,#4141,#2031,.T.);
#5425=EDGE_CURVE('',#4141,#4131,#2863,.T.);
#5426=EDGE_CURVE('',#4141,#4115,#2032,.T.);
#5427=EDGE_CURVE('',#4141,#4142,#2033,.T.);
#5428=EDGE_CURVE('',#4142,#4114,#2034,.T.);
#5429=EDGE_CURVE('',#4143,#4135,#2035,.T.);
#5430=EDGE_CURVE('',#4144,#4142,#2864,.T.);
#5431=EDGE_CURVE('',#4144,#4145,#2036,.T.);
#5432=EDGE_CURVE('',#4145,#4143,#2865,.T.);
#5433=EDGE_CURVE('',#4143,#4121,#2037,.T.);
#5434=EDGE_CURVE('',#4146,#4143,#2866,.T.);
#5435=EDGE_CURVE('',#4146,#4108,#2038,.T.);
#5436=EDGE_CURVE('',#4145,#4147,#2867,.T.);
#5437=EDGE_CURVE('',#4147,#4148,#2405,.T.);
#5438=EDGE_CURVE('',#4148,#4149,#2868,.T.);
#5439=EDGE_CURVE('',#4149,#4146,#2406,.T.);
#5440=EDGE_CURVE('',#4150,#4146,#2407,.T.);
#5441=EDGE_CURVE('',#4151,#4149,#2039,.T.);
#5442=EDGE_CURVE('',#4151,#4152,#116,.T.);
#5443=EDGE_CURVE('',#4150,#4152,#2408,.T.);
#5444=EDGE_CURVE('',#4153,#4150,#2409,.T.);
#5445=EDGE_CURVE('',#4153,#4107,#117,.T.);
#5446=EDGE_CURVE('',#4153,#4154,#2869,.T.);
#5447=EDGE_CURVE('',#4154,#4109,#2040,.T.);
#5448=EDGE_CURVE('',#4155,#4154,#2410,.T.);
#5449=EDGE_CURVE('',#4155,#4110,#2041,.T.);
#5450=EDGE_CURVE('',#4154,#4156,#2870,.T.);
#5451=EDGE_CURVE('',#4157,#4156,#118,.T.);
#5452=EDGE_CURVE('',#4158,#4157,#2871,.T.);
#5453=EDGE_CURVE('',#4158,#4159,#2411,.T.);
#5454=EDGE_CURVE('',#4160,#4159,#2412,.T.);
#5455=EDGE_CURVE('',#4161,#4160,#2413,.T.);
#5456=EDGE_CURVE('',#4155,#4161,#2414,.T.);
#5457=EDGE_CURVE('',#4162,#4155,#2415,.T.);
#5458=EDGE_CURVE('',#4161,#4162,#2042,.T.);
#5459=EDGE_CURVE('',#4162,#4111,#2043,.T.);
#5460=EDGE_CURVE('',#4163,#4162,#2416,.T.);
#5461=EDGE_CURVE('',#4163,#4112,#2044,.T.);
#5462=EDGE_CURVE('',#4160,#4164,#2045,.T.);
#5463=EDGE_CURVE('',#4164,#4165,#2417,.T.);
#5464=EDGE_CURVE('',#4165,#4163,#2418,.T.);
#5465=EDGE_CURVE('',#4165,#4166,#2046,.T.);
#5466=EDGE_CURVE('',#4166,#4112,#2419,.T.);
#5467=EDGE_CURVE('',#4113,#4167,#2047,.T.);
#5468=EDGE_CURVE('',#4167,#4166,#2872,.T.);
#5469=EDGE_CURVE('',#4168,#4169,#2048,.T.);
#5470=EDGE_CURVE('',#4168,#4113,#2049,.T.);
#5471=EDGE_CURVE('',#4169,#4167,#2050,.T.);
#5472=EDGE_CURVE('',#4142,#4168,#2873,.T.);
#5473=EDGE_CURVE('',#4169,#4170,#2874,.T.);
#5474=EDGE_CURVE('',#4170,#4171,#2051,.T.);
#5475=EDGE_CURVE('',#4171,#4144,#2875,.T.);
#5476=EDGE_CURVE('',#4172,#4172,#2052,.T.);
#5477=EDGE_CURVE('',#4173,#4173,#2053,.T.);
#5478=EDGE_CURVE('',#4173,#4172,#2876,.T.);
#5479=EDGE_CURVE('',#4174,#4174,#2054,.T.);
#5480=EDGE_CURVE('',#4175,#4175,#2055,.T.);
#5481=EDGE_CURVE('',#4175,#4103,#2877,.T.);
#5482=EDGE_CURVE('',#4104,#4174,#2878,.T.);
#5483=EDGE_CURVE('',#4176,#4177,#119,.T.);
#5484=EDGE_CURVE('',#4176,#4178,#2879,.T.);
#5485=EDGE_CURVE('',#4178,#4179,#120,.T.);
#5486=EDGE_CURVE('',#4180,#4179,#2880,.T.);
#5487=EDGE_CURVE('',#4181,#4180,#121,.T.);
#5488=EDGE_CURVE('',#4157,#4181,#2881,.T.);
#5489=EDGE_CURVE('',#4156,#4177,#2882,.T.);
#5490=EDGE_CURVE('',#4176,#4151,#2883,.T.);
#5491=EDGE_CURVE('',#4177,#4152,#2884,.T.);
#5492=EDGE_CURVE('',#4182,#4151,#2885,.T.);
#5493=EDGE_CURVE('',#4182,#4178,#2886,.T.);
#5494=EDGE_CURVE('',#4182,#4148,#2056,.T.);
#5495=EDGE_CURVE('',#4147,#4183,#2420,.T.);
#5496=EDGE_CURVE('',#4184,#4183,#2421,.T.);
#5497=EDGE_CURVE('',#4184,#4182,#122,.T.);
#5498=EDGE_CURVE('',#4183,#4185,#2422,.T.);
#5499=EDGE_CURVE('',#4147,#4069,#2057,.T.);
#5500=EDGE_CURVE('',#4185,#4068,#123,.T.);
#5501=EDGE_CURVE('',#4185,#4186,#2887,.T.);
#5502=EDGE_CURVE('',#4180,#4186,#2888,.T.);
#5503=EDGE_CURVE('',#4184,#4179,#2889,.T.);
#5504=EDGE_CURVE('',#4186,#4187,#2423,.T.);
#5505=EDGE_CURVE('',#4181,#4187,#2890,.T.);
#5506=EDGE_CURVE('',#4186,#4067,#124,.T.);
#5507=EDGE_CURVE('',#4067,#4188,#2424,.T.);
#5508=EDGE_CURVE('',#4187,#4188,#125,.T.);
#5509=EDGE_CURVE('',#4187,#4158,#2891,.T.);
#5510=EDGE_CURVE('',#4188,#4189,#2892,.T.);
#5511=EDGE_CURVE('',#4158,#4189,#2058,.T.);
#5512=EDGE_CURVE('',#4189,#4190,#126,.T.);
#5513=EDGE_CURVE('',#4159,#4190,#2059,.T.);
#5514=EDGE_CURVE('',#4159,#4164,#2425,.T.);
#5515=EDGE_CURVE('',#4190,#4191,#2426,.T.);
#5516=EDGE_CURVE('',#4164,#4191,#2060,.T.);
#5517=EDGE_CURVE('',#4191,#4166,#2427,.T.);
#5518=EDGE_CURVE('',#4167,#4192,#2893,.T.);
#5519=EDGE_CURVE('',#4192,#4188,#2894,.T.);
#5520=EDGE_CURVE('',#4170,#4192,#2061,.T.);
#5521=EDGE_CURVE('',#4192,#4065,#2062,.T.);
#5522=EDGE_CURVE('',#4171,#4065,#2063,.T.);
#5523=EDGE_CURVE('',#4144,#4066,#2064,.T.);
#5524=EDGE_CURVE('',#4145,#4070,#2065,.T.);
#5525=EDGE_CURVE('',#4193,#4193,#2066,.T.);
#5526=EDGE_CURVE('',#4194,#4194,#2067,.T.);
#5527=EDGE_CURVE('',#4194,#4195,#2895,.T.);
#5528=EDGE_CURVE('',#4195,#4195,#2068,.T.);
#5529=EDGE_CURVE('',#4196,#4196,#2069,.T.);
#5530=EDGE_CURVE('',#4196,#4193,#2070,.T.);
#5531=EDGE_CURVE('',#4197,#4198,#2428,.T.);
#5532=EDGE_CURVE('',#4197,#4199,#2429,.T.);
#5533=EDGE_CURVE('',#4200,#4199,#2430,.T.);
#5534=EDGE_CURVE('',#4200,#4201,#2431,.T.);
#5535=EDGE_CURVE('',#4201,#4198,#2432,.T.);
#5536=EDGE_CURVE('',#4202,#4202,#2071,.T.);
#5537=EDGE_CURVE('',#4203,#4203,#2072,.T.);
#5538=EDGE_CURVE('',#4203,#4202,#2896,.T.);
#5539=EDGE_CURVE('',#4204,#4204,#2073,.T.);
#5540=EDGE_CURVE('',#4205,#4206,#2433,.F.);
#5541=EDGE_CURVE('',#4207,#4206,#2434,.T.);
#5542=EDGE_CURVE('',#4207,#4208,#2435,.T.);
#5543=EDGE_CURVE('',#4209,#4208,#2436,.T.);
#5544=EDGE_CURVE('',#4209,#4210,#2437,.T.);
#5545=EDGE_CURVE('',#4211,#4210,#2438,.T.);
#5546=EDGE_CURVE('',#4211,#4212,#2439,.T.);
#5547=EDGE_CURVE('',#4213,#4212,#2440,.T.);
#5548=EDGE_CURVE('',#4213,#4214,#2441,.T.);
#5549=EDGE_CURVE('',#4215,#4214,#2442,.T.);
#5550=EDGE_CURVE('',#4215,#4204,#64,.T.);
#5551=EDGE_CURVE('',#4216,#4215,#2443,.T.);
#5552=EDGE_CURVE('',#4216,#4217,#2444,.T.);
#5553=EDGE_CURVE('',#4205,#4217,#2445,.T.);
#5554=EDGE_CURVE('',#4218,#4219,#2074,.T.);
#5555=EDGE_CURVE('',#4206,#4218,#2897,.T.);
#5556=EDGE_CURVE('',#4205,#4219,#2898,.T.);
#5557=EDGE_CURVE('',#4220,#4219,#2899,.T.);
#5558=EDGE_CURVE('',#4220,#4221,#2075,.T.);
#5559=EDGE_CURVE('',#4222,#4221,#2900,.T.);
#5560=EDGE_CURVE('',#4222,#4223,#2076,.T.);
#5561=EDGE_CURVE('',#4224,#4223,#2901,.T.);
#5562=EDGE_CURVE('',#4224,#4225,#2077,.T.);
#5563=EDGE_CURVE('',#4226,#4225,#2902,.T.);
#5564=EDGE_CURVE('',#4226,#4227,#2078,.T.);
#5565=EDGE_CURVE('',#4228,#4227,#2903,.T.);
#5566=EDGE_CURVE('',#4228,#4229,#2079,.T.);
#5567=EDGE_CURVE('',#4218,#4229,#2904,.T.);
#5568=EDGE_CURVE('',#4230,#4230,#2080,.T.);
#5569=EDGE_CURVE('',#4230,#4231,#2905,.T.);
#5570=EDGE_CURVE('',#4231,#4232,#2446,.T.);
#5571=EDGE_CURVE('',#4232,#4233,#2906,.T.);
#5572=EDGE_CURVE('',#4233,#4231,#2447,.T.);
#5573=EDGE_CURVE('',#4234,#4232,#2448,.T.);
#5574=EDGE_CURVE('',#4235,#4234,#2449,.T.);
#5575=EDGE_CURVE('',#4233,#4235,#2450,.T.);
#5576=EDGE_CURVE('',#4236,#4237,#2451,.T.);
#5577=EDGE_CURVE('',#4237,#4233,#2452,.T.);
#5578=EDGE_CURVE('',#4238,#4235,#2453,.T.);
#5579=EDGE_CURVE('',#4236,#4238,#2907,.T.);
#5580=EDGE_CURVE('',#4239,#4236,#2454,.F.);
#5581=EDGE_CURVE('',#4240,#4239,#2908,.T.);
#5582=EDGE_CURVE('',#4240,#4241,#2455,.T.);
#5583=EDGE_CURVE('',#4241,#4237,#2909,.T.);
#5584=EDGE_CURVE('',#4242,#4239,#2456,.T.);
#5585=EDGE_CURVE('',#4243,#4238,#2457,.T.);
#5586=EDGE_CURVE('',#4242,#4243,#2910,.T.);
#5587=EDGE_CURVE('',#4199,#4240,#2458,.T.);
#5588=EDGE_CURVE('',#4201,#4242,#2459,.F.);
#5589=EDGE_CURVE('',#4198,#4243,#2460,.T.);
#5590=EDGE_CURVE('',#4243,#4240,#2911,.T.);
#5591=EDGE_CURVE('',#4238,#4241,#2912,.T.);
#5592=EDGE_CURVE('',#4241,#4234,#2461,.T.);
#5593=EDGE_CURVE('',#4207,#4229,#2913,.T.);
#5594=EDGE_CURVE('',#4208,#4228,#2914,.T.);
#5595=EDGE_CURVE('',#4209,#4227,#2915,.T.);
#5596=EDGE_CURVE('',#4210,#4226,#2916,.T.);
#5597=EDGE_CURVE('',#4211,#4225,#2917,.T.);
#5598=EDGE_CURVE('',#4212,#4224,#2918,.T.);
#5599=EDGE_CURVE('',#4217,#4220,#2919,.T.);
#5600=EDGE_CURVE('',#4216,#4221,#2920,.T.);
#5601=EDGE_CURVE('',#4214,#4222,#2921,.T.);
#5602=EDGE_CURVE('',#4213,#4223,#2922,.T.);
#5603=EDGE_CURVE('',#4244,#4244,#2081,.T.);
#5604=EDGE_CURVE('',#4244,#4244,#2082,.T.);
#5605=EDGE_CURVE('',#4245,#4245,#2083,.T.);
#5606=EDGE_CURVE('',#4246,#4246,#2084,.T.);
#5607=EDGE_CURVE('',#4246,#4247,#2923,.T.);
#5608=EDGE_CURVE('',#4247,#4247,#2085,.T.);
#5609=EDGE_CURVE('',#4248,#4248,#2086,.T.);
#5610=EDGE_CURVE('',#4248,#4245,#2924,.T.);
#5611=EDGE_CURVE('',#4249,#4249,#2087,.T.);
#5612=EDGE_CURVE('',#4250,#4250,#2088,.T.);
#5613=EDGE_CURVE('',#4249,#4251,#2925,.T.);
#5614=EDGE_CURVE('',#4251,#4251,#2089,.T.);
#5615=EDGE_CURVE('',#4251,#4252,#2090,.T.);
#5616=EDGE_CURVE('',#4253,#4254,#2091,.T.);
#5617=EDGE_CURVE('',#4253,#4250,#2926,.T.);
#5618=EDGE_CURVE('',#4254,#4253,#2092,.T.);
#5619=EDGE_CURVE('',#4255,#4254,#2093,.T.);
#5620=ORIENTED_EDGE('',*,*,#4256,.F.);
#5621=ORIENTED_EDGE('',*,*,#4257,.T.);
#5622=ORIENTED_EDGE('',*,*,#4258,.T.);
#5623=ORIENTED_EDGE('',*,*,#4259,.T.);
#5624=ORIENTED_EDGE('',*,*,#4258,.F.);
#5625=ORIENTED_EDGE('',*,*,#4260,.T.);
#5626=ORIENTED_EDGE('',*,*,#4261,.F.);
#5627=ORIENTED_EDGE('',*,*,#4262,.T.);
#5628=ORIENTED_EDGE('',*,*,#4256,.T.);
#5629=ORIENTED_EDGE('',*,*,#4263,.T.);
#5630=ORIENTED_EDGE('',*,*,#4264,.F.);
#5631=ORIENTED_EDGE('',*,*,#4265,.T.);
#5632=ORIENTED_EDGE('',*,*,#4266,.T.);
#5633=ORIENTED_EDGE('',*,*,#4261,.T.);
#5634=ORIENTED_EDGE('',*,*,#4267,.T.);
#5635=ORIENTED_EDGE('',*,*,#4268,.F.);
#5636=ORIENTED_EDGE('',*,*,#4269,.T.);
#5637=ORIENTED_EDGE('',*,*,#4264,.T.);
#5638=ORIENTED_EDGE('',*,*,#4270,.T.);
#5639=ORIENTED_EDGE('',*,*,#4271,.T.);
#5640=ORIENTED_EDGE('',*,*,#4272,.F.);
#5641=ORIENTED_EDGE('',*,*,#4273,.T.);
#5642=ORIENTED_EDGE('',*,*,#4268,.T.);
#5643=ORIENTED_EDGE('',*,*,#4274,.T.);
#5644=ORIENTED_EDGE('',*,*,#4260,.F.);
#5645=ORIENTED_EDGE('',*,*,#4275,.F.);
#5646=ORIENTED_EDGE('',*,*,#4276,.F.);
#5647=ORIENTED_EDGE('',*,*,#4277,.F.);
#5648=ORIENTED_EDGE('',*,*,#4278,.F.);
#5649=ORIENTED_EDGE('',*,*,#4272,.T.);
#5650=ORIENTED_EDGE('',*,*,#4279,.T.);
#5651=ORIENTED_EDGE('',*,*,#4280,.F.);
#5652=ORIENTED_EDGE('',*,*,#4281,.F.);
#5653=ORIENTED_EDGE('',*,*,#4280,.T.);
#5654=ORIENTED_EDGE('',*,*,#4282,.F.);
#5655=ORIENTED_EDGE('',*,*,#4263,.F.);
#5656=ORIENTED_EDGE('',*,*,#4278,.T.);
#5657=ORIENTED_EDGE('',*,*,#4283,.T.);
#5658=ORIENTED_EDGE('',*,*,#4284,.F.);
#5659=ORIENTED_EDGE('',*,*,#4270,.F.);
#5660=ORIENTED_EDGE('',*,*,#4267,.F.);
#5661=ORIENTED_EDGE('',*,*,#4271,.F.);
#5662=ORIENTED_EDGE('',*,*,#4284,.T.);
#5663=ORIENTED_EDGE('',*,*,#4285,.T.);
#5664=ORIENTED_EDGE('',*,*,#4286,.F.);
#5665=ORIENTED_EDGE('',*,*,#4279,.F.);
#5666=ORIENTED_EDGE('',*,*,#4274,.F.);
#5667=ORIENTED_EDGE('',*,*,#4282,.T.);
#5668=ORIENTED_EDGE('',*,*,#4286,.T.);
#5669=ORIENTED_EDGE('',*,*,#4287,.T.);
#5670=ORIENTED_EDGE('',*,*,#4288,.T.);
#5671=ORIENTED_EDGE('',*,*,#4289,.T.);
#5672=ORIENTED_EDGE('',*,*,#4273,.F.);
#5673=ORIENTED_EDGE('',*,*,#4289,.F.);
#5674=ORIENTED_EDGE('',*,*,#4290,.F.);
#5675=ORIENTED_EDGE('',*,*,#4291,.T.);
#5676=ORIENTED_EDGE('',*,*,#4265,.F.);
#5677=ORIENTED_EDGE('',*,*,#4269,.F.);
#5678=ORIENTED_EDGE('',*,*,#4266,.F.);
#5679=ORIENTED_EDGE('',*,*,#4291,.F.);
#5680=ORIENTED_EDGE('',*,*,#4292,.F.);
#5681=ORIENTED_EDGE('',*,*,#4275,.T.);
#5682=ORIENTED_EDGE('',*,*,#4257,.F.);
#5683=ORIENTED_EDGE('',*,*,#4262,.F.);
#5684=ORIENTED_EDGE('',*,*,#4276,.T.);
#5685=ORIENTED_EDGE('',*,*,#4292,.T.);
#5686=ORIENTED_EDGE('',*,*,#4293,.F.);
#5687=ORIENTED_EDGE('',*,*,#4294,.F.);
#5688=ORIENTED_EDGE('',*,*,#4277,.T.);
#5689=ORIENTED_EDGE('',*,*,#4294,.T.);
#5690=ORIENTED_EDGE('',*,*,#4295,.F.);
#5691=ORIENTED_EDGE('',*,*,#4283,.F.);
#5692=ORIENTED_EDGE('',*,*,#4295,.T.);
#5693=ORIENTED_EDGE('',*,*,#4296,.T.);
#5694=ORIENTED_EDGE('',*,*,#4287,.F.);
#5695=ORIENTED_EDGE('',*,*,#4285,.F.);
#5696=ORIENTED_EDGE('',*,*,#4293,.T.);
#5697=ORIENTED_EDGE('',*,*,#4290,.T.);
#5698=ORIENTED_EDGE('',*,*,#4288,.F.);
#5699=ORIENTED_EDGE('',*,*,#4296,.F.);
#5700=ORIENTED_EDGE('',*,*,#4281,.T.);
#5701=ORIENTED_EDGE('',*,*,#4297,.T.);
#5702=ORIENTED_EDGE('',*,*,#4298,.T.);
#5703=ORIENTED_EDGE('',*,*,#4299,.F.);
#5704=ORIENTED_EDGE('',*,*,#4300,.T.);
#5705=ORIENTED_EDGE('',*,*,#4297,.F.);
#5706=ORIENTED_EDGE('',*,*,#4301,.F.);
#5707=ORIENTED_EDGE('',*,*,#4302,.F.);
#5708=ORIENTED_EDGE('',*,*,#4298,.F.);
#5709=ORIENTED_EDGE('',*,*,#4302,.T.);
#5710=ORIENTED_EDGE('',*,*,#4303,.F.);
#5711=ORIENTED_EDGE('',*,*,#4304,.F.);
#5712=ORIENTED_EDGE('',*,*,#4305,.F.);
#5713=ORIENTED_EDGE('',*,*,#4299,.T.);
#5714=ORIENTED_EDGE('',*,*,#4305,.T.);
#5715=ORIENTED_EDGE('',*,*,#4306,.T.);
#5716=ORIENTED_EDGE('',*,*,#4307,.F.);
#5717=ORIENTED_EDGE('',*,*,#4308,.F.);
#5718=ORIENTED_EDGE('',*,*,#4301,.T.);
#5719=ORIENTED_EDGE('',*,*,#4300,.F.);
#5720=ORIENTED_EDGE('',*,*,#4308,.T.);
#5721=ORIENTED_EDGE('',*,*,#4309,.T.);
#5722=ORIENTED_EDGE('',*,*,#4310,.F.);
#5723=ORIENTED_EDGE('',*,*,#4311,.F.);
#5724=ORIENTED_EDGE('',*,*,#4303,.T.);
#5725=ORIENTED_EDGE('',*,*,#4304,.T.);
#5726=ORIENTED_EDGE('',*,*,#4311,.T.);
#5727=ORIENTED_EDGE('',*,*,#4312,.F.);
#5728=ORIENTED_EDGE('',*,*,#4306,.F.);
#5729=ORIENTED_EDGE('',*,*,#4312,.T.);
#5730=ORIENTED_EDGE('',*,*,#4313,.T.);
#5731=ORIENTED_EDGE('',*,*,#4314,.F.);
#5732=ORIENTED_EDGE('',*,*,#4315,.F.);
#5733=ORIENTED_EDGE('',*,*,#4316,.F.);
#5734=ORIENTED_EDGE('',*,*,#4309,.F.);
#5735=ORIENTED_EDGE('',*,*,#4307,.T.);
#5736=ORIENTED_EDGE('',*,*,#4315,.T.);
#5737=ORIENTED_EDGE('',*,*,#4317,.F.);
#5738=ORIENTED_EDGE('',*,*,#4316,.T.);
#5739=ORIENTED_EDGE('',*,*,#4318,.T.);
#5740=ORIENTED_EDGE('',*,*,#4319,.F.);
#5741=ORIENTED_EDGE('',*,*,#4313,.F.);
#5742=ORIENTED_EDGE('',*,*,#4310,.T.);
#5743=ORIENTED_EDGE('',*,*,#4320,.T.);
#5744=ORIENTED_EDGE('',*,*,#4321,.T.);
#5745=ORIENTED_EDGE('',*,*,#4322,.F.);
#5746=ORIENTED_EDGE('',*,*,#4323,.F.);
#5747=ORIENTED_EDGE('',*,*,#4319,.T.);
#5748=ORIENTED_EDGE('',*,*,#4320,.F.);
#5749=ORIENTED_EDGE('',*,*,#4318,.F.);
#5750=ORIENTED_EDGE('',*,*,#4317,.T.);
#5751=ORIENTED_EDGE('',*,*,#4324,.T.);
#5752=ORIENTED_EDGE('',*,*,#4325,.F.);
#5753=ORIENTED_EDGE('',*,*,#4321,.F.);
#5754=ORIENTED_EDGE('',*,*,#4325,.T.);
#5755=ORIENTED_EDGE('',*,*,#4326,.T.);
#5756=ORIENTED_EDGE('',*,*,#4327,.T.);
#5757=ORIENTED_EDGE('',*,*,#4328,.F.);
#5758=ORIENTED_EDGE('',*,*,#4329,.F.);
#5759=ORIENTED_EDGE('',*,*,#4330,.T.);
#5760=ORIENTED_EDGE('',*,*,#4331,.F.);
#5761=ORIENTED_EDGE('',*,*,#4322,.T.);
#5762=ORIENTED_EDGE('',*,*,#4329,.T.);
#5763=ORIENTED_EDGE('',*,*,#4332,.T.);
#5764=ORIENTED_EDGE('',*,*,#4333,.T.);
#5765=ORIENTED_EDGE('',*,*,#4327,.F.);
#5766=ORIENTED_EDGE('',*,*,#4334,.F.);
#5767=ORIENTED_EDGE('',*,*,#4335,.F.);
#5768=ORIENTED_EDGE('',*,*,#4330,.F.);
#5769=ORIENTED_EDGE('',*,*,#4336,.T.);
#5770=ORIENTED_EDGE('',*,*,#4333,.F.);
#5771=ORIENTED_EDGE('',*,*,#4337,.T.);
#5772=ORIENTED_EDGE('',*,*,#4328,.T.);
#5773=ORIENTED_EDGE('',*,*,#4332,.F.);
#5774=ORIENTED_EDGE('',*,*,#4337,.F.);
#5775=ORIENTED_EDGE('',*,*,#4336,.F.);
#5776=ORIENTED_EDGE('',*,*,#4334,.T.);
#5777=ORIENTED_EDGE('',*,*,#4326,.F.);
#5778=ORIENTED_EDGE('',*,*,#4338,.T.);
#5779=ORIENTED_EDGE('',*,*,#4331,.T.);
#5780=ORIENTED_EDGE('',*,*,#4335,.T.);
#5781=ORIENTED_EDGE('',*,*,#4314,.T.);
#5782=ORIENTED_EDGE('',*,*,#4323,.T.);
#5783=ORIENTED_EDGE('',*,*,#4338,.F.);
#5784=ORIENTED_EDGE('',*,*,#4324,.F.);
#5785=ORIENTED_EDGE('',*,*,#4339,.F.);
#5786=ORIENTED_EDGE('',*,*,#4259,.F.);
#5787=ORIENTED_EDGE('',*,*,#4340,.F.);
#5788=ORIENTED_EDGE('',*,*,#4341,.F.);
#5789=ORIENTED_EDGE('',*,*,#4342,.T.);
#5790=ORIENTED_EDGE('',*,*,#4339,.T.);
#5791=ORIENTED_EDGE('',*,*,#4342,.F.);
#5792=ORIENTED_EDGE('',*,*,#4340,.T.);
#5793=ORIENTED_EDGE('',*,*,#4341,.T.);
#5794=ORIENTED_EDGE('',*,*,#4343,.F.);
#5795=ORIENTED_EDGE('',*,*,#4343,.T.);
#5796=ORIENTED_EDGE('',*,*,#4344,.T.);
#5797=ORIENTED_EDGE('',*,*,#4345,.T.);
#5798=ORIENTED_EDGE('',*,*,#4346,.T.);
#5799=ORIENTED_EDGE('',*,*,#4347,.T.);
#5800=ORIENTED_EDGE('',*,*,#4348,.T.);
#5801=ORIENTED_EDGE('',*,*,#4349,.T.);
#5802=ORIENTED_EDGE('',*,*,#4350,.T.);
#5803=ORIENTED_EDGE('',*,*,#4351,.T.);
#5804=ORIENTED_EDGE('',*,*,#4352,.T.);
#5805=ORIENTED_EDGE('',*,*,#4353,.T.);
#5806=ORIENTED_EDGE('',*,*,#4354,.T.);
#5807=ORIENTED_EDGE('',*,*,#4355,.T.);
#5808=ORIENTED_EDGE('',*,*,#4356,.T.);
#5809=ORIENTED_EDGE('',*,*,#4357,.T.);
#5810=ORIENTED_EDGE('',*,*,#4358,.T.);
#5811=ORIENTED_EDGE('',*,*,#4359,.T.);
#5812=ORIENTED_EDGE('',*,*,#4360,.T.);
#5813=ORIENTED_EDGE('',*,*,#4361,.T.);
#5814=ORIENTED_EDGE('',*,*,#4362,.T.);
#5815=ORIENTED_EDGE('',*,*,#4363,.T.);
#5816=ORIENTED_EDGE('',*,*,#4364,.T.);
#5817=ORIENTED_EDGE('',*,*,#4365,.T.);
#5818=ORIENTED_EDGE('',*,*,#4366,.T.);
#5819=ORIENTED_EDGE('',*,*,#4367,.T.);
#5820=ORIENTED_EDGE('',*,*,#4368,.T.);
#5821=ORIENTED_EDGE('',*,*,#4369,.T.);
#5822=ORIENTED_EDGE('',*,*,#4370,.T.);
#5823=ORIENTED_EDGE('',*,*,#4371,.T.);
#5824=ORIENTED_EDGE('',*,*,#4372,.T.);
#5825=ORIENTED_EDGE('',*,*,#4373,.T.);
#5826=ORIENTED_EDGE('',*,*,#4374,.T.);
#5827=ORIENTED_EDGE('',*,*,#4375,.T.);
#5828=ORIENTED_EDGE('',*,*,#4376,.T.);
#5829=ORIENTED_EDGE('',*,*,#4377,.T.);
#5830=ORIENTED_EDGE('',*,*,#4378,.T.);
#5831=ORIENTED_EDGE('',*,*,#4379,.T.);
#5832=ORIENTED_EDGE('',*,*,#4380,.T.);
#5833=ORIENTED_EDGE('',*,*,#4381,.T.);
#5834=ORIENTED_EDGE('',*,*,#4382,.T.);
#5835=ORIENTED_EDGE('',*,*,#4383,.T.);
#5836=ORIENTED_EDGE('',*,*,#4384,.T.);
#5837=ORIENTED_EDGE('',*,*,#4385,.T.);
#5838=ORIENTED_EDGE('',*,*,#4386,.T.);
#5839=ORIENTED_EDGE('',*,*,#4387,.T.);
#5840=ORIENTED_EDGE('',*,*,#4388,.T.);
#5841=ORIENTED_EDGE('',*,*,#4389,.T.);
#5842=ORIENTED_EDGE('',*,*,#4390,.T.);
#5843=ORIENTED_EDGE('',*,*,#4391,.T.);
#5844=ORIENTED_EDGE('',*,*,#4392,.T.);
#5845=ORIENTED_EDGE('',*,*,#4393,.T.);
#5846=ORIENTED_EDGE('',*,*,#4394,.T.);
#5847=ORIENTED_EDGE('',*,*,#4395,.T.);
#5848=ORIENTED_EDGE('',*,*,#4396,.T.);
#5849=ORIENTED_EDGE('',*,*,#4397,.T.);
#5850=ORIENTED_EDGE('',*,*,#4398,.T.);
#5851=ORIENTED_EDGE('',*,*,#4399,.T.);
#5852=ORIENTED_EDGE('',*,*,#4400,.T.);
#5853=ORIENTED_EDGE('',*,*,#4401,.T.);
#5854=ORIENTED_EDGE('',*,*,#4402,.T.);
#5855=ORIENTED_EDGE('',*,*,#4403,.T.);
#5856=ORIENTED_EDGE('',*,*,#4404,.T.);
#5857=ORIENTED_EDGE('',*,*,#4405,.T.);
#5858=ORIENTED_EDGE('',*,*,#4406,.T.);
#5859=ORIENTED_EDGE('',*,*,#4407,.T.);
#5860=ORIENTED_EDGE('',*,*,#4408,.T.);
#5861=ORIENTED_EDGE('',*,*,#4409,.T.);
#5862=ORIENTED_EDGE('',*,*,#4410,.T.);
#5863=ORIENTED_EDGE('',*,*,#4411,.T.);
#5864=ORIENTED_EDGE('',*,*,#4412,.T.);
#5865=ORIENTED_EDGE('',*,*,#4413,.T.);
#5866=ORIENTED_EDGE('',*,*,#4414,.T.);
#5867=ORIENTED_EDGE('',*,*,#4415,.T.);
#5868=ORIENTED_EDGE('',*,*,#4416,.T.);
#5869=ORIENTED_EDGE('',*,*,#4417,.T.);
#5870=ORIENTED_EDGE('',*,*,#4418,.T.);
#5871=ORIENTED_EDGE('',*,*,#4419,.T.);
#5872=ORIENTED_EDGE('',*,*,#4420,.T.);
#5873=ORIENTED_EDGE('',*,*,#4421,.T.);
#5874=ORIENTED_EDGE('',*,*,#4422,.T.);
#5875=ORIENTED_EDGE('',*,*,#4423,.T.);
#5876=ORIENTED_EDGE('',*,*,#4424,.T.);
#5877=ORIENTED_EDGE('',*,*,#4425,.T.);
#5878=ORIENTED_EDGE('',*,*,#4426,.T.);
#5879=ORIENTED_EDGE('',*,*,#4427,.T.);
#5880=ORIENTED_EDGE('',*,*,#4428,.T.);
#5881=ORIENTED_EDGE('',*,*,#4429,.T.);
#5882=ORIENTED_EDGE('',*,*,#4430,.T.);
#5883=ORIENTED_EDGE('',*,*,#4431,.T.);
#5884=ORIENTED_EDGE('',*,*,#4432,.T.);
#5885=ORIENTED_EDGE('',*,*,#4433,.T.);
#5886=ORIENTED_EDGE('',*,*,#4434,.T.);
#5887=ORIENTED_EDGE('',*,*,#4435,.T.);
#5888=ORIENTED_EDGE('',*,*,#4436,.T.);
#5889=ORIENTED_EDGE('',*,*,#4437,.T.);
#5890=ORIENTED_EDGE('',*,*,#4438,.T.);
#5891=ORIENTED_EDGE('',*,*,#4439,.T.);
#5892=ORIENTED_EDGE('',*,*,#4440,.F.);
#5893=ORIENTED_EDGE('',*,*,#4441,.F.);
#5894=ORIENTED_EDGE('',*,*,#4442,.F.);
#5895=ORIENTED_EDGE('',*,*,#4443,.F.);
#5896=ORIENTED_EDGE('',*,*,#4444,.F.);
#5897=ORIENTED_EDGE('',*,*,#4445,.F.);
#5898=ORIENTED_EDGE('',*,*,#4440,.T.);
#5899=ORIENTED_EDGE('',*,*,#4446,.T.);
#5900=ORIENTED_EDGE('',*,*,#4447,.F.);
#5901=ORIENTED_EDGE('',*,*,#4448,.F.);
#5902=ORIENTED_EDGE('',*,*,#4441,.T.);
#5903=ORIENTED_EDGE('',*,*,#4448,.T.);
#5904=ORIENTED_EDGE('',*,*,#4449,.F.);
#5905=ORIENTED_EDGE('',*,*,#4450,.F.);
#5906=ORIENTED_EDGE('',*,*,#4442,.T.);
#5907=ORIENTED_EDGE('',*,*,#4450,.T.);
#5908=ORIENTED_EDGE('',*,*,#4451,.F.);
#5909=ORIENTED_EDGE('',*,*,#4452,.F.);
#5910=ORIENTED_EDGE('',*,*,#4443,.T.);
#5911=ORIENTED_EDGE('',*,*,#4452,.T.);
#5912=ORIENTED_EDGE('',*,*,#4453,.F.);
#5913=ORIENTED_EDGE('',*,*,#4454,.F.);
#5914=ORIENTED_EDGE('',*,*,#4444,.T.);
#5915=ORIENTED_EDGE('',*,*,#4454,.T.);
#5916=ORIENTED_EDGE('',*,*,#4455,.F.);
#5917=ORIENTED_EDGE('',*,*,#4456,.F.);
#5918=ORIENTED_EDGE('',*,*,#4445,.T.);
#5919=ORIENTED_EDGE('',*,*,#4456,.T.);
#5920=ORIENTED_EDGE('',*,*,#4457,.F.);
#5921=ORIENTED_EDGE('',*,*,#4446,.F.);
#5922=ORIENTED_EDGE('',*,*,#4458,.T.);
#5923=ORIENTED_EDGE('',*,*,#4447,.T.);
#5924=ORIENTED_EDGE('',*,*,#4457,.T.);
#5925=ORIENTED_EDGE('',*,*,#4455,.T.);
#5926=ORIENTED_EDGE('',*,*,#4453,.T.);
#5927=ORIENTED_EDGE('',*,*,#4451,.T.);
#5928=ORIENTED_EDGE('',*,*,#4449,.T.);
#5929=ORIENTED_EDGE('',*,*,#4458,.F.);
#5930=ORIENTED_EDGE('',*,*,#4459,.T.);
#5931=ORIENTED_EDGE('',*,*,#4460,.F.);
#5932=ORIENTED_EDGE('',*,*,#4459,.F.);
#5933=ORIENTED_EDGE('',*,*,#4461,.T.);
#5934=ORIENTED_EDGE('',*,*,#4462,.F.);
#5935=ORIENTED_EDGE('',*,*,#4463,.F.);
#5936=ORIENTED_EDGE('',*,*,#4464,.F.);
#5937=ORIENTED_EDGE('',*,*,#4465,.F.);
#5938=ORIENTED_EDGE('',*,*,#4466,.F.);
#5939=ORIENTED_EDGE('',*,*,#4467,.T.);
#5940=ORIENTED_EDGE('',*,*,#4468,.F.);
#5941=ORIENTED_EDGE('',*,*,#4469,.F.);
#5942=ORIENTED_EDGE('',*,*,#4470,.F.);
#5943=ORIENTED_EDGE('',*,*,#4471,.F.);
#5944=ORIENTED_EDGE('',*,*,#4472,.F.);
#5945=ORIENTED_EDGE('',*,*,#4473,.T.);
#5946=ORIENTED_EDGE('',*,*,#4474,.F.);
#5947=ORIENTED_EDGE('',*,*,#4475,.F.);
#5948=ORIENTED_EDGE('',*,*,#4476,.F.);
#5949=ORIENTED_EDGE('',*,*,#4477,.F.);
#5950=ORIENTED_EDGE('',*,*,#4478,.F.);
#5951=ORIENTED_EDGE('',*,*,#4479,.T.);
#5952=ORIENTED_EDGE('',*,*,#4480,.F.);
#5953=ORIENTED_EDGE('',*,*,#4481,.F.);
#5954=ORIENTED_EDGE('',*,*,#4482,.F.);
#5955=ORIENTED_EDGE('',*,*,#4483,.F.);
#5956=ORIENTED_EDGE('',*,*,#4484,.F.);
#5957=ORIENTED_EDGE('',*,*,#4485,.T.);
#5958=ORIENTED_EDGE('',*,*,#4486,.F.);
#5959=ORIENTED_EDGE('',*,*,#4487,.F.);
#5960=ORIENTED_EDGE('',*,*,#4488,.F.);
#5961=ORIENTED_EDGE('',*,*,#4489,.F.);
#5962=ORIENTED_EDGE('',*,*,#4490,.F.);
#5963=ORIENTED_EDGE('',*,*,#4491,.T.);
#5964=ORIENTED_EDGE('',*,*,#4492,.F.);
#5965=ORIENTED_EDGE('',*,*,#4493,.F.);
#5966=ORIENTED_EDGE('',*,*,#4494,.F.);
#5967=ORIENTED_EDGE('',*,*,#4495,.F.);
#5968=ORIENTED_EDGE('',*,*,#4496,.F.);
#5969=ORIENTED_EDGE('',*,*,#4497,.T.);
#5970=ORIENTED_EDGE('',*,*,#4498,.F.);
#5971=ORIENTED_EDGE('',*,*,#4499,.F.);
#5972=ORIENTED_EDGE('',*,*,#4500,.F.);
#5973=ORIENTED_EDGE('',*,*,#4501,.F.);
#5974=ORIENTED_EDGE('',*,*,#4502,.F.);
#5975=ORIENTED_EDGE('',*,*,#4503,.T.);
#5976=ORIENTED_EDGE('',*,*,#4504,.F.);
#5977=ORIENTED_EDGE('',*,*,#4505,.F.);
#5978=ORIENTED_EDGE('',*,*,#4506,.F.);
#5979=ORIENTED_EDGE('',*,*,#4507,.F.);
#5980=ORIENTED_EDGE('',*,*,#4508,.F.);
#5981=ORIENTED_EDGE('',*,*,#4509,.T.);
#5982=ORIENTED_EDGE('',*,*,#4510,.F.);
#5983=ORIENTED_EDGE('',*,*,#4511,.F.);
#5984=ORIENTED_EDGE('',*,*,#4512,.F.);
#5985=ORIENTED_EDGE('',*,*,#4513,.F.);
#5986=ORIENTED_EDGE('',*,*,#4514,.F.);
#5987=ORIENTED_EDGE('',*,*,#4515,.T.);
#5988=ORIENTED_EDGE('',*,*,#4516,.F.);
#5989=ORIENTED_EDGE('',*,*,#4517,.F.);
#5990=ORIENTED_EDGE('',*,*,#4518,.F.);
#5991=ORIENTED_EDGE('',*,*,#4519,.F.);
#5992=ORIENTED_EDGE('',*,*,#4520,.F.);
#5993=ORIENTED_EDGE('',*,*,#4521,.T.);
#5994=ORIENTED_EDGE('',*,*,#4522,.F.);
#5995=ORIENTED_EDGE('',*,*,#4523,.F.);
#5996=ORIENTED_EDGE('',*,*,#4524,.F.);
#5997=ORIENTED_EDGE('',*,*,#4525,.F.);
#5998=ORIENTED_EDGE('',*,*,#4526,.F.);
#5999=ORIENTED_EDGE('',*,*,#4527,.T.);
#6000=ORIENTED_EDGE('',*,*,#4528,.F.);
#6001=ORIENTED_EDGE('',*,*,#4529,.F.);
#6002=ORIENTED_EDGE('',*,*,#4530,.F.);
#6003=ORIENTED_EDGE('',*,*,#4531,.F.);
#6004=ORIENTED_EDGE('',*,*,#4532,.F.);
#6005=ORIENTED_EDGE('',*,*,#4533,.T.);
#6006=ORIENTED_EDGE('',*,*,#4534,.F.);
#6007=ORIENTED_EDGE('',*,*,#4535,.F.);
#6008=ORIENTED_EDGE('',*,*,#4536,.F.);
#6009=ORIENTED_EDGE('',*,*,#4537,.F.);
#6010=ORIENTED_EDGE('',*,*,#4538,.F.);
#6011=ORIENTED_EDGE('',*,*,#4539,.T.);
#6012=ORIENTED_EDGE('',*,*,#4540,.F.);
#6013=ORIENTED_EDGE('',*,*,#4541,.F.);
#6014=ORIENTED_EDGE('',*,*,#4542,.F.);
#6015=ORIENTED_EDGE('',*,*,#4543,.F.);
#6016=ORIENTED_EDGE('',*,*,#4544,.F.);
#6017=ORIENTED_EDGE('',*,*,#4545,.T.);
#6018=ORIENTED_EDGE('',*,*,#4546,.F.);
#6019=ORIENTED_EDGE('',*,*,#4547,.F.);
#6020=ORIENTED_EDGE('',*,*,#4548,.F.);
#6021=ORIENTED_EDGE('',*,*,#4549,.F.);
#6022=ORIENTED_EDGE('',*,*,#4550,.F.);
#6023=ORIENTED_EDGE('',*,*,#4551,.T.);
#6024=ORIENTED_EDGE('',*,*,#4552,.F.);
#6025=ORIENTED_EDGE('',*,*,#4553,.F.);
#6026=ORIENTED_EDGE('',*,*,#4554,.F.);
#6027=ORIENTED_EDGE('',*,*,#4555,.F.);
#6028=ORIENTED_EDGE('',*,*,#4556,.F.);
#6029=ORIENTED_EDGE('',*,*,#4460,.T.);
#6030=ORIENTED_EDGE('',*,*,#4557,.F.);
#6031=ORIENTED_EDGE('',*,*,#4467,.F.);
#6032=ORIENTED_EDGE('',*,*,#4558,.T.);
#6033=ORIENTED_EDGE('',*,*,#4428,.F.);
#6034=ORIENTED_EDGE('',*,*,#4559,.F.);
#6035=ORIENTED_EDGE('',*,*,#4473,.F.);
#6036=ORIENTED_EDGE('',*,*,#4560,.T.);
#6037=ORIENTED_EDGE('',*,*,#4422,.F.);
#6038=ORIENTED_EDGE('',*,*,#4561,.F.);
#6039=ORIENTED_EDGE('',*,*,#4479,.F.);
#6040=ORIENTED_EDGE('',*,*,#4562,.T.);
#6041=ORIENTED_EDGE('',*,*,#4416,.F.);
#6042=ORIENTED_EDGE('',*,*,#4563,.F.);
#6043=ORIENTED_EDGE('',*,*,#4485,.F.);
#6044=ORIENTED_EDGE('',*,*,#4564,.T.);
#6045=ORIENTED_EDGE('',*,*,#4410,.F.);
#6046=ORIENTED_EDGE('',*,*,#4565,.F.);
#6047=ORIENTED_EDGE('',*,*,#4491,.F.);
#6048=ORIENTED_EDGE('',*,*,#4566,.T.);
#6049=ORIENTED_EDGE('',*,*,#4404,.F.);
#6050=ORIENTED_EDGE('',*,*,#4567,.F.);
#6051=ORIENTED_EDGE('',*,*,#4497,.F.);
#6052=ORIENTED_EDGE('',*,*,#4568,.T.);
#6053=ORIENTED_EDGE('',*,*,#4398,.F.);
#6054=ORIENTED_EDGE('',*,*,#4569,.F.);
#6055=ORIENTED_EDGE('',*,*,#4503,.F.);
#6056=ORIENTED_EDGE('',*,*,#4570,.T.);
#6057=ORIENTED_EDGE('',*,*,#4392,.F.);
#6058=ORIENTED_EDGE('',*,*,#4571,.F.);
#6059=ORIENTED_EDGE('',*,*,#4509,.F.);
#6060=ORIENTED_EDGE('',*,*,#4572,.T.);
#6061=ORIENTED_EDGE('',*,*,#4386,.F.);
#6062=ORIENTED_EDGE('',*,*,#4573,.F.);
#6063=ORIENTED_EDGE('',*,*,#4515,.F.);
#6064=ORIENTED_EDGE('',*,*,#4574,.T.);
#6065=ORIENTED_EDGE('',*,*,#4380,.F.);
#6066=ORIENTED_EDGE('',*,*,#4575,.F.);
#6067=ORIENTED_EDGE('',*,*,#4521,.F.);
#6068=ORIENTED_EDGE('',*,*,#4576,.T.);
#6069=ORIENTED_EDGE('',*,*,#4374,.F.);
#6070=ORIENTED_EDGE('',*,*,#4577,.F.);
#6071=ORIENTED_EDGE('',*,*,#4527,.F.);
#6072=ORIENTED_EDGE('',*,*,#4578,.T.);
#6073=ORIENTED_EDGE('',*,*,#4368,.F.);
#6074=ORIENTED_EDGE('',*,*,#4579,.F.);
#6075=ORIENTED_EDGE('',*,*,#4533,.F.);
#6076=ORIENTED_EDGE('',*,*,#4580,.T.);
#6077=ORIENTED_EDGE('',*,*,#4362,.F.);
#6078=ORIENTED_EDGE('',*,*,#4581,.F.);
#6079=ORIENTED_EDGE('',*,*,#4539,.F.);
#6080=ORIENTED_EDGE('',*,*,#4582,.T.);
#6081=ORIENTED_EDGE('',*,*,#4356,.F.);
#6082=ORIENTED_EDGE('',*,*,#4583,.F.);
#6083=ORIENTED_EDGE('',*,*,#4545,.F.);
#6084=ORIENTED_EDGE('',*,*,#4584,.T.);
#6085=ORIENTED_EDGE('',*,*,#4350,.F.);
#6086=ORIENTED_EDGE('',*,*,#4585,.T.);
#6087=ORIENTED_EDGE('',*,*,#4434,.F.);
#6088=ORIENTED_EDGE('',*,*,#4586,.F.);
#6089=ORIENTED_EDGE('',*,*,#4461,.F.);
#6090=ORIENTED_EDGE('',*,*,#4587,.F.);
#6091=ORIENTED_EDGE('',*,*,#4551,.F.);
#6092=ORIENTED_EDGE('',*,*,#4588,.T.);
#6093=ORIENTED_EDGE('',*,*,#4344,.F.);
#6094=ORIENTED_EDGE('',*,*,#4427,.F.);
#6095=ORIENTED_EDGE('',*,*,#4589,.T.);
#6096=ORIENTED_EDGE('',*,*,#4468,.T.);
#6097=ORIENTED_EDGE('',*,*,#4557,.T.);
#6098=ORIENTED_EDGE('',*,*,#4590,.T.);
#6099=ORIENTED_EDGE('',*,*,#4591,.T.);
#6100=ORIENTED_EDGE('',*,*,#4469,.T.);
#6101=ORIENTED_EDGE('',*,*,#4589,.F.);
#6102=ORIENTED_EDGE('',*,*,#4426,.F.);
#6103=ORIENTED_EDGE('',*,*,#4592,.T.);
#6104=ORIENTED_EDGE('',*,*,#4590,.F.);
#6105=ORIENTED_EDGE('',*,*,#4593,.F.);
#6106=ORIENTED_EDGE('',*,*,#4594,.F.);
#6107=ORIENTED_EDGE('',*,*,#4595,.F.);
#6108=ORIENTED_EDGE('',*,*,#4593,.T.);
#6109=ORIENTED_EDGE('',*,*,#4592,.F.);
#6110=ORIENTED_EDGE('',*,*,#4425,.F.);
#6111=ORIENTED_EDGE('',*,*,#4596,.T.);
#6112=ORIENTED_EDGE('',*,*,#4595,.T.);
#6113=ORIENTED_EDGE('',*,*,#4597,.T.);
#6114=ORIENTED_EDGE('',*,*,#4470,.T.);
#6115=ORIENTED_EDGE('',*,*,#4591,.F.);
#6116=ORIENTED_EDGE('',*,*,#4594,.T.);
#6117=ORIENTED_EDGE('',*,*,#4596,.F.);
#6118=ORIENTED_EDGE('',*,*,#4424,.F.);
#6119=ORIENTED_EDGE('',*,*,#4598,.T.);
#6120=ORIENTED_EDGE('',*,*,#4471,.T.);
#6121=ORIENTED_EDGE('',*,*,#4597,.F.);
#6122=ORIENTED_EDGE('',*,*,#4423,.F.);
#6123=ORIENTED_EDGE('',*,*,#4560,.F.);
#6124=ORIENTED_EDGE('',*,*,#4472,.T.);
#6125=ORIENTED_EDGE('',*,*,#4598,.F.);
#6126=ORIENTED_EDGE('',*,*,#4558,.F.);
#6127=ORIENTED_EDGE('',*,*,#4466,.T.);
#6128=ORIENTED_EDGE('',*,*,#4599,.F.);
#6129=ORIENTED_EDGE('',*,*,#4429,.F.);
#6130=ORIENTED_EDGE('',*,*,#4600,.T.);
#6131=ORIENTED_EDGE('',*,*,#4601,.F.);
#6132=ORIENTED_EDGE('',*,*,#4430,.F.);
#6133=ORIENTED_EDGE('',*,*,#4599,.T.);
#6134=ORIENTED_EDGE('',*,*,#4465,.T.);
#6135=ORIENTED_EDGE('',*,*,#4602,.F.);
#6136=ORIENTED_EDGE('',*,*,#4603,.F.);
#6137=ORIENTED_EDGE('',*,*,#4604,.F.);
#6138=ORIENTED_EDGE('',*,*,#4600,.F.);
#6139=ORIENTED_EDGE('',*,*,#4605,.F.);
#6140=ORIENTED_EDGE('',*,*,#4603,.T.);
#6141=ORIENTED_EDGE('',*,*,#4606,.T.);
#6142=ORIENTED_EDGE('',*,*,#4463,.T.);
#6143=ORIENTED_EDGE('',*,*,#4607,.F.);
#6144=ORIENTED_EDGE('',*,*,#4432,.F.);
#6145=ORIENTED_EDGE('',*,*,#4608,.T.);
#6146=ORIENTED_EDGE('',*,*,#4604,.T.);
#6147=ORIENTED_EDGE('',*,*,#4608,.F.);
#6148=ORIENTED_EDGE('',*,*,#4431,.F.);
#6149=ORIENTED_EDGE('',*,*,#4601,.T.);
#6150=ORIENTED_EDGE('',*,*,#4605,.T.);
#6151=ORIENTED_EDGE('',*,*,#4602,.T.);
#6152=ORIENTED_EDGE('',*,*,#4464,.T.);
#6153=ORIENTED_EDGE('',*,*,#4606,.F.);
#6154=ORIENTED_EDGE('',*,*,#4586,.T.);
#6155=ORIENTED_EDGE('',*,*,#4433,.F.);
#6156=ORIENTED_EDGE('',*,*,#4607,.T.);
#6157=ORIENTED_EDGE('',*,*,#4462,.T.);
#6158=ORIENTED_EDGE('',*,*,#4421,.F.);
#6159=ORIENTED_EDGE('',*,*,#4609,.T.);
#6160=ORIENTED_EDGE('',*,*,#4474,.T.);
#6161=ORIENTED_EDGE('',*,*,#4559,.T.);
#6162=ORIENTED_EDGE('',*,*,#4610,.T.);
#6163=ORIENTED_EDGE('',*,*,#4611,.T.);
#6164=ORIENTED_EDGE('',*,*,#4475,.T.);
#6165=ORIENTED_EDGE('',*,*,#4609,.F.);
#6166=ORIENTED_EDGE('',*,*,#4420,.F.);
#6167=ORIENTED_EDGE('',*,*,#4612,.T.);
#6168=ORIENTED_EDGE('',*,*,#4610,.F.);
#6169=ORIENTED_EDGE('',*,*,#4613,.F.);
#6170=ORIENTED_EDGE('',*,*,#4614,.F.);
#6171=ORIENTED_EDGE('',*,*,#4615,.F.);
#6172=ORIENTED_EDGE('',*,*,#4613,.T.);
#6173=ORIENTED_EDGE('',*,*,#4612,.F.);
#6174=ORIENTED_EDGE('',*,*,#4419,.F.);
#6175=ORIENTED_EDGE('',*,*,#4616,.T.);
#6176=ORIENTED_EDGE('',*,*,#4615,.T.);
#6177=ORIENTED_EDGE('',*,*,#4617,.T.);
#6178=ORIENTED_EDGE('',*,*,#4476,.T.);
#6179=ORIENTED_EDGE('',*,*,#4611,.F.);
#6180=ORIENTED_EDGE('',*,*,#4614,.T.);
#6181=ORIENTED_EDGE('',*,*,#4616,.F.);
#6182=ORIENTED_EDGE('',*,*,#4418,.F.);
#6183=ORIENTED_EDGE('',*,*,#4618,.T.);
#6184=ORIENTED_EDGE('',*,*,#4477,.T.);
#6185=ORIENTED_EDGE('',*,*,#4617,.F.);
#6186=ORIENTED_EDGE('',*,*,#4417,.F.);
#6187=ORIENTED_EDGE('',*,*,#4562,.F.);
#6188=ORIENTED_EDGE('',*,*,#4478,.T.);
#6189=ORIENTED_EDGE('',*,*,#4618,.F.);
#6190=ORIENTED_EDGE('',*,*,#4415,.F.);
#6191=ORIENTED_EDGE('',*,*,#4619,.T.);
#6192=ORIENTED_EDGE('',*,*,#4480,.T.);
#6193=ORIENTED_EDGE('',*,*,#4561,.T.);
#6194=ORIENTED_EDGE('',*,*,#4620,.T.);
#6195=ORIENTED_EDGE('',*,*,#4621,.T.);
#6196=ORIENTED_EDGE('',*,*,#4481,.T.);
#6197=ORIENTED_EDGE('',*,*,#4619,.F.);
#6198=ORIENTED_EDGE('',*,*,#4414,.F.);
#6199=ORIENTED_EDGE('',*,*,#4622,.T.);
#6200=ORIENTED_EDGE('',*,*,#4620,.F.);
#6201=ORIENTED_EDGE('',*,*,#4623,.F.);
#6202=ORIENTED_EDGE('',*,*,#4624,.F.);
#6203=ORIENTED_EDGE('',*,*,#4625,.F.);
#6204=ORIENTED_EDGE('',*,*,#4623,.T.);
#6205=ORIENTED_EDGE('',*,*,#4622,.F.);
#6206=ORIENTED_EDGE('',*,*,#4413,.F.);
#6207=ORIENTED_EDGE('',*,*,#4626,.T.);
#6208=ORIENTED_EDGE('',*,*,#4625,.T.);
#6209=ORIENTED_EDGE('',*,*,#4627,.T.);
#6210=ORIENTED_EDGE('',*,*,#4482,.T.);
#6211=ORIENTED_EDGE('',*,*,#4621,.F.);
#6212=ORIENTED_EDGE('',*,*,#4624,.T.);
#6213=ORIENTED_EDGE('',*,*,#4626,.F.);
#6214=ORIENTED_EDGE('',*,*,#4412,.F.);
#6215=ORIENTED_EDGE('',*,*,#4628,.T.);
#6216=ORIENTED_EDGE('',*,*,#4483,.T.);
#6217=ORIENTED_EDGE('',*,*,#4627,.F.);
#6218=ORIENTED_EDGE('',*,*,#4411,.F.);
#6219=ORIENTED_EDGE('',*,*,#4564,.F.);
#6220=ORIENTED_EDGE('',*,*,#4484,.T.);
#6221=ORIENTED_EDGE('',*,*,#4628,.F.);
#6222=ORIENTED_EDGE('',*,*,#4409,.F.);
#6223=ORIENTED_EDGE('',*,*,#4629,.T.);
#6224=ORIENTED_EDGE('',*,*,#4486,.T.);
#6225=ORIENTED_EDGE('',*,*,#4563,.T.);
#6226=ORIENTED_EDGE('',*,*,#4630,.T.);
#6227=ORIENTED_EDGE('',*,*,#4631,.T.);
#6228=ORIENTED_EDGE('',*,*,#4487,.T.);
#6229=ORIENTED_EDGE('',*,*,#4629,.F.);
#6230=ORIENTED_EDGE('',*,*,#4408,.F.);
#6231=ORIENTED_EDGE('',*,*,#4632,.T.);
#6232=ORIENTED_EDGE('',*,*,#4630,.F.);
#6233=ORIENTED_EDGE('',*,*,#4633,.F.);
#6234=ORIENTED_EDGE('',*,*,#4634,.F.);
#6235=ORIENTED_EDGE('',*,*,#4635,.F.);
#6236=ORIENTED_EDGE('',*,*,#4633,.T.);
#6237=ORIENTED_EDGE('',*,*,#4632,.F.);
#6238=ORIENTED_EDGE('',*,*,#4407,.F.);
#6239=ORIENTED_EDGE('',*,*,#4636,.T.);
#6240=ORIENTED_EDGE('',*,*,#4635,.T.);
#6241=ORIENTED_EDGE('',*,*,#4637,.T.);
#6242=ORIENTED_EDGE('',*,*,#4488,.T.);
#6243=ORIENTED_EDGE('',*,*,#4631,.F.);
#6244=ORIENTED_EDGE('',*,*,#4634,.T.);
#6245=ORIENTED_EDGE('',*,*,#4636,.F.);
#6246=ORIENTED_EDGE('',*,*,#4406,.F.);
#6247=ORIENTED_EDGE('',*,*,#4638,.T.);
#6248=ORIENTED_EDGE('',*,*,#4489,.T.);
#6249=ORIENTED_EDGE('',*,*,#4637,.F.);
#6250=ORIENTED_EDGE('',*,*,#4405,.F.);
#6251=ORIENTED_EDGE('',*,*,#4566,.F.);
#6252=ORIENTED_EDGE('',*,*,#4490,.T.);
#6253=ORIENTED_EDGE('',*,*,#4638,.F.);
#6254=ORIENTED_EDGE('',*,*,#4403,.F.);
#6255=ORIENTED_EDGE('',*,*,#4639,.T.);
#6256=ORIENTED_EDGE('',*,*,#4492,.T.);
#6257=ORIENTED_EDGE('',*,*,#4565,.T.);
#6258=ORIENTED_EDGE('',*,*,#4640,.T.);
#6259=ORIENTED_EDGE('',*,*,#4641,.T.);
#6260=ORIENTED_EDGE('',*,*,#4493,.T.);
#6261=ORIENTED_EDGE('',*,*,#4639,.F.);
#6262=ORIENTED_EDGE('',*,*,#4402,.F.);
#6263=ORIENTED_EDGE('',*,*,#4642,.T.);
#6264=ORIENTED_EDGE('',*,*,#4640,.F.);
#6265=ORIENTED_EDGE('',*,*,#4643,.F.);
#6266=ORIENTED_EDGE('',*,*,#4644,.F.);
#6267=ORIENTED_EDGE('',*,*,#4645,.F.);
#6268=ORIENTED_EDGE('',*,*,#4643,.T.);
#6269=ORIENTED_EDGE('',*,*,#4642,.F.);
#6270=ORIENTED_EDGE('',*,*,#4401,.F.);
#6271=ORIENTED_EDGE('',*,*,#4646,.T.);
#6272=ORIENTED_EDGE('',*,*,#4645,.T.);
#6273=ORIENTED_EDGE('',*,*,#4647,.T.);
#6274=ORIENTED_EDGE('',*,*,#4494,.T.);
#6275=ORIENTED_EDGE('',*,*,#4641,.F.);
#6276=ORIENTED_EDGE('',*,*,#4644,.T.);
#6277=ORIENTED_EDGE('',*,*,#4646,.F.);
#6278=ORIENTED_EDGE('',*,*,#4400,.F.);
#6279=ORIENTED_EDGE('',*,*,#4648,.T.);
#6280=ORIENTED_EDGE('',*,*,#4495,.T.);
#6281=ORIENTED_EDGE('',*,*,#4647,.F.);
#6282=ORIENTED_EDGE('',*,*,#4399,.F.);
#6283=ORIENTED_EDGE('',*,*,#4568,.F.);
#6284=ORIENTED_EDGE('',*,*,#4496,.T.);
#6285=ORIENTED_EDGE('',*,*,#4648,.F.);
#6286=ORIENTED_EDGE('',*,*,#4397,.F.);
#6287=ORIENTED_EDGE('',*,*,#4649,.T.);
#6288=ORIENTED_EDGE('',*,*,#4498,.T.);
#6289=ORIENTED_EDGE('',*,*,#4567,.T.);
#6290=ORIENTED_EDGE('',*,*,#4650,.T.);
#6291=ORIENTED_EDGE('',*,*,#4651,.T.);
#6292=ORIENTED_EDGE('',*,*,#4499,.T.);
#6293=ORIENTED_EDGE('',*,*,#4649,.F.);
#6294=ORIENTED_EDGE('',*,*,#4396,.F.);
#6295=ORIENTED_EDGE('',*,*,#4652,.T.);
#6296=ORIENTED_EDGE('',*,*,#4650,.F.);
#6297=ORIENTED_EDGE('',*,*,#4653,.F.);
#6298=ORIENTED_EDGE('',*,*,#4654,.F.);
#6299=ORIENTED_EDGE('',*,*,#4655,.F.);
#6300=ORIENTED_EDGE('',*,*,#4653,.T.);
#6301=ORIENTED_EDGE('',*,*,#4652,.F.);
#6302=ORIENTED_EDGE('',*,*,#4395,.F.);
#6303=ORIENTED_EDGE('',*,*,#4656,.T.);
#6304=ORIENTED_EDGE('',*,*,#4655,.T.);
#6305=ORIENTED_EDGE('',*,*,#4657,.T.);
#6306=ORIENTED_EDGE('',*,*,#4500,.T.);
#6307=ORIENTED_EDGE('',*,*,#4651,.F.);
#6308=ORIENTED_EDGE('',*,*,#4654,.T.);
#6309=ORIENTED_EDGE('',*,*,#4656,.F.);
#6310=ORIENTED_EDGE('',*,*,#4394,.F.);
#6311=ORIENTED_EDGE('',*,*,#4658,.T.);
#6312=ORIENTED_EDGE('',*,*,#4501,.T.);
#6313=ORIENTED_EDGE('',*,*,#4657,.F.);
#6314=ORIENTED_EDGE('',*,*,#4393,.F.);
#6315=ORIENTED_EDGE('',*,*,#4570,.F.);
#6316=ORIENTED_EDGE('',*,*,#4502,.T.);
#6317=ORIENTED_EDGE('',*,*,#4658,.F.);
#6318=ORIENTED_EDGE('',*,*,#4391,.F.);
#6319=ORIENTED_EDGE('',*,*,#4659,.T.);
#6320=ORIENTED_EDGE('',*,*,#4504,.T.);
#6321=ORIENTED_EDGE('',*,*,#4569,.T.);
#6322=ORIENTED_EDGE('',*,*,#4660,.T.);
#6323=ORIENTED_EDGE('',*,*,#4661,.T.);
#6324=ORIENTED_EDGE('',*,*,#4505,.T.);
#6325=ORIENTED_EDGE('',*,*,#4659,.F.);
#6326=ORIENTED_EDGE('',*,*,#4390,.F.);
#6327=ORIENTED_EDGE('',*,*,#4662,.T.);
#6328=ORIENTED_EDGE('',*,*,#4660,.F.);
#6329=ORIENTED_EDGE('',*,*,#4663,.F.);
#6330=ORIENTED_EDGE('',*,*,#4664,.F.);
#6331=ORIENTED_EDGE('',*,*,#4665,.F.);
#6332=ORIENTED_EDGE('',*,*,#4663,.T.);
#6333=ORIENTED_EDGE('',*,*,#4662,.F.);
#6334=ORIENTED_EDGE('',*,*,#4389,.F.);
#6335=ORIENTED_EDGE('',*,*,#4666,.T.);
#6336=ORIENTED_EDGE('',*,*,#4665,.T.);
#6337=ORIENTED_EDGE('',*,*,#4667,.T.);
#6338=ORIENTED_EDGE('',*,*,#4506,.T.);
#6339=ORIENTED_EDGE('',*,*,#4661,.F.);
#6340=ORIENTED_EDGE('',*,*,#4664,.T.);
#6341=ORIENTED_EDGE('',*,*,#4666,.F.);
#6342=ORIENTED_EDGE('',*,*,#4388,.F.);
#6343=ORIENTED_EDGE('',*,*,#4668,.T.);
#6344=ORIENTED_EDGE('',*,*,#4507,.T.);
#6345=ORIENTED_EDGE('',*,*,#4667,.F.);
#6346=ORIENTED_EDGE('',*,*,#4387,.F.);
#6347=ORIENTED_EDGE('',*,*,#4572,.F.);
#6348=ORIENTED_EDGE('',*,*,#4508,.T.);
#6349=ORIENTED_EDGE('',*,*,#4668,.F.);
#6350=ORIENTED_EDGE('',*,*,#4385,.F.);
#6351=ORIENTED_EDGE('',*,*,#4669,.T.);
#6352=ORIENTED_EDGE('',*,*,#4510,.T.);
#6353=ORIENTED_EDGE('',*,*,#4571,.T.);
#6354=ORIENTED_EDGE('',*,*,#4670,.T.);
#6355=ORIENTED_EDGE('',*,*,#4671,.T.);
#6356=ORIENTED_EDGE('',*,*,#4511,.T.);
#6357=ORIENTED_EDGE('',*,*,#4669,.F.);
#6358=ORIENTED_EDGE('',*,*,#4384,.F.);
#6359=ORIENTED_EDGE('',*,*,#4672,.T.);
#6360=ORIENTED_EDGE('',*,*,#4670,.F.);
#6361=ORIENTED_EDGE('',*,*,#4673,.F.);
#6362=ORIENTED_EDGE('',*,*,#4674,.F.);
#6363=ORIENTED_EDGE('',*,*,#4675,.F.);
#6364=ORIENTED_EDGE('',*,*,#4673,.T.);
#6365=ORIENTED_EDGE('',*,*,#4672,.F.);
#6366=ORIENTED_EDGE('',*,*,#4383,.F.);
#6367=ORIENTED_EDGE('',*,*,#4676,.T.);
#6368=ORIENTED_EDGE('',*,*,#4675,.T.);
#6369=ORIENTED_EDGE('',*,*,#4677,.T.);
#6370=ORIENTED_EDGE('',*,*,#4512,.T.);
#6371=ORIENTED_EDGE('',*,*,#4671,.F.);
#6372=ORIENTED_EDGE('',*,*,#4674,.T.);
#6373=ORIENTED_EDGE('',*,*,#4676,.F.);
#6374=ORIENTED_EDGE('',*,*,#4382,.F.);
#6375=ORIENTED_EDGE('',*,*,#4678,.T.);
#6376=ORIENTED_EDGE('',*,*,#4513,.T.);
#6377=ORIENTED_EDGE('',*,*,#4677,.F.);
#6378=ORIENTED_EDGE('',*,*,#4381,.F.);
#6379=ORIENTED_EDGE('',*,*,#4574,.F.);
#6380=ORIENTED_EDGE('',*,*,#4514,.T.);
#6381=ORIENTED_EDGE('',*,*,#4678,.F.);
#6382=ORIENTED_EDGE('',*,*,#4379,.F.);
#6383=ORIENTED_EDGE('',*,*,#4679,.T.);
#6384=ORIENTED_EDGE('',*,*,#4516,.T.);
#6385=ORIENTED_EDGE('',*,*,#4573,.T.);
#6386=ORIENTED_EDGE('',*,*,#4680,.T.);
#6387=ORIENTED_EDGE('',*,*,#4681,.T.);
#6388=ORIENTED_EDGE('',*,*,#4517,.T.);
#6389=ORIENTED_EDGE('',*,*,#4679,.F.);
#6390=ORIENTED_EDGE('',*,*,#4378,.F.);
#6391=ORIENTED_EDGE('',*,*,#4682,.T.);
#6392=ORIENTED_EDGE('',*,*,#4680,.F.);
#6393=ORIENTED_EDGE('',*,*,#4683,.F.);
#6394=ORIENTED_EDGE('',*,*,#4684,.F.);
#6395=ORIENTED_EDGE('',*,*,#4685,.F.);
#6396=ORIENTED_EDGE('',*,*,#4683,.T.);
#6397=ORIENTED_EDGE('',*,*,#4682,.F.);
#6398=ORIENTED_EDGE('',*,*,#4377,.F.);
#6399=ORIENTED_EDGE('',*,*,#4686,.T.);
#6400=ORIENTED_EDGE('',*,*,#4685,.T.);
#6401=ORIENTED_EDGE('',*,*,#4687,.T.);
#6402=ORIENTED_EDGE('',*,*,#4518,.T.);
#6403=ORIENTED_EDGE('',*,*,#4681,.F.);
#6404=ORIENTED_EDGE('',*,*,#4684,.T.);
#6405=ORIENTED_EDGE('',*,*,#4686,.F.);
#6406=ORIENTED_EDGE('',*,*,#4376,.F.);
#6407=ORIENTED_EDGE('',*,*,#4688,.T.);
#6408=ORIENTED_EDGE('',*,*,#4519,.T.);
#6409=ORIENTED_EDGE('',*,*,#4687,.F.);
#6410=ORIENTED_EDGE('',*,*,#4375,.F.);
#6411=ORIENTED_EDGE('',*,*,#4576,.F.);
#6412=ORIENTED_EDGE('',*,*,#4520,.T.);
#6413=ORIENTED_EDGE('',*,*,#4688,.F.);
#6414=ORIENTED_EDGE('',*,*,#4373,.F.);
#6415=ORIENTED_EDGE('',*,*,#4689,.T.);
#6416=ORIENTED_EDGE('',*,*,#4522,.T.);
#6417=ORIENTED_EDGE('',*,*,#4575,.T.);
#6418=ORIENTED_EDGE('',*,*,#4690,.T.);
#6419=ORIENTED_EDGE('',*,*,#4691,.T.);
#6420=ORIENTED_EDGE('',*,*,#4523,.T.);
#6421=ORIENTED_EDGE('',*,*,#4689,.F.);
#6422=ORIENTED_EDGE('',*,*,#4372,.F.);
#6423=ORIENTED_EDGE('',*,*,#4692,.T.);
#6424=ORIENTED_EDGE('',*,*,#4690,.F.);
#6425=ORIENTED_EDGE('',*,*,#4693,.F.);
#6426=ORIENTED_EDGE('',*,*,#4694,.F.);
#6427=ORIENTED_EDGE('',*,*,#4695,.F.);
#6428=ORIENTED_EDGE('',*,*,#4693,.T.);
#6429=ORIENTED_EDGE('',*,*,#4692,.F.);
#6430=ORIENTED_EDGE('',*,*,#4371,.F.);
#6431=ORIENTED_EDGE('',*,*,#4696,.T.);
#6432=ORIENTED_EDGE('',*,*,#4695,.T.);
#6433=ORIENTED_EDGE('',*,*,#4697,.T.);
#6434=ORIENTED_EDGE('',*,*,#4524,.T.);
#6435=ORIENTED_EDGE('',*,*,#4691,.F.);
#6436=ORIENTED_EDGE('',*,*,#4694,.T.);
#6437=ORIENTED_EDGE('',*,*,#4696,.F.);
#6438=ORIENTED_EDGE('',*,*,#4370,.F.);
#6439=ORIENTED_EDGE('',*,*,#4698,.T.);
#6440=ORIENTED_EDGE('',*,*,#4525,.T.);
#6441=ORIENTED_EDGE('',*,*,#4697,.F.);
#6442=ORIENTED_EDGE('',*,*,#4369,.F.);
#6443=ORIENTED_EDGE('',*,*,#4578,.F.);
#6444=ORIENTED_EDGE('',*,*,#4526,.T.);
#6445=ORIENTED_EDGE('',*,*,#4698,.F.);
#6446=ORIENTED_EDGE('',*,*,#4367,.F.);
#6447=ORIENTED_EDGE('',*,*,#4699,.T.);
#6448=ORIENTED_EDGE('',*,*,#4528,.T.);
#6449=ORIENTED_EDGE('',*,*,#4577,.T.);
#6450=ORIENTED_EDGE('',*,*,#4700,.T.);
#6451=ORIENTED_EDGE('',*,*,#4701,.T.);
#6452=ORIENTED_EDGE('',*,*,#4529,.T.);
#6453=ORIENTED_EDGE('',*,*,#4699,.F.);
#6454=ORIENTED_EDGE('',*,*,#4366,.F.);
#6455=ORIENTED_EDGE('',*,*,#4702,.T.);
#6456=ORIENTED_EDGE('',*,*,#4700,.F.);
#6457=ORIENTED_EDGE('',*,*,#4703,.F.);
#6458=ORIENTED_EDGE('',*,*,#4704,.F.);
#6459=ORIENTED_EDGE('',*,*,#4705,.F.);
#6460=ORIENTED_EDGE('',*,*,#4703,.T.);
#6461=ORIENTED_EDGE('',*,*,#4702,.F.);
#6462=ORIENTED_EDGE('',*,*,#4365,.F.);
#6463=ORIENTED_EDGE('',*,*,#4706,.T.);
#6464=ORIENTED_EDGE('',*,*,#4705,.T.);
#6465=ORIENTED_EDGE('',*,*,#4707,.T.);
#6466=ORIENTED_EDGE('',*,*,#4530,.T.);
#6467=ORIENTED_EDGE('',*,*,#4701,.F.);
#6468=ORIENTED_EDGE('',*,*,#4704,.T.);
#6469=ORIENTED_EDGE('',*,*,#4706,.F.);
#6470=ORIENTED_EDGE('',*,*,#4364,.F.);
#6471=ORIENTED_EDGE('',*,*,#4708,.T.);
#6472=ORIENTED_EDGE('',*,*,#4531,.T.);
#6473=ORIENTED_EDGE('',*,*,#4707,.F.);
#6474=ORIENTED_EDGE('',*,*,#4363,.F.);
#6475=ORIENTED_EDGE('',*,*,#4580,.F.);
#6476=ORIENTED_EDGE('',*,*,#4532,.T.);
#6477=ORIENTED_EDGE('',*,*,#4708,.F.);
#6478=ORIENTED_EDGE('',*,*,#4361,.F.);
#6479=ORIENTED_EDGE('',*,*,#4709,.T.);
#6480=ORIENTED_EDGE('',*,*,#4534,.T.);
#6481=ORIENTED_EDGE('',*,*,#4579,.T.);
#6482=ORIENTED_EDGE('',*,*,#4710,.T.);
#6483=ORIENTED_EDGE('',*,*,#4711,.T.);
#6484=ORIENTED_EDGE('',*,*,#4535,.T.);
#6485=ORIENTED_EDGE('',*,*,#4709,.F.);
#6486=ORIENTED_EDGE('',*,*,#4360,.F.);
#6487=ORIENTED_EDGE('',*,*,#4712,.T.);
#6488=ORIENTED_EDGE('',*,*,#4710,.F.);
#6489=ORIENTED_EDGE('',*,*,#4713,.F.);
#6490=ORIENTED_EDGE('',*,*,#4714,.F.);
#6491=ORIENTED_EDGE('',*,*,#4715,.F.);
#6492=ORIENTED_EDGE('',*,*,#4713,.T.);
#6493=ORIENTED_EDGE('',*,*,#4712,.F.);
#6494=ORIENTED_EDGE('',*,*,#4359,.F.);
#6495=ORIENTED_EDGE('',*,*,#4716,.T.);
#6496=ORIENTED_EDGE('',*,*,#4715,.T.);
#6497=ORIENTED_EDGE('',*,*,#4717,.T.);
#6498=ORIENTED_EDGE('',*,*,#4536,.T.);
#6499=ORIENTED_EDGE('',*,*,#4711,.F.);
#6500=ORIENTED_EDGE('',*,*,#4714,.T.);
#6501=ORIENTED_EDGE('',*,*,#4716,.F.);
#6502=ORIENTED_EDGE('',*,*,#4358,.F.);
#6503=ORIENTED_EDGE('',*,*,#4718,.T.);
#6504=ORIENTED_EDGE('',*,*,#4537,.T.);
#6505=ORIENTED_EDGE('',*,*,#4717,.F.);
#6506=ORIENTED_EDGE('',*,*,#4357,.F.);
#6507=ORIENTED_EDGE('',*,*,#4582,.F.);
#6508=ORIENTED_EDGE('',*,*,#4538,.T.);
#6509=ORIENTED_EDGE('',*,*,#4718,.F.);
#6510=ORIENTED_EDGE('',*,*,#4355,.F.);
#6511=ORIENTED_EDGE('',*,*,#4719,.T.);
#6512=ORIENTED_EDGE('',*,*,#4540,.T.);
#6513=ORIENTED_EDGE('',*,*,#4581,.T.);
#6514=ORIENTED_EDGE('',*,*,#4720,.T.);
#6515=ORIENTED_EDGE('',*,*,#4721,.T.);
#6516=ORIENTED_EDGE('',*,*,#4541,.T.);
#6517=ORIENTED_EDGE('',*,*,#4719,.F.);
#6518=ORIENTED_EDGE('',*,*,#4354,.F.);
#6519=ORIENTED_EDGE('',*,*,#4722,.T.);
#6520=ORIENTED_EDGE('',*,*,#4720,.F.);
#6521=ORIENTED_EDGE('',*,*,#4723,.F.);
#6522=ORIENTED_EDGE('',*,*,#4724,.F.);
#6523=ORIENTED_EDGE('',*,*,#4725,.F.);
#6524=ORIENTED_EDGE('',*,*,#4723,.T.);
#6525=ORIENTED_EDGE('',*,*,#4722,.F.);
#6526=ORIENTED_EDGE('',*,*,#4353,.F.);
#6527=ORIENTED_EDGE('',*,*,#4726,.T.);
#6528=ORIENTED_EDGE('',*,*,#4725,.T.);
#6529=ORIENTED_EDGE('',*,*,#4727,.T.);
#6530=ORIENTED_EDGE('',*,*,#4542,.T.);
#6531=ORIENTED_EDGE('',*,*,#4721,.F.);
#6532=ORIENTED_EDGE('',*,*,#4724,.T.);
#6533=ORIENTED_EDGE('',*,*,#4726,.F.);
#6534=ORIENTED_EDGE('',*,*,#4352,.F.);
#6535=ORIENTED_EDGE('',*,*,#4728,.T.);
#6536=ORIENTED_EDGE('',*,*,#4543,.T.);
#6537=ORIENTED_EDGE('',*,*,#4727,.F.);
#6538=ORIENTED_EDGE('',*,*,#4351,.F.);
#6539=ORIENTED_EDGE('',*,*,#4584,.F.);
#6540=ORIENTED_EDGE('',*,*,#4544,.T.);
#6541=ORIENTED_EDGE('',*,*,#4728,.F.);
#6542=ORIENTED_EDGE('',*,*,#4349,.F.);
#6543=ORIENTED_EDGE('',*,*,#4729,.T.);
#6544=ORIENTED_EDGE('',*,*,#4546,.T.);
#6545=ORIENTED_EDGE('',*,*,#4583,.T.);
#6546=ORIENTED_EDGE('',*,*,#4730,.T.);
#6547=ORIENTED_EDGE('',*,*,#4731,.T.);
#6548=ORIENTED_EDGE('',*,*,#4547,.T.);
#6549=ORIENTED_EDGE('',*,*,#4729,.F.);
#6550=ORIENTED_EDGE('',*,*,#4348,.F.);
#6551=ORIENTED_EDGE('',*,*,#4732,.T.);
#6552=ORIENTED_EDGE('',*,*,#4730,.F.);
#6553=ORIENTED_EDGE('',*,*,#4733,.F.);
#6554=ORIENTED_EDGE('',*,*,#4734,.F.);
#6555=ORIENTED_EDGE('',*,*,#4735,.F.);
#6556=ORIENTED_EDGE('',*,*,#4733,.T.);
#6557=ORIENTED_EDGE('',*,*,#4732,.F.);
#6558=ORIENTED_EDGE('',*,*,#4347,.F.);
#6559=ORIENTED_EDGE('',*,*,#4736,.T.);
#6560=ORIENTED_EDGE('',*,*,#4735,.T.);
#6561=ORIENTED_EDGE('',*,*,#4737,.T.);
#6562=ORIENTED_EDGE('',*,*,#4548,.T.);
#6563=ORIENTED_EDGE('',*,*,#4731,.F.);
#6564=ORIENTED_EDGE('',*,*,#4734,.T.);
#6565=ORIENTED_EDGE('',*,*,#4736,.F.);
#6566=ORIENTED_EDGE('',*,*,#4346,.F.);
#6567=ORIENTED_EDGE('',*,*,#4738,.T.);
#6568=ORIENTED_EDGE('',*,*,#4549,.T.);
#6569=ORIENTED_EDGE('',*,*,#4737,.F.);
#6570=ORIENTED_EDGE('',*,*,#4345,.F.);
#6571=ORIENTED_EDGE('',*,*,#4588,.F.);
#6572=ORIENTED_EDGE('',*,*,#4550,.T.);
#6573=ORIENTED_EDGE('',*,*,#4738,.F.);
#6574=ORIENTED_EDGE('',*,*,#4435,.F.);
#6575=ORIENTED_EDGE('',*,*,#4585,.F.);
#6576=ORIENTED_EDGE('',*,*,#4556,.T.);
#6577=ORIENTED_EDGE('',*,*,#4739,.F.);
#6578=ORIENTED_EDGE('',*,*,#4740,.T.);
#6579=ORIENTED_EDGE('',*,*,#4741,.F.);
#6580=ORIENTED_EDGE('',*,*,#4436,.F.);
#6581=ORIENTED_EDGE('',*,*,#4739,.T.);
#6582=ORIENTED_EDGE('',*,*,#4555,.T.);
#6583=ORIENTED_EDGE('',*,*,#4742,.F.);
#6584=ORIENTED_EDGE('',*,*,#4743,.F.);
#6585=ORIENTED_EDGE('',*,*,#4744,.F.);
#6586=ORIENTED_EDGE('',*,*,#4740,.F.);
#6587=ORIENTED_EDGE('',*,*,#4745,.F.);
#6588=ORIENTED_EDGE('',*,*,#4743,.T.);
#6589=ORIENTED_EDGE('',*,*,#4746,.T.);
#6590=ORIENTED_EDGE('',*,*,#4553,.T.);
#6591=ORIENTED_EDGE('',*,*,#4747,.F.);
#6592=ORIENTED_EDGE('',*,*,#4438,.F.);
#6593=ORIENTED_EDGE('',*,*,#4748,.T.);
#6594=ORIENTED_EDGE('',*,*,#4744,.T.);
#6595=ORIENTED_EDGE('',*,*,#4748,.F.);
#6596=ORIENTED_EDGE('',*,*,#4437,.F.);
#6597=ORIENTED_EDGE('',*,*,#4741,.T.);
#6598=ORIENTED_EDGE('',*,*,#4745,.T.);
#6599=ORIENTED_EDGE('',*,*,#4742,.T.);
#6600=ORIENTED_EDGE('',*,*,#4554,.T.);
#6601=ORIENTED_EDGE('',*,*,#4746,.F.);
#6602=ORIENTED_EDGE('',*,*,#4439,.F.);
#6603=ORIENTED_EDGE('',*,*,#4747,.T.);
#6604=ORIENTED_EDGE('',*,*,#4552,.T.);
#6605=ORIENTED_EDGE('',*,*,#4587,.T.);
#6606=ORIENTED_EDGE('',*,*,#4749,.F.);
#6607=ORIENTED_EDGE('',*,*,#4750,.F.);
#6608=ORIENTED_EDGE('',*,*,#4751,.F.);
#6609=ORIENTED_EDGE('',*,*,#4752,.F.);
#6610=ORIENTED_EDGE('',*,*,#4753,.F.);
#6611=ORIENTED_EDGE('',*,*,#4754,.F.);
#6612=ORIENTED_EDGE('',*,*,#4755,.F.);
#6613=ORIENTED_EDGE('',*,*,#4749,.T.);
#6614=ORIENTED_EDGE('',*,*,#4756,.T.);
#6615=ORIENTED_EDGE('',*,*,#4757,.T.);
#6616=ORIENTED_EDGE('',*,*,#4756,.F.);
#6617=ORIENTED_EDGE('',*,*,#4758,.F.);
#6618=ORIENTED_EDGE('',*,*,#4759,.T.);
#6619=ORIENTED_EDGE('',*,*,#4760,.T.);
#6620=ORIENTED_EDGE('',*,*,#4759,.F.);
#6621=ORIENTED_EDGE('',*,*,#4757,.F.);
#6622=ORIENTED_EDGE('',*,*,#4761,.T.);
#6623=ORIENTED_EDGE('',*,*,#4758,.T.);
#6624=ORIENTED_EDGE('',*,*,#4761,.F.);
#6625=ORIENTED_EDGE('',*,*,#4762,.T.);
#6626=ORIENTED_EDGE('',*,*,#4763,.T.);
#6627=ORIENTED_EDGE('',*,*,#4764,.T.);
#6628=ORIENTED_EDGE('',*,*,#4760,.F.);
#6629=ORIENTED_EDGE('',*,*,#4765,.T.);
#6630=ORIENTED_EDGE('',*,*,#4765,.F.);
#6631=ORIENTED_EDGE('',*,*,#4763,.F.);
#6632=ORIENTED_EDGE('',*,*,#4764,.F.);
#6633=ORIENTED_EDGE('',*,*,#4766,.T.);
#6634=ORIENTED_EDGE('',*,*,#4762,.F.);
#6635=ORIENTED_EDGE('',*,*,#4766,.F.);
#6636=ORIENTED_EDGE('',*,*,#4750,.T.);
#6637=ORIENTED_EDGE('',*,*,#4767,.T.);
#6638=ORIENTED_EDGE('',*,*,#4768,.F.);
#6639=ORIENTED_EDGE('',*,*,#4769,.F.);
#6640=ORIENTED_EDGE('',*,*,#4751,.T.);
#6641=ORIENTED_EDGE('',*,*,#4769,.T.);
#6642=ORIENTED_EDGE('',*,*,#4770,.F.);
#6643=ORIENTED_EDGE('',*,*,#4771,.F.);
#6644=ORIENTED_EDGE('',*,*,#4752,.T.);
#6645=ORIENTED_EDGE('',*,*,#4771,.T.);
#6646=ORIENTED_EDGE('',*,*,#4772,.F.);
#6647=ORIENTED_EDGE('',*,*,#4773,.F.);
#6648=ORIENTED_EDGE('',*,*,#4753,.T.);
#6649=ORIENTED_EDGE('',*,*,#4773,.T.);
#6650=ORIENTED_EDGE('',*,*,#4774,.F.);
#6651=ORIENTED_EDGE('',*,*,#4775,.F.);
#6652=ORIENTED_EDGE('',*,*,#4754,.T.);
#6653=ORIENTED_EDGE('',*,*,#4775,.T.);
#6654=ORIENTED_EDGE('',*,*,#4776,.F.);
#6655=ORIENTED_EDGE('',*,*,#4777,.F.);
#6656=ORIENTED_EDGE('',*,*,#4755,.T.);
#6657=ORIENTED_EDGE('',*,*,#4777,.T.);
#6658=ORIENTED_EDGE('',*,*,#4778,.F.);
#6659=ORIENTED_EDGE('',*,*,#4767,.F.);
#6660=ORIENTED_EDGE('',*,*,#4768,.T.);
#6661=ORIENTED_EDGE('',*,*,#4778,.T.);
#6662=ORIENTED_EDGE('',*,*,#4776,.T.);
#6663=ORIENTED_EDGE('',*,*,#4774,.T.);
#6664=ORIENTED_EDGE('',*,*,#4772,.T.);
#6665=ORIENTED_EDGE('',*,*,#4770,.T.);
#6666=ORIENTED_EDGE('',*,*,#4779,.F.);
#6667=ORIENTED_EDGE('',*,*,#4780,.F.);
#6668=ORIENTED_EDGE('',*,*,#4781,.T.);
#6669=ORIENTED_EDGE('',*,*,#4782,.F.);
#6670=ORIENTED_EDGE('',*,*,#4783,.F.);
#6671=ORIENTED_EDGE('',*,*,#4784,.F.);
#6672=ORIENTED_EDGE('',*,*,#4780,.T.);
#6673=ORIENTED_EDGE('',*,*,#4785,.F.);
#6674=ORIENTED_EDGE('',*,*,#4786,.T.);
#6675=ORIENTED_EDGE('',*,*,#4784,.T.);
#6676=ORIENTED_EDGE('',*,*,#4787,.F.);
#6677=ORIENTED_EDGE('',*,*,#4788,.T.);
#6678=ORIENTED_EDGE('',*,*,#4789,.T.);
#6679=ORIENTED_EDGE('',*,*,#4785,.T.);
#6680=ORIENTED_EDGE('',*,*,#4779,.T.);
#6681=ORIENTED_EDGE('',*,*,#4782,.T.);
#6682=ORIENTED_EDGE('',*,*,#4790,.F.);
#6683=ORIENTED_EDGE('',*,*,#4789,.F.);
#6684=ORIENTED_EDGE('',*,*,#4791,.T.);
#6685=ORIENTED_EDGE('',*,*,#4792,.T.);
#6686=ORIENTED_EDGE('',*,*,#4793,.T.);
#6687=ORIENTED_EDGE('',*,*,#4783,.T.);
#6688=ORIENTED_EDGE('',*,*,#4793,.F.);
#6689=ORIENTED_EDGE('',*,*,#4794,.T.);
#6690=ORIENTED_EDGE('',*,*,#4787,.T.);
#6691=ORIENTED_EDGE('',*,*,#4795,.T.);
#6692=ORIENTED_EDGE('',*,*,#4796,.T.);
#6693=ORIENTED_EDGE('',*,*,#4794,.F.);
#6694=ORIENTED_EDGE('',*,*,#4797,.F.);
#6695=ORIENTED_EDGE('',*,*,#4798,.T.);
#6696=ORIENTED_EDGE('',*,*,#4799,.T.);
#6697=ORIENTED_EDGE('',*,*,#4795,.F.);
#6698=ORIENTED_EDGE('',*,*,#4800,.F.);
#6699=ORIENTED_EDGE('',*,*,#4801,.T.);
#6700=ORIENTED_EDGE('',*,*,#4802,.T.);
#6701=ORIENTED_EDGE('',*,*,#4798,.F.);
#6702=ORIENTED_EDGE('',*,*,#4803,.F.);
#6703=ORIENTED_EDGE('',*,*,#4804,.T.);
#6704=ORIENTED_EDGE('',*,*,#4805,.T.);
#6705=ORIENTED_EDGE('',*,*,#4801,.F.);
#6706=ORIENTED_EDGE('',*,*,#4806,.F.);
#6707=ORIENTED_EDGE('',*,*,#4807,.F.);
#6708=ORIENTED_EDGE('',*,*,#4808,.T.);
#6709=ORIENTED_EDGE('',*,*,#4809,.F.);
#6710=ORIENTED_EDGE('',*,*,#4804,.F.);
#6711=ORIENTED_EDGE('',*,*,#4810,.F.);
#6712=ORIENTED_EDGE('',*,*,#4811,.F.);
#6713=ORIENTED_EDGE('',*,*,#4812,.T.);
#6714=ORIENTED_EDGE('',*,*,#4813,.T.);
#6715=ORIENTED_EDGE('',*,*,#4807,.T.);
#6716=ORIENTED_EDGE('',*,*,#4811,.T.);
#6717=ORIENTED_EDGE('',*,*,#4810,.T.);
#6718=ORIENTED_EDGE('',*,*,#4806,.T.);
#6719=ORIENTED_EDGE('',*,*,#4814,.F.);
#6720=ORIENTED_EDGE('',*,*,#4815,.F.);
#6721=ORIENTED_EDGE('',*,*,#4816,.T.);
#6722=ORIENTED_EDGE('',*,*,#4812,.F.);
#6723=ORIENTED_EDGE('',*,*,#4813,.F.);
#6724=ORIENTED_EDGE('',*,*,#4816,.F.);
#6725=ORIENTED_EDGE('',*,*,#4808,.F.);
#6726=ORIENTED_EDGE('',*,*,#4815,.T.);
#6727=ORIENTED_EDGE('',*,*,#4817,.T.);
#6728=ORIENTED_EDGE('',*,*,#4818,.F.);
#6729=ORIENTED_EDGE('',*,*,#4805,.F.);
#6730=ORIENTED_EDGE('',*,*,#4809,.T.);
#6731=ORIENTED_EDGE('',*,*,#4819,.T.);
#6732=ORIENTED_EDGE('',*,*,#4820,.T.);
#6733=ORIENTED_EDGE('',*,*,#4821,.F.);
#6734=ORIENTED_EDGE('',*,*,#4802,.F.);
#6735=ORIENTED_EDGE('',*,*,#4818,.T.);
#6736=ORIENTED_EDGE('',*,*,#4817,.F.);
#6737=ORIENTED_EDGE('',*,*,#4814,.T.);
#6738=ORIENTED_EDGE('',*,*,#4803,.T.);
#6739=ORIENTED_EDGE('',*,*,#4822,.F.);
#6740=ORIENTED_EDGE('',*,*,#4819,.F.);
#6741=ORIENTED_EDGE('',*,*,#4820,.F.);
#6742=ORIENTED_EDGE('',*,*,#4822,.T.);
#6743=ORIENTED_EDGE('',*,*,#4800,.T.);
#6744=ORIENTED_EDGE('',*,*,#4823,.F.);
#6745=ORIENTED_EDGE('',*,*,#4824,.F.);
#6746=ORIENTED_EDGE('',*,*,#4824,.T.);
#6747=ORIENTED_EDGE('',*,*,#4825,.T.);
#6748=ORIENTED_EDGE('',*,*,#4826,.F.);
#6749=ORIENTED_EDGE('',*,*,#4799,.F.);
#6750=ORIENTED_EDGE('',*,*,#4821,.T.);
#6751=ORIENTED_EDGE('',*,*,#4827,.T.);
#6752=ORIENTED_EDGE('',*,*,#4791,.F.);
#6753=ORIENTED_EDGE('',*,*,#4788,.F.);
#6754=ORIENTED_EDGE('',*,*,#4796,.F.);
#6755=ORIENTED_EDGE('',*,*,#4826,.T.);
#6756=ORIENTED_EDGE('',*,*,#4825,.F.);
#6757=ORIENTED_EDGE('',*,*,#4823,.T.);
#6758=ORIENTED_EDGE('',*,*,#4797,.T.);
#6759=ORIENTED_EDGE('',*,*,#4792,.F.);
#6760=ORIENTED_EDGE('',*,*,#4827,.F.);
#6761=ORIENTED_EDGE('',*,*,#4781,.F.);
#6762=ORIENTED_EDGE('',*,*,#4786,.F.);
#6763=ORIENTED_EDGE('',*,*,#4790,.T.);
#6764=ORIENTED_EDGE('',*,*,#4828,.T.);
#6765=ORIENTED_EDGE('',*,*,#4829,.F.);
#6766=ORIENTED_EDGE('',*,*,#4829,.T.);
#6767=ORIENTED_EDGE('',*,*,#4830,.T.);
#6768=ORIENTED_EDGE('',*,*,#4831,.F.);
#6769=ORIENTED_EDGE('',*,*,#4830,.F.);
#6770=ORIENTED_EDGE('',*,*,#4832,.T.);
#6771=ORIENTED_EDGE('',*,*,#4831,.T.);
#6772=ORIENTED_EDGE('',*,*,#4832,.F.);
#6773=ORIENTED_EDGE('',*,*,#4833,.T.);
#6774=ORIENTED_EDGE('',*,*,#4828,.F.);
#6775=ORIENTED_EDGE('',*,*,#4833,.F.);
#6776=ORIENTED_EDGE('',*,*,#4834,.F.);
#6777=ORIENTED_EDGE('',*,*,#4835,.F.);
#6778=ORIENTED_EDGE('',*,*,#4836,.T.);
#6779=ORIENTED_EDGE('',*,*,#4837,.T.);
#6780=ORIENTED_EDGE('',*,*,#4838,.T.);
#6781=ORIENTED_EDGE('',*,*,#4837,.F.);
#6782=ORIENTED_EDGE('',*,*,#4839,.F.);
#6783=ORIENTED_EDGE('',*,*,#4840,.T.);
#6784=ORIENTED_EDGE('',*,*,#4841,.F.);
#6785=ORIENTED_EDGE('',*,*,#4842,.F.);
#6786=ORIENTED_EDGE('',*,*,#4839,.T.);
#6787=ORIENTED_EDGE('',*,*,#4838,.F.);
#6788=ORIENTED_EDGE('',*,*,#4842,.T.);
#6789=ORIENTED_EDGE('',*,*,#4843,.T.);
#6790=ORIENTED_EDGE('',*,*,#4844,.T.);
#6791=ORIENTED_EDGE('',*,*,#4845,.F.);
#6792=ORIENTED_EDGE('',*,*,#4846,.T.);
#6793=ORIENTED_EDGE('',*,*,#4845,.T.);
#6794=ORIENTED_EDGE('',*,*,#4847,.T.);
#6795=ORIENTED_EDGE('',*,*,#4848,.T.);
#6796=ORIENTED_EDGE('',*,*,#4849,.F.);
#6797=ORIENTED_EDGE('',*,*,#4850,.F.);
#6798=ORIENTED_EDGE('',*,*,#4851,.F.);
#6799=ORIENTED_EDGE('',*,*,#4840,.F.);
#6800=ORIENTED_EDGE('',*,*,#4846,.F.);
#6801=ORIENTED_EDGE('',*,*,#4851,.T.);
#6802=ORIENTED_EDGE('',*,*,#4850,.T.);
#6803=ORIENTED_EDGE('',*,*,#4849,.T.);
#6804=ORIENTED_EDGE('',*,*,#4852,.T.);
#6805=ORIENTED_EDGE('',*,*,#4843,.F.);
#6806=ORIENTED_EDGE('',*,*,#4841,.T.);
#6807=ORIENTED_EDGE('',*,*,#4848,.F.);
#6808=ORIENTED_EDGE('',*,*,#4853,.T.);
#6809=ORIENTED_EDGE('',*,*,#4854,.T.);
#6810=ORIENTED_EDGE('',*,*,#4855,.F.);
#6811=ORIENTED_EDGE('',*,*,#4852,.F.);
#6812=ORIENTED_EDGE('',*,*,#4844,.F.);
#6813=ORIENTED_EDGE('',*,*,#4855,.T.);
#6814=ORIENTED_EDGE('',*,*,#4856,.T.);
#6815=ORIENTED_EDGE('',*,*,#4857,.F.);
#6816=ORIENTED_EDGE('',*,*,#4853,.F.);
#6817=ORIENTED_EDGE('',*,*,#4847,.F.);
#6818=ORIENTED_EDGE('',*,*,#4857,.T.);
#6819=ORIENTED_EDGE('',*,*,#4858,.T.);
#6820=ORIENTED_EDGE('',*,*,#4859,.T.);
#6821=ORIENTED_EDGE('',*,*,#4859,.F.);
#6822=ORIENTED_EDGE('',*,*,#4860,.T.);
#6823=ORIENTED_EDGE('',*,*,#4861,.T.);
#6824=ORIENTED_EDGE('',*,*,#4862,.F.);
#6825=ORIENTED_EDGE('',*,*,#4854,.F.);
#6826=ORIENTED_EDGE('',*,*,#4856,.F.);
#6827=ORIENTED_EDGE('',*,*,#4862,.T.);
#6828=ORIENTED_EDGE('',*,*,#4863,.T.);
#6829=ORIENTED_EDGE('',*,*,#4864,.F.);
#6830=ORIENTED_EDGE('',*,*,#4860,.F.);
#6831=ORIENTED_EDGE('',*,*,#4858,.F.);
#6832=ORIENTED_EDGE('',*,*,#4864,.T.);
#6833=ORIENTED_EDGE('',*,*,#4865,.T.);
#6834=ORIENTED_EDGE('',*,*,#4866,.T.);
#6835=ORIENTED_EDGE('',*,*,#4867,.T.);
#6836=ORIENTED_EDGE('',*,*,#4868,.F.);
#6837=ORIENTED_EDGE('',*,*,#4869,.F.);
#6838=ORIENTED_EDGE('',*,*,#4870,.T.);
#6839=ORIENTED_EDGE('',*,*,#4871,.F.);
#6840=ORIENTED_EDGE('',*,*,#4861,.F.);
#6841=ORIENTED_EDGE('',*,*,#4866,.F.);
#6842=ORIENTED_EDGE('',*,*,#4872,.F.);
#6843=ORIENTED_EDGE('',*,*,#4873,.T.);
#6844=ORIENTED_EDGE('',*,*,#4835,.T.);
#6845=ORIENTED_EDGE('',*,*,#4874,.T.);
#6846=ORIENTED_EDGE('',*,*,#4868,.T.);
#6847=ORIENTED_EDGE('',*,*,#4867,.F.);
#6848=ORIENTED_EDGE('',*,*,#4865,.F.);
#6849=ORIENTED_EDGE('',*,*,#4875,.T.);
#6850=ORIENTED_EDGE('',*,*,#4876,.T.);
#6851=ORIENTED_EDGE('',*,*,#4836,.F.);
#6852=ORIENTED_EDGE('',*,*,#4873,.F.);
#6853=ORIENTED_EDGE('',*,*,#4872,.T.);
#6854=ORIENTED_EDGE('',*,*,#4877,.F.);
#6855=ORIENTED_EDGE('',*,*,#4878,.F.);
#6856=ORIENTED_EDGE('',*,*,#4879,.T.);
#6857=ORIENTED_EDGE('',*,*,#4880,.T.);
#6858=ORIENTED_EDGE('',*,*,#4879,.F.);
#6859=ORIENTED_EDGE('',*,*,#4834,.T.);
#6860=ORIENTED_EDGE('',*,*,#4878,.T.);
#6861=ORIENTED_EDGE('',*,*,#4881,.T.);
#6862=ORIENTED_EDGE('',*,*,#4869,.T.);
#6863=ORIENTED_EDGE('',*,*,#4874,.F.);
#6864=ORIENTED_EDGE('',*,*,#4870,.F.);
#6865=ORIENTED_EDGE('',*,*,#4881,.F.);
#6866=ORIENTED_EDGE('',*,*,#4877,.T.);
#6867=ORIENTED_EDGE('',*,*,#4876,.F.);
#6868=ORIENTED_EDGE('',*,*,#4882,.F.);
#6869=ORIENTED_EDGE('',*,*,#4863,.F.);
#6870=ORIENTED_EDGE('',*,*,#4871,.T.);
#6871=ORIENTED_EDGE('',*,*,#4882,.T.);
#6872=ORIENTED_EDGE('',*,*,#4875,.F.);
#6873=ORIENTED_EDGE('',*,*,#4883,.T.);
#6874=ORIENTED_EDGE('',*,*,#4880,.F.);
#6875=ORIENTED_EDGE('',*,*,#4883,.F.);
#6876=ORIENTED_EDGE('',*,*,#4884,.T.);
#6877=ORIENTED_EDGE('',*,*,#4885,.T.);
#6878=ORIENTED_EDGE('',*,*,#4886,.T.);
#6879=ORIENTED_EDGE('',*,*,#4884,.F.);
#6880=ORIENTED_EDGE('',*,*,#4887,.T.);
#6881=ORIENTED_EDGE('',*,*,#4888,.T.);
#6882=ORIENTED_EDGE('',*,*,#4889,.T.);
#6883=ORIENTED_EDGE('',*,*,#4890,.F.);
#6884=ORIENTED_EDGE('',*,*,#4891,.T.);
#6885=ORIENTED_EDGE('',*,*,#4892,.T.);
#6886=ORIENTED_EDGE('',*,*,#4893,.T.);
#6887=ORIENTED_EDGE('',*,*,#4894,.T.);
#6888=ORIENTED_EDGE('',*,*,#4885,.F.);
#6889=ORIENTED_EDGE('',*,*,#4886,.F.);
#6890=ORIENTED_EDGE('',*,*,#4894,.F.);
#6891=ORIENTED_EDGE('',*,*,#4895,.T.);
#6892=ORIENTED_EDGE('',*,*,#4896,.T.);
#6893=ORIENTED_EDGE('',*,*,#4897,.T.);
#6894=ORIENTED_EDGE('',*,*,#4898,.F.);
#6895=ORIENTED_EDGE('',*,*,#4899,.T.);
#6896=ORIENTED_EDGE('',*,*,#4900,.T.);
#6897=ORIENTED_EDGE('',*,*,#4901,.T.);
#6898=ORIENTED_EDGE('',*,*,#4902,.T.);
#6899=ORIENTED_EDGE('',*,*,#4903,.T.);
#6900=ORIENTED_EDGE('',*,*,#4904,.T.);
#6901=ORIENTED_EDGE('',*,*,#4905,.T.);
#6902=ORIENTED_EDGE('',*,*,#4906,.T.);
#6903=ORIENTED_EDGE('',*,*,#4907,.T.);
#6904=ORIENTED_EDGE('',*,*,#4908,.T.);
#6905=ORIENTED_EDGE('',*,*,#4909,.T.);
#6906=ORIENTED_EDGE('',*,*,#4910,.T.);
#6907=ORIENTED_EDGE('',*,*,#4911,.T.);
#6908=ORIENTED_EDGE('',*,*,#4912,.T.);
#6909=ORIENTED_EDGE('',*,*,#4913,.T.);
#6910=ORIENTED_EDGE('',*,*,#4914,.F.);
#6911=ORIENTED_EDGE('',*,*,#4915,.F.);
#6912=ORIENTED_EDGE('',*,*,#4895,.F.);
#6913=ORIENTED_EDGE('',*,*,#4893,.F.);
#6914=ORIENTED_EDGE('',*,*,#4916,.F.);
#6915=ORIENTED_EDGE('',*,*,#4913,.F.);
#6916=ORIENTED_EDGE('',*,*,#4892,.F.);
#6917=ORIENTED_EDGE('',*,*,#4917,.T.);
#6918=ORIENTED_EDGE('',*,*,#4918,.T.);
#6919=ORIENTED_EDGE('',*,*,#4919,.T.);
#6920=ORIENTED_EDGE('',*,*,#4920,.T.);
#6921=ORIENTED_EDGE('',*,*,#4921,.T.);
#6922=ORIENTED_EDGE('',*,*,#4922,.T.);
#6923=ORIENTED_EDGE('',*,*,#4923,.T.);
#6924=ORIENTED_EDGE('',*,*,#4924,.T.);
#6925=ORIENTED_EDGE('',*,*,#4925,.T.);
#6926=ORIENTED_EDGE('',*,*,#4914,.T.);
#6927=ORIENTED_EDGE('',*,*,#4916,.T.);
#6928=ORIENTED_EDGE('',*,*,#4926,.T.);
#6929=ORIENTED_EDGE('',*,*,#4927,.T.);
#6930=ORIENTED_EDGE('',*,*,#4928,.T.);
#6931=ORIENTED_EDGE('',*,*,#4929,.T.);
#6932=ORIENTED_EDGE('',*,*,#4930,.T.);
#6933=ORIENTED_EDGE('',*,*,#4931,.T.);
#6934=ORIENTED_EDGE('',*,*,#4932,.T.);
#6935=ORIENTED_EDGE('',*,*,#4933,.T.);
#6936=ORIENTED_EDGE('',*,*,#4934,.T.);
#6937=ORIENTED_EDGE('',*,*,#4935,.T.);
#6938=ORIENTED_EDGE('',*,*,#4936,.T.);
#6939=ORIENTED_EDGE('',*,*,#4937,.T.);
#6940=ORIENTED_EDGE('',*,*,#4938,.T.);
#6941=ORIENTED_EDGE('',*,*,#4939,.T.);
#6942=ORIENTED_EDGE('',*,*,#4940,.T.);
#6943=ORIENTED_EDGE('',*,*,#4903,.F.);
#6944=ORIENTED_EDGE('',*,*,#4941,.T.);
#6945=ORIENTED_EDGE('',*,*,#4918,.F.);
#6946=ORIENTED_EDGE('',*,*,#4942,.T.);
#6947=ORIENTED_EDGE('',*,*,#4943,.F.);
#6948=ORIENTED_EDGE('',*,*,#4898,.T.);
#6949=ORIENTED_EDGE('',*,*,#4944,.F.);
#6950=ORIENTED_EDGE('',*,*,#4945,.T.);
#6951=ORIENTED_EDGE('',*,*,#4946,.F.);
#6952=ORIENTED_EDGE('',*,*,#4890,.T.);
#6953=ORIENTED_EDGE('',*,*,#4947,.F.);
#6954=ORIENTED_EDGE('',*,*,#4948,.T.);
#6955=ORIENTED_EDGE('',*,*,#4949,.F.);
#6956=ORIENTED_EDGE('',*,*,#4910,.F.);
#6957=ORIENTED_EDGE('',*,*,#4950,.F.);
#6958=ORIENTED_EDGE('',*,*,#4951,.T.);
#6959=ORIENTED_EDGE('',*,*,#4952,.F.);
#6960=ORIENTED_EDGE('',*,*,#4904,.F.);
#6961=ORIENTED_EDGE('',*,*,#4940,.F.);
#6962=ORIENTED_EDGE('',*,*,#4953,.T.);
#6963=ORIENTED_EDGE('',*,*,#4943,.T.);
#6964=ORIENTED_EDGE('',*,*,#4954,.F.);
#6965=ORIENTED_EDGE('',*,*,#4922,.F.);
#6966=ORIENTED_EDGE('',*,*,#4955,.F.);
#6967=ORIENTED_EDGE('',*,*,#4899,.F.);
#6968=ORIENTED_EDGE('',*,*,#4921,.F.);
#6969=ORIENTED_EDGE('',*,*,#4956,.F.);
#6970=ORIENTED_EDGE('',*,*,#4900,.F.);
#6971=ORIENTED_EDGE('',*,*,#4955,.T.);
#6972=ORIENTED_EDGE('',*,*,#4957,.F.);
#6973=ORIENTED_EDGE('',*,*,#4901,.F.);
#6974=ORIENTED_EDGE('',*,*,#4956,.T.);
#6975=ORIENTED_EDGE('',*,*,#4920,.F.);
#6976=ORIENTED_EDGE('',*,*,#4919,.F.);
#6977=ORIENTED_EDGE('',*,*,#4941,.F.);
#6978=ORIENTED_EDGE('',*,*,#4902,.F.);
#6979=ORIENTED_EDGE('',*,*,#4957,.T.);
#6980=ORIENTED_EDGE('',*,*,#4958,.T.);
#6981=ORIENTED_EDGE('',*,*,#4936,.F.);
#6982=ORIENTED_EDGE('',*,*,#4959,.F.);
#6983=ORIENTED_EDGE('',*,*,#4907,.F.);
#6984=ORIENTED_EDGE('',*,*,#4937,.F.);
#6985=ORIENTED_EDGE('',*,*,#4958,.F.);
#6986=ORIENTED_EDGE('',*,*,#4906,.F.);
#6987=ORIENTED_EDGE('',*,*,#4960,.T.);
#6988=ORIENTED_EDGE('',*,*,#4952,.T.);
#6989=ORIENTED_EDGE('',*,*,#4961,.F.);
#6990=ORIENTED_EDGE('',*,*,#4938,.F.);
#6991=ORIENTED_EDGE('',*,*,#4960,.F.);
#6992=ORIENTED_EDGE('',*,*,#4905,.F.);
#6993=ORIENTED_EDGE('',*,*,#4953,.F.);
#6994=ORIENTED_EDGE('',*,*,#4942,.F.);
#6995=ORIENTED_EDGE('',*,*,#4939,.F.);
#6996=ORIENTED_EDGE('',*,*,#4961,.T.);
#6997=ORIENTED_EDGE('',*,*,#4935,.F.);
#6998=ORIENTED_EDGE('',*,*,#4962,.F.);
#6999=ORIENTED_EDGE('',*,*,#4908,.F.);
#7000=ORIENTED_EDGE('',*,*,#4959,.T.);
#7001=ORIENTED_EDGE('',*,*,#4950,.T.);
#7002=ORIENTED_EDGE('',*,*,#4909,.F.);
#7003=ORIENTED_EDGE('',*,*,#4962,.T.);
#7004=ORIENTED_EDGE('',*,*,#4934,.F.);
#7005=ORIENTED_EDGE('',*,*,#4963,.T.);
#7006=ORIENTED_EDGE('',*,*,#4951,.F.);
#7007=ORIENTED_EDGE('',*,*,#4963,.F.);
#7008=ORIENTED_EDGE('',*,*,#4933,.F.);
#7009=ORIENTED_EDGE('',*,*,#4964,.T.);
#7010=ORIENTED_EDGE('',*,*,#4949,.T.);
#7011=ORIENTED_EDGE('',*,*,#4964,.F.);
#7012=ORIENTED_EDGE('',*,*,#4932,.F.);
#7013=ORIENTED_EDGE('',*,*,#4965,.F.);
#7014=ORIENTED_EDGE('',*,*,#4911,.F.);
#7015=ORIENTED_EDGE('',*,*,#4931,.F.);
#7016=ORIENTED_EDGE('',*,*,#4966,.F.);
#7017=ORIENTED_EDGE('',*,*,#4912,.F.);
#7018=ORIENTED_EDGE('',*,*,#4965,.T.);
#7019=ORIENTED_EDGE('',*,*,#4966,.T.);
#7020=ORIENTED_EDGE('',*,*,#4930,.F.);
#7021=ORIENTED_EDGE('',*,*,#4967,.F.);
#7022=ORIENTED_EDGE('',*,*,#4887,.F.);
#7023=ORIENTED_EDGE('',*,*,#4929,.F.);
#7024=ORIENTED_EDGE('',*,*,#4968,.F.);
#7025=ORIENTED_EDGE('',*,*,#4888,.F.);
#7026=ORIENTED_EDGE('',*,*,#4967,.T.);
#7027=ORIENTED_EDGE('',*,*,#4947,.T.);
#7028=ORIENTED_EDGE('',*,*,#4889,.F.);
#7029=ORIENTED_EDGE('',*,*,#4968,.T.);
#7030=ORIENTED_EDGE('',*,*,#4928,.F.);
#7031=ORIENTED_EDGE('',*,*,#4969,.T.);
#7032=ORIENTED_EDGE('',*,*,#4948,.F.);
#7033=ORIENTED_EDGE('',*,*,#4969,.F.);
#7034=ORIENTED_EDGE('',*,*,#4927,.F.);
#7035=ORIENTED_EDGE('',*,*,#4970,.T.);
#7036=ORIENTED_EDGE('',*,*,#4946,.T.);
#7037=ORIENTED_EDGE('',*,*,#4970,.F.);
#7038=ORIENTED_EDGE('',*,*,#4926,.F.);
#7039=ORIENTED_EDGE('',*,*,#4917,.F.);
#7040=ORIENTED_EDGE('',*,*,#4891,.F.);
#7041=ORIENTED_EDGE('',*,*,#4945,.F.);
#7042=ORIENTED_EDGE('',*,*,#4971,.F.);
#7043=ORIENTED_EDGE('',*,*,#4923,.F.);
#7044=ORIENTED_EDGE('',*,*,#4954,.T.);
#7045=ORIENTED_EDGE('',*,*,#4944,.T.);
#7046=ORIENTED_EDGE('',*,*,#4897,.F.);
#7047=ORIENTED_EDGE('',*,*,#4972,.T.);
#7048=ORIENTED_EDGE('',*,*,#4924,.F.);
#7049=ORIENTED_EDGE('',*,*,#4971,.T.);
#7050=ORIENTED_EDGE('',*,*,#4925,.F.);
#7051=ORIENTED_EDGE('',*,*,#4972,.F.);
#7052=ORIENTED_EDGE('',*,*,#4896,.F.);
#7053=ORIENTED_EDGE('',*,*,#4915,.T.);
#7054=ORIENTED_EDGE('',*,*,#4973,.T.);
#7055=ORIENTED_EDGE('',*,*,#4974,.T.);
#7056=ORIENTED_EDGE('',*,*,#4975,.F.);
#7057=ORIENTED_EDGE('',*,*,#4976,.T.);
#7058=ORIENTED_EDGE('',*,*,#4977,.T.);
#7059=ORIENTED_EDGE('',*,*,#4978,.T.);
#7060=ORIENTED_EDGE('',*,*,#4979,.T.);
#7061=ORIENTED_EDGE('',*,*,#4980,.F.);
#7062=ORIENTED_EDGE('',*,*,#4981,.F.);
#7063=ORIENTED_EDGE('',*,*,#4982,.T.);
#7064=ORIENTED_EDGE('',*,*,#4983,.T.);
#7065=ORIENTED_EDGE('',*,*,#4984,.T.);
#7066=ORIENTED_EDGE('',*,*,#4985,.F.);
#7067=ORIENTED_EDGE('',*,*,#4973,.F.);
#7068=ORIENTED_EDGE('',*,*,#4986,.T.);
#7069=ORIENTED_EDGE('',*,*,#4987,.T.);
#7070=ORIENTED_EDGE('',*,*,#4988,.F.);
#7071=ORIENTED_EDGE('',*,*,#4989,.T.);
#7072=ORIENTED_EDGE('',*,*,#4990,.T.);
#7073=ORIENTED_EDGE('',*,*,#4991,.T.);
#7074=ORIENTED_EDGE('',*,*,#4992,.F.);
#7075=ORIENTED_EDGE('',*,*,#4984,.F.);
#7076=ORIENTED_EDGE('',*,*,#4993,.F.);
#7077=ORIENTED_EDGE('',*,*,#4994,.T.);
#7078=ORIENTED_EDGE('',*,*,#4995,.F.);
#7079=ORIENTED_EDGE('',*,*,#4996,.T.);
#7080=ORIENTED_EDGE('',*,*,#4997,.F.);
#7081=ORIENTED_EDGE('',*,*,#4987,.F.);
#7082=ORIENTED_EDGE('',*,*,#4998,.F.);
#7083=ORIENTED_EDGE('',*,*,#4999,.T.);
#7084=ORIENTED_EDGE('',*,*,#5000,.F.);
#7085=ORIENTED_EDGE('',*,*,#5001,.F.);
#7086=ORIENTED_EDGE('',*,*,#5000,.T.);
#7087=ORIENTED_EDGE('',*,*,#5002,.T.);
#7088=ORIENTED_EDGE('',*,*,#5003,.F.);
#7089=ORIENTED_EDGE('',*,*,#5001,.T.);
#7090=ORIENTED_EDGE('',*,*,#5004,.T.);
#7091=ORIENTED_EDGE('',*,*,#5005,.F.);
#7092=ORIENTED_EDGE('',*,*,#5006,.F.);
#7093=ORIENTED_EDGE('',*,*,#4988,.T.);
#7094=ORIENTED_EDGE('',*,*,#5007,.T.);
#7095=ORIENTED_EDGE('',*,*,#5006,.T.);
#7096=ORIENTED_EDGE('',*,*,#5008,.F.);
#7097=ORIENTED_EDGE('',*,*,#5009,.F.);
#7098=ORIENTED_EDGE('',*,*,#5010,.F.);
#7099=ORIENTED_EDGE('',*,*,#4989,.F.);
#7100=ORIENTED_EDGE('',*,*,#5007,.F.);
#7101=ORIENTED_EDGE('',*,*,#5011,.T.);
#7102=ORIENTED_EDGE('',*,*,#5012,.T.);
#7103=ORIENTED_EDGE('',*,*,#5013,.F.);
#7104=ORIENTED_EDGE('',*,*,#4998,.T.);
#7105=ORIENTED_EDGE('',*,*,#5010,.T.);
#7106=ORIENTED_EDGE('',*,*,#5014,.F.);
#7107=ORIENTED_EDGE('',*,*,#5013,.T.);
#7108=ORIENTED_EDGE('',*,*,#5015,.T.);
#7109=ORIENTED_EDGE('',*,*,#5016,.F.);
#7110=ORIENTED_EDGE('',*,*,#5017,.F.);
#7111=ORIENTED_EDGE('',*,*,#5018,.F.);
#7112=ORIENTED_EDGE('',*,*,#5002,.F.);
#7113=ORIENTED_EDGE('',*,*,#4999,.F.);
#7114=ORIENTED_EDGE('',*,*,#5017,.T.);
#7115=ORIENTED_EDGE('',*,*,#5019,.T.);
#7116=ORIENTED_EDGE('',*,*,#5020,.T.);
#7117=ORIENTED_EDGE('',*,*,#5021,.F.);
#7118=ORIENTED_EDGE('',*,*,#5022,.F.);
#7119=ORIENTED_EDGE('',*,*,#5023,.F.);
#7120=ORIENTED_EDGE('',*,*,#5024,.F.);
#7121=ORIENTED_EDGE('',*,*,#5025,.F.);
#7122=ORIENTED_EDGE('',*,*,#5018,.T.);
#7123=ORIENTED_EDGE('',*,*,#5026,.F.);
#7124=ORIENTED_EDGE('',*,*,#5003,.T.);
#7125=ORIENTED_EDGE('',*,*,#5026,.T.);
#7126=ORIENTED_EDGE('',*,*,#5027,.T.);
#7127=ORIENTED_EDGE('',*,*,#5028,.F.);
#7128=ORIENTED_EDGE('',*,*,#5004,.F.);
#7129=ORIENTED_EDGE('',*,*,#5029,.T.);
#7130=ORIENTED_EDGE('',*,*,#5030,.T.);
#7131=ORIENTED_EDGE('',*,*,#5031,.T.);
#7132=ORIENTED_EDGE('',*,*,#5032,.T.);
#7133=ORIENTED_EDGE('',*,*,#5033,.F.);
#7134=ORIENTED_EDGE('',*,*,#5034,.T.);
#7135=ORIENTED_EDGE('',*,*,#5035,.T.);
#7136=ORIENTED_EDGE('',*,*,#5008,.T.);
#7137=ORIENTED_EDGE('',*,*,#5036,.F.);
#7138=ORIENTED_EDGE('',*,*,#5037,.T.);
#7139=ORIENTED_EDGE('',*,*,#5038,.T.);
#7140=ORIENTED_EDGE('',*,*,#5039,.T.);
#7141=ORIENTED_EDGE('',*,*,#5040,.F.);
#7142=ORIENTED_EDGE('',*,*,#5028,.T.);
#7143=ORIENTED_EDGE('',*,*,#5041,.T.);
#7144=ORIENTED_EDGE('',*,*,#5042,.T.);
#7145=ORIENTED_EDGE('',*,*,#5043,.T.);
#7146=ORIENTED_EDGE('',*,*,#5044,.T.);
#7147=ORIENTED_EDGE('',*,*,#5045,.T.);
#7148=ORIENTED_EDGE('',*,*,#5046,.F.);
#7149=ORIENTED_EDGE('',*,*,#5047,.F.);
#7150=ORIENTED_EDGE('',*,*,#5048,.T.);
#7151=ORIENTED_EDGE('',*,*,#5049,.T.);
#7152=ORIENTED_EDGE('',*,*,#5050,.T.);
#7153=ORIENTED_EDGE('',*,*,#5029,.F.);
#7154=ORIENTED_EDGE('',*,*,#5051,.F.);
#7155=ORIENTED_EDGE('',*,*,#5050,.F.);
#7156=ORIENTED_EDGE('',*,*,#5052,.T.);
#7157=ORIENTED_EDGE('',*,*,#5053,.T.);
#7158=ORIENTED_EDGE('',*,*,#5054,.F.);
#7159=ORIENTED_EDGE('',*,*,#5030,.F.);
#7160=ORIENTED_EDGE('',*,*,#5054,.T.);
#7161=ORIENTED_EDGE('',*,*,#5055,.T.);
#7162=ORIENTED_EDGE('',*,*,#5056,.F.);
#7163=ORIENTED_EDGE('',*,*,#5057,.F.);
#7164=ORIENTED_EDGE('',*,*,#5056,.T.);
#7165=ORIENTED_EDGE('',*,*,#5058,.T.);
#7166=ORIENTED_EDGE('',*,*,#5059,.F.);
#7167=ORIENTED_EDGE('',*,*,#5031,.F.);
#7168=ORIENTED_EDGE('',*,*,#5057,.T.);
#7169=ORIENTED_EDGE('',*,*,#5060,.T.);
#7170=ORIENTED_EDGE('',*,*,#5061,.T.);
#7171=ORIENTED_EDGE('',*,*,#5062,.T.);
#7172=ORIENTED_EDGE('',*,*,#5032,.F.);
#7173=ORIENTED_EDGE('',*,*,#5060,.F.);
#7174=ORIENTED_EDGE('',*,*,#5063,.F.);
#7175=ORIENTED_EDGE('',*,*,#4994,.F.);
#7176=ORIENTED_EDGE('',*,*,#5061,.F.);
#7177=ORIENTED_EDGE('',*,*,#5059,.T.);
#7178=ORIENTED_EDGE('',*,*,#5064,.T.);
#7179=ORIENTED_EDGE('',*,*,#5065,.F.);
#7180=ORIENTED_EDGE('',*,*,#4985,.T.);
#7181=ORIENTED_EDGE('',*,*,#5063,.T.);
#7182=ORIENTED_EDGE('',*,*,#5066,.F.);
#7183=ORIENTED_EDGE('',*,*,#5065,.T.);
#7184=ORIENTED_EDGE('',*,*,#5067,.T.);
#7185=ORIENTED_EDGE('',*,*,#5068,.F.);
#7186=ORIENTED_EDGE('',*,*,#4974,.F.);
#7187=ORIENTED_EDGE('',*,*,#5069,.F.);
#7188=ORIENTED_EDGE('',*,*,#5068,.T.);
#7189=ORIENTED_EDGE('',*,*,#5070,.T.);
#7190=ORIENTED_EDGE('',*,*,#5071,.F.);
#7191=ORIENTED_EDGE('',*,*,#5072,.T.);
#7192=ORIENTED_EDGE('',*,*,#4975,.T.);
#7193=ORIENTED_EDGE('',*,*,#5069,.T.);
#7194=ORIENTED_EDGE('',*,*,#5073,.F.);
#7195=ORIENTED_EDGE('',*,*,#5072,.F.);
#7196=ORIENTED_EDGE('',*,*,#5074,.T.);
#7197=ORIENTED_EDGE('',*,*,#5075,.T.);
#7198=ORIENTED_EDGE('',*,*,#5076,.F.);
#7199=ORIENTED_EDGE('',*,*,#5077,.F.);
#7200=ORIENTED_EDGE('',*,*,#4976,.F.);
#7201=ORIENTED_EDGE('',*,*,#5076,.T.);
#7202=ORIENTED_EDGE('',*,*,#5078,.T.);
#7203=ORIENTED_EDGE('',*,*,#5079,.F.);
#7204=ORIENTED_EDGE('',*,*,#5080,.T.);
#7205=ORIENTED_EDGE('',*,*,#5077,.T.);
#7206=ORIENTED_EDGE('',*,*,#5081,.F.);
#7207=ORIENTED_EDGE('',*,*,#5079,.T.);
#7208=ORIENTED_EDGE('',*,*,#5082,.T.);
#7209=ORIENTED_EDGE('',*,*,#5083,.F.);
#7210=ORIENTED_EDGE('',*,*,#5084,.F.);
#7211=ORIENTED_EDGE('',*,*,#4996,.F.);
#7212=ORIENTED_EDGE('',*,*,#5084,.T.);
#7213=ORIENTED_EDGE('',*,*,#5085,.T.);
#7214=ORIENTED_EDGE('',*,*,#5037,.F.);
#7215=ORIENTED_EDGE('',*,*,#5086,.F.);
#7216=ORIENTED_EDGE('',*,*,#5087,.F.);
#7217=ORIENTED_EDGE('',*,*,#4997,.T.);
#7218=ORIENTED_EDGE('',*,*,#5086,.T.);
#7219=ORIENTED_EDGE('',*,*,#5088,.F.);
#7220=ORIENTED_EDGE('',*,*,#5089,.F.);
#7221=ORIENTED_EDGE('',*,*,#4978,.F.);
#7222=ORIENTED_EDGE('',*,*,#5090,.T.);
#7223=ORIENTED_EDGE('',*,*,#5087,.T.);
#7224=ORIENTED_EDGE('',*,*,#5091,.F.);
#7225=ORIENTED_EDGE('',*,*,#5091,.T.);
#7226=ORIENTED_EDGE('',*,*,#5092,.T.);
#7227=ORIENTED_EDGE('',*,*,#4979,.F.);
#7228=ORIENTED_EDGE('',*,*,#5092,.F.);
#7229=ORIENTED_EDGE('',*,*,#5089,.T.);
#7230=ORIENTED_EDGE('',*,*,#5045,.F.);
#7231=ORIENTED_EDGE('',*,*,#5093,.F.);
#7232=ORIENTED_EDGE('',*,*,#4980,.T.);
#7233=ORIENTED_EDGE('',*,*,#5093,.T.);
#7234=ORIENTED_EDGE('',*,*,#5044,.F.);
#7235=ORIENTED_EDGE('',*,*,#5094,.F.);
#7236=ORIENTED_EDGE('',*,*,#4981,.T.);
#7237=ORIENTED_EDGE('',*,*,#5094,.T.);
#7238=ORIENTED_EDGE('',*,*,#5049,.F.);
#7239=ORIENTED_EDGE('',*,*,#5095,.F.);
#7240=ORIENTED_EDGE('',*,*,#5096,.F.);
#7241=ORIENTED_EDGE('',*,*,#5095,.T.);
#7242=ORIENTED_EDGE('',*,*,#5048,.F.);
#7243=ORIENTED_EDGE('',*,*,#5097,.F.);
#7244=ORIENTED_EDGE('',*,*,#4982,.F.);
#7245=ORIENTED_EDGE('',*,*,#5096,.T.);
#7246=ORIENTED_EDGE('',*,*,#5098,.F.);
#7247=ORIENTED_EDGE('',*,*,#4983,.F.);
#7248=ORIENTED_EDGE('',*,*,#5098,.T.);
#7249=ORIENTED_EDGE('',*,*,#5099,.T.);
#7250=ORIENTED_EDGE('',*,*,#4986,.F.);
#7251=ORIENTED_EDGE('',*,*,#5099,.F.);
#7252=ORIENTED_EDGE('',*,*,#5097,.T.);
#7253=ORIENTED_EDGE('',*,*,#5100,.F.);
#7254=ORIENTED_EDGE('',*,*,#5062,.F.);
#7255=ORIENTED_EDGE('',*,*,#4993,.T.);
#7256=ORIENTED_EDGE('',*,*,#5101,.F.);
#7257=ORIENTED_EDGE('',*,*,#5102,.T.);
#7258=ORIENTED_EDGE('',*,*,#5046,.T.);
#7259=ORIENTED_EDGE('',*,*,#5088,.T.);
#7260=ORIENTED_EDGE('',*,*,#5036,.T.);
#7261=ORIENTED_EDGE('',*,*,#5005,.T.);
#7262=ORIENTED_EDGE('',*,*,#5040,.T.);
#7263=ORIENTED_EDGE('',*,*,#5103,.T.);
#7264=ORIENTED_EDGE('',*,*,#5033,.T.);
#7265=ORIENTED_EDGE('',*,*,#5100,.T.);
#7266=ORIENTED_EDGE('',*,*,#5047,.T.);
#7267=ORIENTED_EDGE('',*,*,#5102,.F.);
#7268=ORIENTED_EDGE('',*,*,#5104,.T.);
#7269=ORIENTED_EDGE('',*,*,#4992,.T.);
#7270=ORIENTED_EDGE('',*,*,#5105,.T.);
#7271=ORIENTED_EDGE('',*,*,#5103,.F.);
#7272=ORIENTED_EDGE('',*,*,#5106,.F.);
#7273=ORIENTED_EDGE('',*,*,#5104,.F.);
#7274=ORIENTED_EDGE('',*,*,#5107,.T.);
#7275=ORIENTED_EDGE('',*,*,#5022,.T.);
#7276=ORIENTED_EDGE('',*,*,#5108,.F.);
#7277=ORIENTED_EDGE('',*,*,#5021,.T.);
#7278=ORIENTED_EDGE('',*,*,#5109,.F.);
#7279=ORIENTED_EDGE('',*,*,#4990,.F.);
#7280=ORIENTED_EDGE('',*,*,#5108,.T.);
#7281=ORIENTED_EDGE('',*,*,#5110,.F.);
#7282=ORIENTED_EDGE('',*,*,#5109,.T.);
#7283=ORIENTED_EDGE('',*,*,#5111,.T.);
#7284=ORIENTED_EDGE('',*,*,#5112,.F.);
#7285=ORIENTED_EDGE('',*,*,#5110,.T.);
#7286=ORIENTED_EDGE('',*,*,#5113,.T.);
#7287=ORIENTED_EDGE('',*,*,#5052,.F.);
#7288=ORIENTED_EDGE('',*,*,#5114,.F.);
#7289=ORIENTED_EDGE('',*,*,#4991,.F.);
#7290=ORIENTED_EDGE('',*,*,#5114,.T.);
#7291=ORIENTED_EDGE('',*,*,#5051,.T.);
#7292=ORIENTED_EDGE('',*,*,#5034,.F.);
#7293=ORIENTED_EDGE('',*,*,#5105,.F.);
#7294=ORIENTED_EDGE('',*,*,#5112,.T.);
#7295=ORIENTED_EDGE('',*,*,#5115,.F.);
#7296=ORIENTED_EDGE('',*,*,#5116,.F.);
#7297=ORIENTED_EDGE('',*,*,#5117,.F.);
#7298=ORIENTED_EDGE('',*,*,#5118,.F.);
#7299=ORIENTED_EDGE('',*,*,#5119,.F.);
#7300=ORIENTED_EDGE('',*,*,#5120,.F.);
#7301=ORIENTED_EDGE('',*,*,#5121,.F.);
#7302=ORIENTED_EDGE('',*,*,#5070,.F.);
#7303=ORIENTED_EDGE('',*,*,#5067,.F.);
#7304=ORIENTED_EDGE('',*,*,#5066,.T.);
#7305=ORIENTED_EDGE('',*,*,#5064,.F.);
#7306=ORIENTED_EDGE('',*,*,#5058,.F.);
#7307=ORIENTED_EDGE('',*,*,#5055,.F.);
#7308=ORIENTED_EDGE('',*,*,#5053,.F.);
#7309=ORIENTED_EDGE('',*,*,#5113,.F.);
#7310=ORIENTED_EDGE('',*,*,#5122,.F.);
#7311=ORIENTED_EDGE('',*,*,#5071,.T.);
#7312=ORIENTED_EDGE('',*,*,#5121,.T.);
#7313=ORIENTED_EDGE('',*,*,#5123,.F.);
#7314=ORIENTED_EDGE('',*,*,#5124,.T.);
#7315=ORIENTED_EDGE('',*,*,#5073,.T.);
#7316=ORIENTED_EDGE('',*,*,#5122,.T.);
#7317=ORIENTED_EDGE('',*,*,#5125,.F.);
#7318=ORIENTED_EDGE('',*,*,#5124,.F.);
#7319=ORIENTED_EDGE('',*,*,#5126,.T.);
#7320=ORIENTED_EDGE('',*,*,#5127,.T.);
#7321=ORIENTED_EDGE('',*,*,#5074,.F.);
#7322=ORIENTED_EDGE('',*,*,#5014,.T.);
#7323=ORIENTED_EDGE('',*,*,#5012,.F.);
#7324=ORIENTED_EDGE('',*,*,#5128,.F.);
#7325=ORIENTED_EDGE('',*,*,#5129,.F.);
#7326=ORIENTED_EDGE('',*,*,#5130,.F.);
#7327=ORIENTED_EDGE('',*,*,#5082,.F.);
#7328=ORIENTED_EDGE('',*,*,#5081,.T.);
#7329=ORIENTED_EDGE('',*,*,#5078,.F.);
#7330=ORIENTED_EDGE('',*,*,#5075,.F.);
#7331=ORIENTED_EDGE('',*,*,#5127,.F.);
#7332=ORIENTED_EDGE('',*,*,#5131,.F.);
#7333=ORIENTED_EDGE('',*,*,#5132,.F.);
#7334=ORIENTED_EDGE('',*,*,#5133,.F.);
#7335=ORIENTED_EDGE('',*,*,#5134,.F.);
#7336=ORIENTED_EDGE('',*,*,#5135,.F.);
#7337=ORIENTED_EDGE('',*,*,#5015,.F.);
#7338=ORIENTED_EDGE('',*,*,#5136,.F.);
#7339=ORIENTED_EDGE('',*,*,#5016,.T.);
#7340=ORIENTED_EDGE('',*,*,#5135,.T.);
#7341=ORIENTED_EDGE('',*,*,#5137,.F.);
#7342=ORIENTED_EDGE('',*,*,#5136,.T.);
#7343=ORIENTED_EDGE('',*,*,#5138,.T.);
#7344=ORIENTED_EDGE('',*,*,#5139,.T.);
#7345=ORIENTED_EDGE('',*,*,#5019,.F.);
#7346=ORIENTED_EDGE('',*,*,#5139,.F.);
#7347=ORIENTED_EDGE('',*,*,#5140,.T.);
#7348=ORIENTED_EDGE('',*,*,#5116,.T.);
#7349=ORIENTED_EDGE('',*,*,#5141,.F.);
#7350=ORIENTED_EDGE('',*,*,#5111,.F.);
#7351=ORIENTED_EDGE('',*,*,#5020,.F.);
#7352=ORIENTED_EDGE('',*,*,#5141,.T.);
#7353=ORIENTED_EDGE('',*,*,#5115,.T.);
#7354=ORIENTED_EDGE('',*,*,#5142,.F.);
#7355=ORIENTED_EDGE('',*,*,#5143,.T.);
#7356=ORIENTED_EDGE('',*,*,#5117,.T.);
#7357=ORIENTED_EDGE('',*,*,#5140,.F.);
#7358=ORIENTED_EDGE('',*,*,#5144,.T.);
#7359=ORIENTED_EDGE('',*,*,#5145,.T.);
#7360=ORIENTED_EDGE('',*,*,#5142,.T.);
#7361=ORIENTED_EDGE('',*,*,#5138,.F.);
#7362=ORIENTED_EDGE('',*,*,#5144,.F.);
#7363=ORIENTED_EDGE('',*,*,#5137,.T.);
#7364=ORIENTED_EDGE('',*,*,#5134,.T.);
#7365=ORIENTED_EDGE('',*,*,#5146,.F.);
#7366=ORIENTED_EDGE('',*,*,#5147,.F.);
#7367=ORIENTED_EDGE('',*,*,#5146,.T.);
#7368=ORIENTED_EDGE('',*,*,#5133,.T.);
#7369=ORIENTED_EDGE('',*,*,#5148,.F.);
#7370=ORIENTED_EDGE('',*,*,#5147,.T.);
#7371=ORIENTED_EDGE('',*,*,#5149,.T.);
#7372=ORIENTED_EDGE('',*,*,#5150,.T.);
#7373=ORIENTED_EDGE('',*,*,#5145,.F.);
#7374=ORIENTED_EDGE('',*,*,#5150,.F.);
#7375=ORIENTED_EDGE('',*,*,#5151,.T.);
#7376=ORIENTED_EDGE('',*,*,#5118,.T.);
#7377=ORIENTED_EDGE('',*,*,#5143,.F.);
#7378=ORIENTED_EDGE('',*,*,#5152,.F.);
#7379=ORIENTED_EDGE('',*,*,#5153,.T.);
#7380=ORIENTED_EDGE('',*,*,#5119,.T.);
#7381=ORIENTED_EDGE('',*,*,#5151,.F.);
#7382=ORIENTED_EDGE('',*,*,#5154,.T.);
#7383=ORIENTED_EDGE('',*,*,#5155,.T.);
#7384=ORIENTED_EDGE('',*,*,#5152,.T.);
#7385=ORIENTED_EDGE('',*,*,#5149,.F.);
#7386=ORIENTED_EDGE('',*,*,#5156,.T.);
#7387=ORIENTED_EDGE('',*,*,#5157,.T.);
#7388=ORIENTED_EDGE('',*,*,#5158,.T.);
#7389=ORIENTED_EDGE('',*,*,#5159,.T.);
#7390=ORIENTED_EDGE('',*,*,#5160,.T.);
#7391=ORIENTED_EDGE('',*,*,#5161,.T.);
#7392=ORIENTED_EDGE('',*,*,#5156,.F.);
#7393=ORIENTED_EDGE('',*,*,#5158,.F.);
#7394=ORIENTED_EDGE('',*,*,#5162,.F.);
#7395=ORIENTED_EDGE('',*,*,#5163,.T.);
#7396=ORIENTED_EDGE('',*,*,#5164,.T.);
#7397=ORIENTED_EDGE('',*,*,#5160,.F.);
#7398=ORIENTED_EDGE('',*,*,#5159,.F.);
#7399=ORIENTED_EDGE('',*,*,#5162,.T.);
#7400=ORIENTED_EDGE('',*,*,#5157,.F.);
#7401=ORIENTED_EDGE('',*,*,#5161,.F.);
#7402=ORIENTED_EDGE('',*,*,#5164,.F.);
#7403=ORIENTED_EDGE('',*,*,#5165,.T.);
#7404=ORIENTED_EDGE('',*,*,#5163,.F.);
#7405=ORIENTED_EDGE('',*,*,#5166,.T.);
#7406=ORIENTED_EDGE('',*,*,#5167,.T.);
#7407=ORIENTED_EDGE('',*,*,#5166,.F.);
#7408=ORIENTED_EDGE('',*,*,#5165,.F.);
#7409=ORIENTED_EDGE('',*,*,#5168,.T.);
#7410=ORIENTED_EDGE('',*,*,#5167,.F.);
#7411=ORIENTED_EDGE('',*,*,#5168,.F.);
#7412=ORIENTED_EDGE('',*,*,#5169,.T.);
#7413=ORIENTED_EDGE('',*,*,#5170,.T.);
#7414=ORIENTED_EDGE('',*,*,#5169,.F.);
#7415=ORIENTED_EDGE('',*,*,#5101,.T.);
#7416=ORIENTED_EDGE('',*,*,#5170,.F.);
#7417=ORIENTED_EDGE('',*,*,#5154,.F.);
#7418=ORIENTED_EDGE('',*,*,#5148,.T.);
#7419=ORIENTED_EDGE('',*,*,#5132,.T.);
#7420=ORIENTED_EDGE('',*,*,#5171,.F.);
#7421=ORIENTED_EDGE('',*,*,#5172,.F.);
#7422=ORIENTED_EDGE('',*,*,#5171,.T.);
#7423=ORIENTED_EDGE('',*,*,#5131,.T.);
#7424=ORIENTED_EDGE('',*,*,#5126,.F.);
#7425=ORIENTED_EDGE('',*,*,#5172,.T.);
#7426=ORIENTED_EDGE('',*,*,#5125,.T.);
#7427=ORIENTED_EDGE('',*,*,#5173,.T.);
#7428=ORIENTED_EDGE('',*,*,#5155,.F.);
#7429=ORIENTED_EDGE('',*,*,#5173,.F.);
#7430=ORIENTED_EDGE('',*,*,#5123,.T.);
#7431=ORIENTED_EDGE('',*,*,#5120,.T.);
#7432=ORIENTED_EDGE('',*,*,#5153,.F.);
#7433=ORIENTED_EDGE('',*,*,#5174,.F.);
#7434=ORIENTED_EDGE('',*,*,#5083,.T.);
#7435=ORIENTED_EDGE('',*,*,#5130,.T.);
#7436=ORIENTED_EDGE('',*,*,#5175,.F.);
#7437=ORIENTED_EDGE('',*,*,#5174,.T.);
#7438=ORIENTED_EDGE('',*,*,#5038,.F.);
#7439=ORIENTED_EDGE('',*,*,#5085,.F.);
#7440=ORIENTED_EDGE('',*,*,#5039,.F.);
#7441=ORIENTED_EDGE('',*,*,#5175,.T.);
#7442=ORIENTED_EDGE('',*,*,#5129,.T.);
#7443=ORIENTED_EDGE('',*,*,#5176,.F.);
#7444=ORIENTED_EDGE('',*,*,#5177,.F.);
#7445=ORIENTED_EDGE('',*,*,#5176,.T.);
#7446=ORIENTED_EDGE('',*,*,#5128,.T.);
#7447=ORIENTED_EDGE('',*,*,#5011,.F.);
#7448=ORIENTED_EDGE('',*,*,#5035,.F.);
#7449=ORIENTED_EDGE('',*,*,#5177,.T.);
#7450=ORIENTED_EDGE('',*,*,#5009,.T.);
#7451=ORIENTED_EDGE('',*,*,#5107,.F.);
#7452=ORIENTED_EDGE('',*,*,#5178,.F.);
#7453=ORIENTED_EDGE('',*,*,#5023,.T.);
#7454=ORIENTED_EDGE('',*,*,#5178,.T.);
#7455=ORIENTED_EDGE('',*,*,#5106,.T.);
#7456=ORIENTED_EDGE('',*,*,#5043,.F.);
#7457=ORIENTED_EDGE('',*,*,#5179,.F.);
#7458=ORIENTED_EDGE('',*,*,#5024,.T.);
#7459=ORIENTED_EDGE('',*,*,#5179,.T.);
#7460=ORIENTED_EDGE('',*,*,#5042,.F.);
#7461=ORIENTED_EDGE('',*,*,#5180,.F.);
#7462=ORIENTED_EDGE('',*,*,#5025,.T.);
#7463=ORIENTED_EDGE('',*,*,#5180,.T.);
#7464=ORIENTED_EDGE('',*,*,#5041,.F.);
#7465=ORIENTED_EDGE('',*,*,#5027,.F.);
#7466=ORIENTED_EDGE('',*,*,#4977,.F.);
#7467=ORIENTED_EDGE('',*,*,#5080,.F.);
#7468=ORIENTED_EDGE('',*,*,#4995,.T.);
#7469=ORIENTED_EDGE('',*,*,#5090,.F.);
#7470=ORIENTED_EDGE('',*,*,#5181,.T.);
#7471=ORIENTED_EDGE('',*,*,#5182,.T.);
#7472=ORIENTED_EDGE('',*,*,#5183,.T.);
#7473=ORIENTED_EDGE('',*,*,#5184,.T.);
#7474=ORIENTED_EDGE('',*,*,#5185,.T.);
#7475=ORIENTED_EDGE('',*,*,#5186,.T.);
#7476=ORIENTED_EDGE('',*,*,#5187,.T.);
#7477=ORIENTED_EDGE('',*,*,#5188,.T.);
#7478=ORIENTED_EDGE('',*,*,#5189,.T.);
#7479=ORIENTED_EDGE('',*,*,#5190,.T.);
#7480=ORIENTED_EDGE('',*,*,#5191,.T.);
#7481=ORIENTED_EDGE('',*,*,#5192,.T.);
#7482=ORIENTED_EDGE('',*,*,#5193,.T.);
#7483=ORIENTED_EDGE('',*,*,#5194,.T.);
#7484=ORIENTED_EDGE('',*,*,#5195,.T.);
#7485=ORIENTED_EDGE('',*,*,#5196,.T.);
#7486=ORIENTED_EDGE('',*,*,#5197,.T.);
#7487=ORIENTED_EDGE('',*,*,#5198,.T.);
#7488=ORIENTED_EDGE('',*,*,#5199,.T.);
#7489=ORIENTED_EDGE('',*,*,#5200,.T.);
#7490=ORIENTED_EDGE('',*,*,#5201,.T.);
#7491=ORIENTED_EDGE('',*,*,#5202,.T.);
#7492=ORIENTED_EDGE('',*,*,#5203,.T.);
#7493=ORIENTED_EDGE('',*,*,#5204,.T.);
#7494=ORIENTED_EDGE('',*,*,#5205,.T.);
#7495=ORIENTED_EDGE('',*,*,#5181,.F.);
#7496=ORIENTED_EDGE('',*,*,#5206,.T.);
#7497=ORIENTED_EDGE('',*,*,#5207,.T.);
#7498=ORIENTED_EDGE('',*,*,#5206,.F.);
#7499=ORIENTED_EDGE('',*,*,#5207,.F.);
#7500=ORIENTED_EDGE('',*,*,#5208,.T.);
#7501=ORIENTED_EDGE('',*,*,#5209,.T.);
#7502=ORIENTED_EDGE('',*,*,#5208,.F.);
#7503=ORIENTED_EDGE('',*,*,#5209,.F.);
#7504=ORIENTED_EDGE('',*,*,#5210,.T.);
#7505=ORIENTED_EDGE('',*,*,#5211,.T.);
#7506=ORIENTED_EDGE('',*,*,#5212,.T.);
#7507=ORIENTED_EDGE('',*,*,#5210,.F.);
#7508=ORIENTED_EDGE('',*,*,#5213,.F.);
#7509=ORIENTED_EDGE('',*,*,#5214,.T.);
#7510=ORIENTED_EDGE('',*,*,#5215,.T.);
#7511=ORIENTED_EDGE('',*,*,#5211,.F.);
#7512=ORIENTED_EDGE('',*,*,#5212,.F.);
#7513=ORIENTED_EDGE('',*,*,#5215,.F.);
#7514=ORIENTED_EDGE('',*,*,#5216,.T.);
#7515=ORIENTED_EDGE('',*,*,#5217,.T.);
#7516=ORIENTED_EDGE('',*,*,#5216,.F.);
#7517=ORIENTED_EDGE('',*,*,#5214,.F.);
#7518=ORIENTED_EDGE('',*,*,#5218,.F.);
#7519=ORIENTED_EDGE('',*,*,#5219,.F.);
#7520=ORIENTED_EDGE('',*,*,#5220,.F.);
#7521=ORIENTED_EDGE('',*,*,#5221,.T.);
#7522=ORIENTED_EDGE('',*,*,#5222,.T.);
#7523=ORIENTED_EDGE('',*,*,#5213,.T.);
#7524=ORIENTED_EDGE('',*,*,#5217,.F.);
#7525=ORIENTED_EDGE('',*,*,#5223,.T.);
#7526=ORIENTED_EDGE('',*,*,#5219,.T.);
#7527=ORIENTED_EDGE('',*,*,#5224,.T.);
#7528=ORIENTED_EDGE('',*,*,#5225,.F.);
#7529=ORIENTED_EDGE('',*,*,#5226,.F.);
#7530=ORIENTED_EDGE('',*,*,#5227,.F.);
#7531=ORIENTED_EDGE('',*,*,#5228,.F.);
#7532=ORIENTED_EDGE('',*,*,#5229,.T.);
#7533=ORIENTED_EDGE('',*,*,#5220,.T.);
#7534=ORIENTED_EDGE('',*,*,#5223,.F.);
#7535=ORIENTED_EDGE('',*,*,#5230,.T.);
#7536=ORIENTED_EDGE('',*,*,#5227,.T.);
#7537=ORIENTED_EDGE('',*,*,#5226,.T.);
#7538=ORIENTED_EDGE('',*,*,#5231,.F.);
#7539=ORIENTED_EDGE('',*,*,#5232,.F.);
#7540=ORIENTED_EDGE('',*,*,#5233,.F.);
#7541=ORIENTED_EDGE('',*,*,#5234,.F.);
#7542=ORIENTED_EDGE('',*,*,#5235,.T.);
#7543=ORIENTED_EDGE('',*,*,#5228,.T.);
#7544=ORIENTED_EDGE('',*,*,#5230,.F.);
#7545=ORIENTED_EDGE('',*,*,#5236,.T.);
#7546=ORIENTED_EDGE('',*,*,#5233,.T.);
#7547=ORIENTED_EDGE('',*,*,#5232,.T.);
#7548=ORIENTED_EDGE('',*,*,#5237,.F.);
#7549=ORIENTED_EDGE('',*,*,#5238,.F.);
#7550=ORIENTED_EDGE('',*,*,#5239,.F.);
#7551=ORIENTED_EDGE('',*,*,#5240,.F.);
#7552=ORIENTED_EDGE('',*,*,#5241,.T.);
#7553=ORIENTED_EDGE('',*,*,#5234,.T.);
#7554=ORIENTED_EDGE('',*,*,#5236,.F.);
#7555=ORIENTED_EDGE('',*,*,#5242,.T.);
#7556=ORIENTED_EDGE('',*,*,#5239,.T.);
#7557=ORIENTED_EDGE('',*,*,#5238,.T.);
#7558=ORIENTED_EDGE('',*,*,#5243,.F.);
#7559=ORIENTED_EDGE('',*,*,#5244,.F.);
#7560=ORIENTED_EDGE('',*,*,#5245,.F.);
#7561=ORIENTED_EDGE('',*,*,#5246,.F.);
#7562=ORIENTED_EDGE('',*,*,#5247,.T.);
#7563=ORIENTED_EDGE('',*,*,#5240,.T.);
#7564=ORIENTED_EDGE('',*,*,#5242,.F.);
#7565=ORIENTED_EDGE('',*,*,#5248,.T.);
#7566=ORIENTED_EDGE('',*,*,#5245,.T.);
#7567=ORIENTED_EDGE('',*,*,#5244,.T.);
#7568=ORIENTED_EDGE('',*,*,#5249,.F.);
#7569=ORIENTED_EDGE('',*,*,#5250,.F.);
#7570=ORIENTED_EDGE('',*,*,#5251,.F.);
#7571=ORIENTED_EDGE('',*,*,#5252,.F.);
#7572=ORIENTED_EDGE('',*,*,#5253,.F.);
#7573=ORIENTED_EDGE('',*,*,#5254,.T.);
#7574=ORIENTED_EDGE('',*,*,#5246,.T.);
#7575=ORIENTED_EDGE('',*,*,#5248,.F.);
#7576=ORIENTED_EDGE('',*,*,#5251,.T.);
#7577=ORIENTED_EDGE('',*,*,#5250,.T.);
#7578=ORIENTED_EDGE('',*,*,#5255,.F.);
#7579=ORIENTED_EDGE('',*,*,#5256,.F.);
#7580=ORIENTED_EDGE('',*,*,#5252,.T.);
#7581=ORIENTED_EDGE('',*,*,#5256,.T.);
#7582=ORIENTED_EDGE('',*,*,#5257,.T.);
#7583=ORIENTED_EDGE('',*,*,#5253,.T.);
#7584=ORIENTED_EDGE('',*,*,#5257,.F.);
#7585=ORIENTED_EDGE('',*,*,#5255,.T.);
#7586=ORIENTED_EDGE('',*,*,#5258,.T.);
#7587=ORIENTED_EDGE('',*,*,#5254,.F.);
#7588=ORIENTED_EDGE('',*,*,#5258,.F.);
#7589=ORIENTED_EDGE('',*,*,#5249,.T.);
#7590=ORIENTED_EDGE('',*,*,#5259,.T.);
#7591=ORIENTED_EDGE('',*,*,#5247,.F.);
#7592=ORIENTED_EDGE('',*,*,#5259,.F.);
#7593=ORIENTED_EDGE('',*,*,#5243,.T.);
#7594=ORIENTED_EDGE('',*,*,#5260,.T.);
#7595=ORIENTED_EDGE('',*,*,#5241,.F.);
#7596=ORIENTED_EDGE('',*,*,#5260,.F.);
#7597=ORIENTED_EDGE('',*,*,#5237,.T.);
#7598=ORIENTED_EDGE('',*,*,#5261,.T.);
#7599=ORIENTED_EDGE('',*,*,#5235,.F.);
#7600=ORIENTED_EDGE('',*,*,#5261,.F.);
#7601=ORIENTED_EDGE('',*,*,#5231,.T.);
#7602=ORIENTED_EDGE('',*,*,#5262,.T.);
#7603=ORIENTED_EDGE('',*,*,#5229,.F.);
#7604=ORIENTED_EDGE('',*,*,#5262,.F.);
#7605=ORIENTED_EDGE('',*,*,#5225,.T.);
#7606=ORIENTED_EDGE('',*,*,#5263,.T.);
#7607=ORIENTED_EDGE('',*,*,#5221,.F.);
#7608=ORIENTED_EDGE('',*,*,#5218,.T.);
#7609=ORIENTED_EDGE('',*,*,#5222,.F.);
#7610=ORIENTED_EDGE('',*,*,#5263,.F.);
#7611=ORIENTED_EDGE('',*,*,#5224,.F.);
#7612=ORIENTED_EDGE('',*,*,#5264,.T.);
#7613=ORIENTED_EDGE('',*,*,#5265,.F.);
#7614=ORIENTED_EDGE('',*,*,#5266,.F.);
#7615=ORIENTED_EDGE('',*,*,#5182,.F.);
#7616=ORIENTED_EDGE('',*,*,#5264,.F.);
#7617=ORIENTED_EDGE('',*,*,#5205,.F.);
#7618=ORIENTED_EDGE('',*,*,#5267,.F.);
#7619=ORIENTED_EDGE('',*,*,#5268,.T.);
#7620=ORIENTED_EDGE('',*,*,#5269,.T.);
#7621=ORIENTED_EDGE('',*,*,#5270,.T.);
#7622=ORIENTED_EDGE('',*,*,#5271,.T.);
#7623=ORIENTED_EDGE('',*,*,#5272,.T.);
#7624=ORIENTED_EDGE('',*,*,#5273,.F.);
#7625=ORIENTED_EDGE('',*,*,#5265,.T.);
#7626=ORIENTED_EDGE('',*,*,#5268,.F.);
#7627=ORIENTED_EDGE('',*,*,#5274,.T.);
#7628=ORIENTED_EDGE('',*,*,#5275,.F.);
#7629=ORIENTED_EDGE('',*,*,#5276,.T.);
#7630=ORIENTED_EDGE('',*,*,#5277,.T.);
#7631=ORIENTED_EDGE('',*,*,#5278,.T.);
#7632=ORIENTED_EDGE('',*,*,#5279,.F.);
#7633=ORIENTED_EDGE('',*,*,#5280,.T.);
#7634=ORIENTED_EDGE('',*,*,#5281,.T.);
#7635=ORIENTED_EDGE('',*,*,#5282,.T.);
#7636=ORIENTED_EDGE('',*,*,#5283,.T.);
#7637=ORIENTED_EDGE('',*,*,#5284,.T.);
#7638=ORIENTED_EDGE('',*,*,#5285,.T.);
#7639=ORIENTED_EDGE('',*,*,#5286,.T.);
#7640=ORIENTED_EDGE('',*,*,#5287,.F.);
#7641=ORIENTED_EDGE('',*,*,#5288,.T.);
#7642=ORIENTED_EDGE('',*,*,#5289,.T.);
#7643=ORIENTED_EDGE('',*,*,#5290,.T.);
#7644=ORIENTED_EDGE('',*,*,#5291,.F.);
#7645=ORIENTED_EDGE('',*,*,#5187,.F.);
#7646=ORIENTED_EDGE('',*,*,#5292,.F.);
#7647=ORIENTED_EDGE('',*,*,#5269,.F.);
#7648=ORIENTED_EDGE('',*,*,#5291,.T.);
#7649=ORIENTED_EDGE('',*,*,#5290,.F.);
#7650=ORIENTED_EDGE('',*,*,#5293,.F.);
#7651=ORIENTED_EDGE('',*,*,#5188,.F.);
#7652=ORIENTED_EDGE('',*,*,#5293,.T.);
#7653=ORIENTED_EDGE('',*,*,#5289,.F.);
#7654=ORIENTED_EDGE('',*,*,#5294,.T.);
#7655=ORIENTED_EDGE('',*,*,#5189,.F.);
#7656=ORIENTED_EDGE('',*,*,#5295,.T.);
#7657=ORIENTED_EDGE('',*,*,#5190,.F.);
#7658=ORIENTED_EDGE('',*,*,#5294,.F.);
#7659=ORIENTED_EDGE('',*,*,#5288,.F.);
#7660=ORIENTED_EDGE('',*,*,#5295,.F.);
#7661=ORIENTED_EDGE('',*,*,#5287,.T.);
#7662=ORIENTED_EDGE('',*,*,#5296,.T.);
#7663=ORIENTED_EDGE('',*,*,#5191,.F.);
#7664=ORIENTED_EDGE('',*,*,#5297,.T.);
#7665=ORIENTED_EDGE('',*,*,#5192,.F.);
#7666=ORIENTED_EDGE('',*,*,#5296,.F.);
#7667=ORIENTED_EDGE('',*,*,#5286,.F.);
#7668=ORIENTED_EDGE('',*,*,#5298,.F.);
#7669=ORIENTED_EDGE('',*,*,#5193,.F.);
#7670=ORIENTED_EDGE('',*,*,#5297,.F.);
#7671=ORIENTED_EDGE('',*,*,#5285,.F.);
#7672=ORIENTED_EDGE('',*,*,#5298,.T.);
#7673=ORIENTED_EDGE('',*,*,#5284,.F.);
#7674=ORIENTED_EDGE('',*,*,#5299,.F.);
#7675=ORIENTED_EDGE('',*,*,#5194,.F.);
#7676=ORIENTED_EDGE('',*,*,#5299,.T.);
#7677=ORIENTED_EDGE('',*,*,#5283,.F.);
#7678=ORIENTED_EDGE('',*,*,#5300,.T.);
#7679=ORIENTED_EDGE('',*,*,#5195,.F.);
#7680=ORIENTED_EDGE('',*,*,#5301,.T.);
#7681=ORIENTED_EDGE('',*,*,#5196,.F.);
#7682=ORIENTED_EDGE('',*,*,#5300,.F.);
#7683=ORIENTED_EDGE('',*,*,#5282,.F.);
#7684=ORIENTED_EDGE('',*,*,#5301,.F.);
#7685=ORIENTED_EDGE('',*,*,#5281,.F.);
#7686=ORIENTED_EDGE('',*,*,#5302,.T.);
#7687=ORIENTED_EDGE('',*,*,#5197,.F.);
#7688=ORIENTED_EDGE('',*,*,#5303,.T.);
#7689=ORIENTED_EDGE('',*,*,#5198,.F.);
#7690=ORIENTED_EDGE('',*,*,#5302,.F.);
#7691=ORIENTED_EDGE('',*,*,#5280,.F.);
#7692=ORIENTED_EDGE('',*,*,#5304,.F.);
#7693=ORIENTED_EDGE('',*,*,#5199,.F.);
#7694=ORIENTED_EDGE('',*,*,#5303,.F.);
#7695=ORIENTED_EDGE('',*,*,#5279,.T.);
#7696=ORIENTED_EDGE('',*,*,#5304,.T.);
#7697=ORIENTED_EDGE('',*,*,#5278,.F.);
#7698=ORIENTED_EDGE('',*,*,#5305,.F.);
#7699=ORIENTED_EDGE('',*,*,#5200,.F.);
#7700=ORIENTED_EDGE('',*,*,#5305,.T.);
#7701=ORIENTED_EDGE('',*,*,#5277,.F.);
#7702=ORIENTED_EDGE('',*,*,#5306,.T.);
#7703=ORIENTED_EDGE('',*,*,#5201,.F.);
#7704=ORIENTED_EDGE('',*,*,#5307,.T.);
#7705=ORIENTED_EDGE('',*,*,#5202,.F.);
#7706=ORIENTED_EDGE('',*,*,#5306,.F.);
#7707=ORIENTED_EDGE('',*,*,#5276,.F.);
#7708=ORIENTED_EDGE('',*,*,#5308,.T.);
#7709=ORIENTED_EDGE('',*,*,#5203,.F.);
#7710=ORIENTED_EDGE('',*,*,#5307,.F.);
#7711=ORIENTED_EDGE('',*,*,#5275,.T.);
#7712=ORIENTED_EDGE('',*,*,#5267,.T.);
#7713=ORIENTED_EDGE('',*,*,#5204,.F.);
#7714=ORIENTED_EDGE('',*,*,#5308,.F.);
#7715=ORIENTED_EDGE('',*,*,#5274,.F.);
#7716=ORIENTED_EDGE('',*,*,#5292,.T.);
#7717=ORIENTED_EDGE('',*,*,#5186,.F.);
#7718=ORIENTED_EDGE('',*,*,#5309,.F.);
#7719=ORIENTED_EDGE('',*,*,#5270,.F.);
#7720=ORIENTED_EDGE('',*,*,#5310,.F.);
#7721=ORIENTED_EDGE('',*,*,#5271,.F.);
#7722=ORIENTED_EDGE('',*,*,#5309,.T.);
#7723=ORIENTED_EDGE('',*,*,#5185,.F.);
#7724=ORIENTED_EDGE('',*,*,#5310,.T.);
#7725=ORIENTED_EDGE('',*,*,#5184,.F.);
#7726=ORIENTED_EDGE('',*,*,#5311,.F.);
#7727=ORIENTED_EDGE('',*,*,#5272,.F.);
#7728=ORIENTED_EDGE('',*,*,#5266,.T.);
#7729=ORIENTED_EDGE('',*,*,#5273,.T.);
#7730=ORIENTED_EDGE('',*,*,#5311,.T.);
#7731=ORIENTED_EDGE('',*,*,#5183,.F.);
#7732=ORIENTED_EDGE('',*,*,#5312,.F.);
#7733=ORIENTED_EDGE('',*,*,#5313,.T.);
#7734=ORIENTED_EDGE('',*,*,#5314,.F.);
#7735=ORIENTED_EDGE('',*,*,#5315,.F.);
#7736=ORIENTED_EDGE('',*,*,#5316,.F.);
#7737=ORIENTED_EDGE('',*,*,#5317,.F.);
#7738=ORIENTED_EDGE('',*,*,#5318,.F.);
#7739=ORIENTED_EDGE('',*,*,#5319,.F.);
#7740=ORIENTED_EDGE('',*,*,#5320,.F.);
#7741=ORIENTED_EDGE('',*,*,#5321,.T.);
#7742=ORIENTED_EDGE('',*,*,#5318,.T.);
#7743=ORIENTED_EDGE('',*,*,#5321,.F.);
#7744=ORIENTED_EDGE('',*,*,#5322,.F.);
#7745=ORIENTED_EDGE('',*,*,#5323,.T.);
#7746=ORIENTED_EDGE('',*,*,#5319,.T.);
#7747=ORIENTED_EDGE('',*,*,#5320,.T.);
#7748=ORIENTED_EDGE('',*,*,#5323,.F.);
#7749=ORIENTED_EDGE('',*,*,#5322,.T.);
#7750=ORIENTED_EDGE('',*,*,#5324,.T.);
#7751=ORIENTED_EDGE('',*,*,#5325,.F.);
#7752=ORIENTED_EDGE('',*,*,#5326,.F.);
#7753=ORIENTED_EDGE('',*,*,#5327,.T.);
#7754=ORIENTED_EDGE('',*,*,#5324,.F.);
#7755=ORIENTED_EDGE('',*,*,#5327,.F.);
#7756=ORIENTED_EDGE('',*,*,#5328,.F.);
#7757=ORIENTED_EDGE('',*,*,#5329,.T.);
#7758=ORIENTED_EDGE('',*,*,#5330,.F.);
#7759=ORIENTED_EDGE('',*,*,#5331,.F.);
#7760=ORIENTED_EDGE('',*,*,#5332,.F.);
#7761=ORIENTED_EDGE('',*,*,#5329,.F.);
#7762=ORIENTED_EDGE('',*,*,#5333,.F.);
#7763=ORIENTED_EDGE('',*,*,#5325,.T.);
#7764=ORIENTED_EDGE('',*,*,#5326,.T.);
#7765=ORIENTED_EDGE('',*,*,#5334,.F.);
#7766=ORIENTED_EDGE('',*,*,#5335,.F.);
#7767=ORIENTED_EDGE('',*,*,#5333,.T.);
#7768=ORIENTED_EDGE('',*,*,#5336,.T.);
#7769=ORIENTED_EDGE('',*,*,#5337,.F.);
#7770=ORIENTED_EDGE('',*,*,#5338,.F.);
#7771=ORIENTED_EDGE('',*,*,#5339,.F.);
#7772=ORIENTED_EDGE('',*,*,#5340,.F.);
#7773=ORIENTED_EDGE('',*,*,#5334,.T.);
#7774=ORIENTED_EDGE('',*,*,#5340,.T.);
#7775=ORIENTED_EDGE('',*,*,#5339,.T.);
#7776=ORIENTED_EDGE('',*,*,#5338,.T.);
#7777=ORIENTED_EDGE('',*,*,#5341,.T.);
#7778=ORIENTED_EDGE('',*,*,#5342,.F.);
#7779=ORIENTED_EDGE('',*,*,#5343,.F.);
#7780=ORIENTED_EDGE('',*,*,#5344,.F.);
#7781=ORIENTED_EDGE('',*,*,#5335,.T.);
#7782=ORIENTED_EDGE('',*,*,#5344,.T.);
#7783=ORIENTED_EDGE('',*,*,#5345,.F.);
#7784=ORIENTED_EDGE('',*,*,#5336,.F.);
#7785=ORIENTED_EDGE('',*,*,#5345,.T.);
#7786=ORIENTED_EDGE('',*,*,#5346,.T.);
#7787=ORIENTED_EDGE('',*,*,#5347,.F.);
#7788=ORIENTED_EDGE('',*,*,#5348,.F.);
#7789=ORIENTED_EDGE('',*,*,#5342,.T.);
#7790=ORIENTED_EDGE('',*,*,#5341,.F.);
#7791=ORIENTED_EDGE('',*,*,#5337,.T.);
#7792=ORIENTED_EDGE('',*,*,#5348,.T.);
#7793=ORIENTED_EDGE('',*,*,#5349,.F.);
#7794=ORIENTED_EDGE('',*,*,#5350,.F.);
#7795=ORIENTED_EDGE('',*,*,#5350,.T.);
#7796=ORIENTED_EDGE('',*,*,#5351,.T.);
#7797=ORIENTED_EDGE('',*,*,#5352,.F.);
#7798=ORIENTED_EDGE('',*,*,#5346,.F.);
#7799=ORIENTED_EDGE('',*,*,#5343,.T.);
#7800=ORIENTED_EDGE('',*,*,#5353,.T.);
#7801=ORIENTED_EDGE('',*,*,#5354,.T.);
#7802=ORIENTED_EDGE('',*,*,#5355,.F.);
#7803=ORIENTED_EDGE('',*,*,#5356,.F.);
#7804=ORIENTED_EDGE('',*,*,#5352,.T.);
#7805=ORIENTED_EDGE('',*,*,#5353,.F.);
#7806=ORIENTED_EDGE('',*,*,#5351,.F.);
#7807=ORIENTED_EDGE('',*,*,#5349,.T.);
#7808=ORIENTED_EDGE('',*,*,#5357,.T.);
#7809=ORIENTED_EDGE('',*,*,#5358,.F.);
#7810=ORIENTED_EDGE('',*,*,#5354,.F.);
#7811=ORIENTED_EDGE('',*,*,#5358,.T.);
#7812=ORIENTED_EDGE('',*,*,#5359,.T.);
#7813=ORIENTED_EDGE('',*,*,#5360,.F.);
#7814=ORIENTED_EDGE('',*,*,#5361,.F.);
#7815=ORIENTED_EDGE('',*,*,#5361,.T.);
#7816=ORIENTED_EDGE('',*,*,#5330,.T.);
#7817=ORIENTED_EDGE('',*,*,#5332,.T.);
#7818=ORIENTED_EDGE('',*,*,#5362,.F.);
#7819=ORIENTED_EDGE('',*,*,#5363,.F.);
#7820=ORIENTED_EDGE('',*,*,#5355,.T.);
#7821=ORIENTED_EDGE('',*,*,#5364,.T.);
#7822=ORIENTED_EDGE('',*,*,#5363,.T.);
#7823=ORIENTED_EDGE('',*,*,#5365,.F.);
#7824=ORIENTED_EDGE('',*,*,#5359,.F.);
#7825=ORIENTED_EDGE('',*,*,#5347,.T.);
#7826=ORIENTED_EDGE('',*,*,#5356,.T.);
#7827=ORIENTED_EDGE('',*,*,#5364,.F.);
#7828=ORIENTED_EDGE('',*,*,#5357,.F.);
#7829=ORIENTED_EDGE('',*,*,#5360,.T.);
#7830=ORIENTED_EDGE('',*,*,#5365,.T.);
#7831=ORIENTED_EDGE('',*,*,#5362,.T.);
#7832=ORIENTED_EDGE('',*,*,#5331,.T.);
#7833=ORIENTED_EDGE('',*,*,#5366,.T.);
#7834=ORIENTED_EDGE('',*,*,#5328,.T.);
#7835=ORIENTED_EDGE('',*,*,#5366,.F.);
#7836=ORIENTED_EDGE('',*,*,#5367,.T.);
#7837=ORIENTED_EDGE('',*,*,#5368,.T.);
#7838=ORIENTED_EDGE('',*,*,#5367,.F.);
#7839=ORIENTED_EDGE('',*,*,#5369,.T.);
#7840=ORIENTED_EDGE('',*,*,#5370,.T.);
#7841=ORIENTED_EDGE('',*,*,#5371,.T.);
#7842=ORIENTED_EDGE('',*,*,#5368,.F.);
#7843=ORIENTED_EDGE('',*,*,#5371,.F.);
#7844=ORIENTED_EDGE('',*,*,#5372,.T.);
#7845=ORIENTED_EDGE('',*,*,#5373,.T.);
#7846=ORIENTED_EDGE('',*,*,#5372,.F.);
#7847=ORIENTED_EDGE('',*,*,#5374,.F.);
#7848=ORIENTED_EDGE('',*,*,#5375,.F.);
#7849=ORIENTED_EDGE('',*,*,#5376,.F.);
#7850=ORIENTED_EDGE('',*,*,#5377,.F.);
#7851=ORIENTED_EDGE('',*,*,#5378,.F.);
#7852=ORIENTED_EDGE('',*,*,#5379,.F.);
#7853=ORIENTED_EDGE('',*,*,#5380,.F.);
#7854=ORIENTED_EDGE('',*,*,#5381,.F.);
#7855=ORIENTED_EDGE('',*,*,#5382,.F.);
#7856=ORIENTED_EDGE('',*,*,#5383,.F.);
#7857=ORIENTED_EDGE('',*,*,#5384,.F.);
#7858=ORIENTED_EDGE('',*,*,#5385,.F.);
#7859=ORIENTED_EDGE('',*,*,#5386,.F.);
#7860=ORIENTED_EDGE('',*,*,#5387,.F.);
#7861=ORIENTED_EDGE('',*,*,#5388,.F.);
#7862=ORIENTED_EDGE('',*,*,#5389,.T.);
#7863=ORIENTED_EDGE('',*,*,#5373,.F.);
#7864=ORIENTED_EDGE('',*,*,#5390,.T.);
#7865=ORIENTED_EDGE('',*,*,#5391,.T.);
#7866=ORIENTED_EDGE('',*,*,#5389,.F.);
#7867=ORIENTED_EDGE('',*,*,#5391,.F.);
#7868=ORIENTED_EDGE('',*,*,#5392,.T.);
#7869=ORIENTED_EDGE('',*,*,#5393,.T.);
#7870=ORIENTED_EDGE('',*,*,#5394,.T.);
#7871=ORIENTED_EDGE('',*,*,#5395,.T.);
#7872=ORIENTED_EDGE('',*,*,#5390,.F.);
#7873=ORIENTED_EDGE('',*,*,#5392,.F.);
#7874=ORIENTED_EDGE('',*,*,#5396,.T.);
#7875=ORIENTED_EDGE('',*,*,#5397,.F.);
#7876=ORIENTED_EDGE('',*,*,#5398,.F.);
#7877=ORIENTED_EDGE('',*,*,#5399,.F.);
#7878=ORIENTED_EDGE('',*,*,#5398,.T.);
#7879=ORIENTED_EDGE('',*,*,#5400,.T.);
#7880=ORIENTED_EDGE('',*,*,#5401,.F.);
#7881=ORIENTED_EDGE('',*,*,#5402,.F.);
#7882=ORIENTED_EDGE('',*,*,#5393,.F.);
#7883=ORIENTED_EDGE('',*,*,#5399,.T.);
#7884=ORIENTED_EDGE('',*,*,#5403,.T.);
#7885=ORIENTED_EDGE('',*,*,#5404,.F.);
#7886=ORIENTED_EDGE('',*,*,#5405,.T.);
#7887=ORIENTED_EDGE('',*,*,#5402,.T.);
#7888=ORIENTED_EDGE('',*,*,#5406,.F.);
#7889=ORIENTED_EDGE('',*,*,#5407,.T.);
#7890=ORIENTED_EDGE('',*,*,#5408,.T.);
#7891=ORIENTED_EDGE('',*,*,#5404,.T.);
#7892=ORIENTED_EDGE('',*,*,#5409,.T.);
#7893=ORIENTED_EDGE('',*,*,#5407,.F.);
#7894=ORIENTED_EDGE('',*,*,#5410,.T.);
#7895=ORIENTED_EDGE('',*,*,#5386,.T.);
#7896=ORIENTED_EDGE('',*,*,#5411,.F.);
#7897=ORIENTED_EDGE('',*,*,#5412,.F.);
#7898=ORIENTED_EDGE('',*,*,#5411,.T.);
#7899=ORIENTED_EDGE('',*,*,#5385,.T.);
#7900=ORIENTED_EDGE('',*,*,#5413,.F.);
#7901=ORIENTED_EDGE('',*,*,#5412,.T.);
#7902=ORIENTED_EDGE('',*,*,#5414,.T.);
#7903=ORIENTED_EDGE('',*,*,#5415,.T.);
#7904=ORIENTED_EDGE('',*,*,#5408,.F.);
#7905=ORIENTED_EDGE('',*,*,#5415,.F.);
#7906=ORIENTED_EDGE('',*,*,#5416,.F.);
#7907=ORIENTED_EDGE('',*,*,#5394,.F.);
#7908=ORIENTED_EDGE('',*,*,#5405,.F.);
#7909=ORIENTED_EDGE('',*,*,#5395,.F.);
#7910=ORIENTED_EDGE('',*,*,#5416,.T.);
#7911=ORIENTED_EDGE('',*,*,#5417,.T.);
#7912=ORIENTED_EDGE('',*,*,#5396,.F.);
#7913=ORIENTED_EDGE('',*,*,#5418,.T.);
#7914=ORIENTED_EDGE('',*,*,#5419,.T.);
#7915=ORIENTED_EDGE('',*,*,#5417,.F.);
#7916=ORIENTED_EDGE('',*,*,#5414,.F.);
#7917=ORIENTED_EDGE('',*,*,#5418,.F.);
#7918=ORIENTED_EDGE('',*,*,#5413,.T.);
#7919=ORIENTED_EDGE('',*,*,#5384,.T.);
#7920=ORIENTED_EDGE('',*,*,#5420,.F.);
#7921=ORIENTED_EDGE('',*,*,#5421,.F.);
#7922=ORIENTED_EDGE('',*,*,#5420,.T.);
#7923=ORIENTED_EDGE('',*,*,#5383,.T.);
#7924=ORIENTED_EDGE('',*,*,#5422,.F.);
#7925=ORIENTED_EDGE('',*,*,#5421,.T.);
#7926=ORIENTED_EDGE('',*,*,#5423,.F.);
#7927=ORIENTED_EDGE('',*,*,#5397,.T.);
#7928=ORIENTED_EDGE('',*,*,#5419,.F.);
#7929=ORIENTED_EDGE('',*,*,#5424,.T.);
#7930=ORIENTED_EDGE('',*,*,#5425,.T.);
#7931=ORIENTED_EDGE('',*,*,#5400,.F.);
#7932=ORIENTED_EDGE('',*,*,#5423,.T.);
#7933=ORIENTED_EDGE('',*,*,#5424,.F.);
#7934=ORIENTED_EDGE('',*,*,#5422,.T.);
#7935=ORIENTED_EDGE('',*,*,#5382,.T.);
#7936=ORIENTED_EDGE('',*,*,#5426,.F.);
#7937=ORIENTED_EDGE('',*,*,#5427,.F.);
#7938=ORIENTED_EDGE('',*,*,#5426,.T.);
#7939=ORIENTED_EDGE('',*,*,#5381,.T.);
#7940=ORIENTED_EDGE('',*,*,#5428,.F.);
#7941=ORIENTED_EDGE('',*,*,#5429,.T.);
#7942=ORIENTED_EDGE('',*,*,#5409,.F.);
#7943=ORIENTED_EDGE('',*,*,#5406,.T.);
#7944=ORIENTED_EDGE('',*,*,#5403,.F.);
#7945=ORIENTED_EDGE('',*,*,#5401,.T.);
#7946=ORIENTED_EDGE('',*,*,#5425,.F.);
#7947=ORIENTED_EDGE('',*,*,#5427,.T.);
#7948=ORIENTED_EDGE('',*,*,#5430,.F.);
#7949=ORIENTED_EDGE('',*,*,#5431,.T.);
#7950=ORIENTED_EDGE('',*,*,#5432,.T.);
#7951=ORIENTED_EDGE('',*,*,#5429,.F.);
#7952=ORIENTED_EDGE('',*,*,#5433,.T.);
#7953=ORIENTED_EDGE('',*,*,#5387,.T.);
#7954=ORIENTED_EDGE('',*,*,#5410,.F.);
#7955=ORIENTED_EDGE('',*,*,#5434,.F.);
#7956=ORIENTED_EDGE('',*,*,#5435,.T.);
#7957=ORIENTED_EDGE('',*,*,#5388,.T.);
#7958=ORIENTED_EDGE('',*,*,#5433,.F.);
#7959=ORIENTED_EDGE('',*,*,#5434,.T.);
#7960=ORIENTED_EDGE('',*,*,#5432,.F.);
#7961=ORIENTED_EDGE('',*,*,#5436,.T.);
#7962=ORIENTED_EDGE('',*,*,#5437,.T.);
#7963=ORIENTED_EDGE('',*,*,#5438,.T.);
#7964=ORIENTED_EDGE('',*,*,#5439,.T.);
#7965=ORIENTED_EDGE('',*,*,#5440,.T.);
#7966=ORIENTED_EDGE('',*,*,#5439,.F.);
#7967=ORIENTED_EDGE('',*,*,#5441,.F.);
#7968=ORIENTED_EDGE('',*,*,#5442,.T.);
#7969=ORIENTED_EDGE('',*,*,#5443,.F.);
#7970=ORIENTED_EDGE('',*,*,#5440,.F.);
#7971=ORIENTED_EDGE('',*,*,#5444,.F.);
#7972=ORIENTED_EDGE('',*,*,#5445,.T.);
#7973=ORIENTED_EDGE('',*,*,#5374,.T.);
#7974=ORIENTED_EDGE('',*,*,#5435,.F.);
#7975=ORIENTED_EDGE('',*,*,#5375,.T.);
#7976=ORIENTED_EDGE('',*,*,#5445,.F.);
#7977=ORIENTED_EDGE('',*,*,#5446,.T.);
#7978=ORIENTED_EDGE('',*,*,#5447,.T.);
#7979=ORIENTED_EDGE('',*,*,#5448,.F.);
#7980=ORIENTED_EDGE('',*,*,#5449,.T.);
#7981=ORIENTED_EDGE('',*,*,#5376,.T.);
#7982=ORIENTED_EDGE('',*,*,#5447,.F.);
#7983=ORIENTED_EDGE('',*,*,#5448,.T.);
#7984=ORIENTED_EDGE('',*,*,#5450,.T.);
#7985=ORIENTED_EDGE('',*,*,#5451,.F.);
#7986=ORIENTED_EDGE('',*,*,#5452,.F.);
#7987=ORIENTED_EDGE('',*,*,#5453,.T.);
#7988=ORIENTED_EDGE('',*,*,#5454,.F.);
#7989=ORIENTED_EDGE('',*,*,#5455,.F.);
#7990=ORIENTED_EDGE('',*,*,#5456,.F.);
#7991=ORIENTED_EDGE('',*,*,#5457,.T.);
#7992=ORIENTED_EDGE('',*,*,#5456,.T.);
#7993=ORIENTED_EDGE('',*,*,#5458,.T.);
#7994=ORIENTED_EDGE('',*,*,#5457,.F.);
#7995=ORIENTED_EDGE('',*,*,#5459,.T.);
#7996=ORIENTED_EDGE('',*,*,#5377,.T.);
#7997=ORIENTED_EDGE('',*,*,#5449,.F.);
#7998=ORIENTED_EDGE('',*,*,#5460,.F.);
#7999=ORIENTED_EDGE('',*,*,#5461,.T.);
#8000=ORIENTED_EDGE('',*,*,#5378,.T.);
#8001=ORIENTED_EDGE('',*,*,#5459,.F.);
#8002=ORIENTED_EDGE('',*,*,#5460,.T.);
#8003=ORIENTED_EDGE('',*,*,#5458,.F.);
#8004=ORIENTED_EDGE('',*,*,#5455,.T.);
#8005=ORIENTED_EDGE('',*,*,#5462,.T.);
#8006=ORIENTED_EDGE('',*,*,#5463,.T.);
#8007=ORIENTED_EDGE('',*,*,#5464,.T.);
#8008=ORIENTED_EDGE('',*,*,#5464,.F.);
#8009=ORIENTED_EDGE('',*,*,#5465,.T.);
#8010=ORIENTED_EDGE('',*,*,#5466,.T.);
#8011=ORIENTED_EDGE('',*,*,#5461,.F.);
#8012=ORIENTED_EDGE('',*,*,#5467,.F.);
#8013=ORIENTED_EDGE('',*,*,#5379,.T.);
#8014=ORIENTED_EDGE('',*,*,#5466,.F.);
#8015=ORIENTED_EDGE('',*,*,#5468,.F.);
#8016=ORIENTED_EDGE('',*,*,#5469,.F.);
#8017=ORIENTED_EDGE('',*,*,#5470,.T.);
#8018=ORIENTED_EDGE('',*,*,#5467,.T.);
#8019=ORIENTED_EDGE('',*,*,#5471,.F.);
#8020=ORIENTED_EDGE('',*,*,#5472,.T.);
#8021=ORIENTED_EDGE('',*,*,#5469,.T.);
#8022=ORIENTED_EDGE('',*,*,#5473,.T.);
#8023=ORIENTED_EDGE('',*,*,#5474,.T.);
#8024=ORIENTED_EDGE('',*,*,#5475,.T.);
#8025=ORIENTED_EDGE('',*,*,#5430,.T.);
#8026=ORIENTED_EDGE('',*,*,#5476,.F.);
#8027=ORIENTED_EDGE('',*,*,#5477,.F.);
#8028=ORIENTED_EDGE('',*,*,#5478,.T.);
#8029=ORIENTED_EDGE('',*,*,#5476,.T.);
#8030=ORIENTED_EDGE('',*,*,#5478,.F.);
#8031=ORIENTED_EDGE('',*,*,#5477,.T.);
#8032=ORIENTED_EDGE('',*,*,#5479,.F.);
#8033=ORIENTED_EDGE('',*,*,#5480,.F.);
#8034=ORIENTED_EDGE('',*,*,#5481,.T.);
#8035=ORIENTED_EDGE('',*,*,#5370,.F.);
#8036=ORIENTED_EDGE('',*,*,#5482,.T.);
#8037=ORIENTED_EDGE('',*,*,#5479,.T.);
#8038=ORIENTED_EDGE('',*,*,#5482,.F.);
#8039=ORIENTED_EDGE('',*,*,#5369,.F.);
#8040=ORIENTED_EDGE('',*,*,#5481,.F.);
#8041=ORIENTED_EDGE('',*,*,#5483,.F.);
#8042=ORIENTED_EDGE('',*,*,#5484,.T.);
#8043=ORIENTED_EDGE('',*,*,#5485,.T.);
#8044=ORIENTED_EDGE('',*,*,#5486,.F.);
#8045=ORIENTED_EDGE('',*,*,#5487,.F.);
#8046=ORIENTED_EDGE('',*,*,#5488,.F.);
#8047=ORIENTED_EDGE('',*,*,#5451,.T.);
#8048=ORIENTED_EDGE('',*,*,#5489,.T.);
#8049=ORIENTED_EDGE('',*,*,#5480,.T.);
#8050=ORIENTED_EDGE('',*,*,#5442,.F.);
#8051=ORIENTED_EDGE('',*,*,#5490,.F.);
#8052=ORIENTED_EDGE('',*,*,#5483,.T.);
#8053=ORIENTED_EDGE('',*,*,#5491,.T.);
#8054=ORIENTED_EDGE('',*,*,#5443,.T.);
#8055=ORIENTED_EDGE('',*,*,#5491,.F.);
#8056=ORIENTED_EDGE('',*,*,#5489,.F.);
#8057=ORIENTED_EDGE('',*,*,#5450,.F.);
#8058=ORIENTED_EDGE('',*,*,#5446,.F.);
#8059=ORIENTED_EDGE('',*,*,#5444,.T.);
#8060=ORIENTED_EDGE('',*,*,#5492,.F.);
#8061=ORIENTED_EDGE('',*,*,#5493,.T.);
#8062=ORIENTED_EDGE('',*,*,#5484,.F.);
#8063=ORIENTED_EDGE('',*,*,#5490,.T.);
#8064=ORIENTED_EDGE('',*,*,#5492,.T.);
#8065=ORIENTED_EDGE('',*,*,#5441,.T.);
#8066=ORIENTED_EDGE('',*,*,#5438,.F.);
#8067=ORIENTED_EDGE('',*,*,#5494,.F.);
#8068=ORIENTED_EDGE('',*,*,#5495,.T.);
#8069=ORIENTED_EDGE('',*,*,#5496,.F.);
#8070=ORIENTED_EDGE('',*,*,#5497,.T.);
#8071=ORIENTED_EDGE('',*,*,#5494,.T.);
#8072=ORIENTED_EDGE('',*,*,#5437,.F.);
#8073=ORIENTED_EDGE('',*,*,#5498,.F.);
#8074=ORIENTED_EDGE('',*,*,#5495,.F.);
#8075=ORIENTED_EDGE('',*,*,#5499,.T.);
#8076=ORIENTED_EDGE('',*,*,#5315,.T.);
#8077=ORIENTED_EDGE('',*,*,#5500,.F.);
#8078=ORIENTED_EDGE('',*,*,#5498,.T.);
#8079=ORIENTED_EDGE('',*,*,#5501,.T.);
#8080=ORIENTED_EDGE('',*,*,#5502,.F.);
#8081=ORIENTED_EDGE('',*,*,#5486,.T.);
#8082=ORIENTED_EDGE('',*,*,#5503,.F.);
#8083=ORIENTED_EDGE('',*,*,#5496,.T.);
#8084=ORIENTED_EDGE('',*,*,#5497,.F.);
#8085=ORIENTED_EDGE('',*,*,#5503,.T.);
#8086=ORIENTED_EDGE('',*,*,#5485,.F.);
#8087=ORIENTED_EDGE('',*,*,#5493,.F.);
#8088=ORIENTED_EDGE('',*,*,#5504,.T.);
#8089=ORIENTED_EDGE('',*,*,#5505,.F.);
#8090=ORIENTED_EDGE('',*,*,#5487,.T.);
#8091=ORIENTED_EDGE('',*,*,#5502,.T.);
#8092=ORIENTED_EDGE('',*,*,#5504,.F.);
#8093=ORIENTED_EDGE('',*,*,#5506,.T.);
#8094=ORIENTED_EDGE('',*,*,#5507,.T.);
#8095=ORIENTED_EDGE('',*,*,#5508,.F.);
#8096=ORIENTED_EDGE('',*,*,#5509,.F.);
#8097=ORIENTED_EDGE('',*,*,#5508,.T.);
#8098=ORIENTED_EDGE('',*,*,#5510,.T.);
#8099=ORIENTED_EDGE('',*,*,#5511,.F.);
#8100=ORIENTED_EDGE('',*,*,#5509,.T.);
#8101=ORIENTED_EDGE('',*,*,#5452,.T.);
#8102=ORIENTED_EDGE('',*,*,#5488,.T.);
#8103=ORIENTED_EDGE('',*,*,#5505,.T.);
#8104=ORIENTED_EDGE('',*,*,#5453,.F.);
#8105=ORIENTED_EDGE('',*,*,#5511,.T.);
#8106=ORIENTED_EDGE('',*,*,#5512,.T.);
#8107=ORIENTED_EDGE('',*,*,#5513,.F.);
#8108=ORIENTED_EDGE('',*,*,#5514,.F.);
#8109=ORIENTED_EDGE('',*,*,#5513,.T.);
#8110=ORIENTED_EDGE('',*,*,#5515,.T.);
#8111=ORIENTED_EDGE('',*,*,#5516,.F.);
#8112=ORIENTED_EDGE('',*,*,#5514,.T.);
#8113=ORIENTED_EDGE('',*,*,#5462,.F.);
#8114=ORIENTED_EDGE('',*,*,#5454,.T.);
#8115=ORIENTED_EDGE('',*,*,#5463,.F.);
#8116=ORIENTED_EDGE('',*,*,#5516,.T.);
#8117=ORIENTED_EDGE('',*,*,#5517,.T.);
#8118=ORIENTED_EDGE('',*,*,#5465,.F.);
#8119=ORIENTED_EDGE('',*,*,#5518,.F.);
#8120=ORIENTED_EDGE('',*,*,#5468,.T.);
#8121=ORIENTED_EDGE('',*,*,#5517,.F.);
#8122=ORIENTED_EDGE('',*,*,#5515,.F.);
#8123=ORIENTED_EDGE('',*,*,#5512,.F.);
#8124=ORIENTED_EDGE('',*,*,#5510,.F.);
#8125=ORIENTED_EDGE('',*,*,#5519,.F.);
#8126=ORIENTED_EDGE('',*,*,#5473,.F.);
#8127=ORIENTED_EDGE('',*,*,#5471,.T.);
#8128=ORIENTED_EDGE('',*,*,#5518,.T.);
#8129=ORIENTED_EDGE('',*,*,#5520,.F.);
#8130=ORIENTED_EDGE('',*,*,#5474,.F.);
#8131=ORIENTED_EDGE('',*,*,#5520,.T.);
#8132=ORIENTED_EDGE('',*,*,#5521,.T.);
#8133=ORIENTED_EDGE('',*,*,#5522,.F.);
#8134=ORIENTED_EDGE('',*,*,#5475,.F.);
#8135=ORIENTED_EDGE('',*,*,#5522,.T.);
#8136=ORIENTED_EDGE('',*,*,#5312,.T.);
#8137=ORIENTED_EDGE('',*,*,#5523,.F.);
#8138=ORIENTED_EDGE('',*,*,#5431,.F.);
#8139=ORIENTED_EDGE('',*,*,#5523,.T.);
#8140=ORIENTED_EDGE('',*,*,#5317,.T.);
#8141=ORIENTED_EDGE('',*,*,#5524,.F.);
#8142=ORIENTED_EDGE('',*,*,#5436,.F.);
#8143=ORIENTED_EDGE('',*,*,#5524,.T.);
#8144=ORIENTED_EDGE('',*,*,#5316,.T.);
#8145=ORIENTED_EDGE('',*,*,#5499,.F.);
#8146=ORIENTED_EDGE('',*,*,#5521,.F.);
#8147=ORIENTED_EDGE('',*,*,#5519,.T.);
#8148=ORIENTED_EDGE('',*,*,#5507,.F.);
#8149=ORIENTED_EDGE('',*,*,#5313,.F.);
#8150=ORIENTED_EDGE('',*,*,#5501,.F.);
#8151=ORIENTED_EDGE('',*,*,#5500,.T.);
#8152=ORIENTED_EDGE('',*,*,#5314,.T.);
#8153=ORIENTED_EDGE('',*,*,#5506,.F.);
#8154=ORIENTED_EDGE('',*,*,#5472,.F.);
#8155=ORIENTED_EDGE('',*,*,#5428,.T.);
#8156=ORIENTED_EDGE('',*,*,#5380,.T.);
#8157=ORIENTED_EDGE('',*,*,#5470,.F.);
#8158=ORIENTED_EDGE('',*,*,#5525,.T.);
#8159=ORIENTED_EDGE('',*,*,#5526,.F.);
#8160=ORIENTED_EDGE('',*,*,#5526,.T.);
#8161=ORIENTED_EDGE('',*,*,#5527,.T.);
#8162=ORIENTED_EDGE('',*,*,#5528,.F.);
#8163=ORIENTED_EDGE('',*,*,#5527,.F.);
#8164=ORIENTED_EDGE('',*,*,#5529,.T.);
#8165=ORIENTED_EDGE('',*,*,#5528,.T.);
#8166=ORIENTED_EDGE('',*,*,#5529,.F.);
#8167=ORIENTED_EDGE('',*,*,#5530,.T.);
#8168=ORIENTED_EDGE('',*,*,#5525,.F.);
#8169=ORIENTED_EDGE('',*,*,#5530,.F.);
#8170=ORIENTED_EDGE('',*,*,#5531,.F.);
#8171=ORIENTED_EDGE('',*,*,#5532,.T.);
#8172=ORIENTED_EDGE('',*,*,#5533,.F.);
#8173=ORIENTED_EDGE('',*,*,#5534,.T.);
#8174=ORIENTED_EDGE('',*,*,#5535,.T.);
#8175=ORIENTED_EDGE('',*,*,#5536,.F.);
#8176=ORIENTED_EDGE('',*,*,#5537,.F.);
#8177=ORIENTED_EDGE('',*,*,#5538,.T.);
#8178=ORIENTED_EDGE('',*,*,#5536,.T.);
#8179=ORIENTED_EDGE('',*,*,#5538,.F.);
#8180=ORIENTED_EDGE('',*,*,#5539,.T.);
#8181=ORIENTED_EDGE('',*,*,#5537,.T.);
#8182=ORIENTED_EDGE('',*,*,#5540,.T.);
#8183=ORIENTED_EDGE('',*,*,#5541,.F.);
#8184=ORIENTED_EDGE('',*,*,#5542,.T.);
#8185=ORIENTED_EDGE('',*,*,#5543,.F.);
#8186=ORIENTED_EDGE('',*,*,#5544,.T.);
#8187=ORIENTED_EDGE('',*,*,#5545,.F.);
#8188=ORIENTED_EDGE('',*,*,#5546,.T.);
#8189=ORIENTED_EDGE('',*,*,#5547,.F.);
#8190=ORIENTED_EDGE('',*,*,#5548,.T.);
#8191=ORIENTED_EDGE('',*,*,#5549,.F.);
#8192=ORIENTED_EDGE('',*,*,#5550,.T.);
#8193=ORIENTED_EDGE('',*,*,#5539,.F.);
#8194=ORIENTED_EDGE('',*,*,#5550,.F.);
#8195=ORIENTED_EDGE('',*,*,#5551,.F.);
#8196=ORIENTED_EDGE('',*,*,#5552,.T.);
#8197=ORIENTED_EDGE('',*,*,#5553,.F.);
#8198=ORIENTED_EDGE('',*,*,#5554,.F.);
#8199=ORIENTED_EDGE('',*,*,#5555,.F.);
#8200=ORIENTED_EDGE('',*,*,#5540,.F.);
#8201=ORIENTED_EDGE('',*,*,#5556,.T.);
#8202=ORIENTED_EDGE('',*,*,#5554,.T.);
#8203=ORIENTED_EDGE('',*,*,#5557,.F.);
#8204=ORIENTED_EDGE('',*,*,#5558,.T.);
#8205=ORIENTED_EDGE('',*,*,#5559,.F.);
#8206=ORIENTED_EDGE('',*,*,#5560,.T.);
#8207=ORIENTED_EDGE('',*,*,#5561,.F.);
#8208=ORIENTED_EDGE('',*,*,#5562,.T.);
#8209=ORIENTED_EDGE('',*,*,#5563,.F.);
#8210=ORIENTED_EDGE('',*,*,#5564,.T.);
#8211=ORIENTED_EDGE('',*,*,#5565,.F.);
#8212=ORIENTED_EDGE('',*,*,#5566,.T.);
#8213=ORIENTED_EDGE('',*,*,#5567,.F.);
#8214=ORIENTED_EDGE('',*,*,#5568,.T.);
#8215=ORIENTED_EDGE('',*,*,#5568,.F.);
#8216=ORIENTED_EDGE('',*,*,#5569,.T.);
#8217=ORIENTED_EDGE('',*,*,#5570,.T.);
#8218=ORIENTED_EDGE('',*,*,#5571,.T.);
#8219=ORIENTED_EDGE('',*,*,#5572,.T.);
#8220=ORIENTED_EDGE('',*,*,#5569,.F.);
#8221=ORIENTED_EDGE('',*,*,#5571,.F.);
#8222=ORIENTED_EDGE('',*,*,#5573,.F.);
#8223=ORIENTED_EDGE('',*,*,#5574,.F.);
#8224=ORIENTED_EDGE('',*,*,#5575,.F.);
#8225=ORIENTED_EDGE('',*,*,#5576,.T.);
#8226=ORIENTED_EDGE('',*,*,#5577,.T.);
#8227=ORIENTED_EDGE('',*,*,#5575,.T.);
#8228=ORIENTED_EDGE('',*,*,#5578,.F.);
#8229=ORIENTED_EDGE('',*,*,#5579,.F.);
#8230=ORIENTED_EDGE('',*,*,#5580,.F.);
#8231=ORIENTED_EDGE('',*,*,#5581,.F.);
#8232=ORIENTED_EDGE('',*,*,#5582,.T.);
#8233=ORIENTED_EDGE('',*,*,#5583,.T.);
#8234=ORIENTED_EDGE('',*,*,#5576,.F.);
#8235=ORIENTED_EDGE('',*,*,#5584,.T.);
#8236=ORIENTED_EDGE('',*,*,#5580,.T.);
#8237=ORIENTED_EDGE('',*,*,#5579,.T.);
#8238=ORIENTED_EDGE('',*,*,#5585,.F.);
#8239=ORIENTED_EDGE('',*,*,#5586,.F.);
#8240=ORIENTED_EDGE('',*,*,#5534,.F.);
#8241=ORIENTED_EDGE('',*,*,#5533,.T.);
#8242=ORIENTED_EDGE('',*,*,#5587,.T.);
#8243=ORIENTED_EDGE('',*,*,#5581,.T.);
#8244=ORIENTED_EDGE('',*,*,#5584,.F.);
#8245=ORIENTED_EDGE('',*,*,#5588,.F.);
#8246=ORIENTED_EDGE('',*,*,#5589,.F.);
#8247=ORIENTED_EDGE('',*,*,#5535,.F.);
#8248=ORIENTED_EDGE('',*,*,#5588,.T.);
#8249=ORIENTED_EDGE('',*,*,#5586,.T.);
#8250=ORIENTED_EDGE('',*,*,#5587,.F.);
#8251=ORIENTED_EDGE('',*,*,#5532,.F.);
#8252=ORIENTED_EDGE('',*,*,#5531,.T.);
#8253=ORIENTED_EDGE('',*,*,#5589,.T.);
#8254=ORIENTED_EDGE('',*,*,#5590,.T.);
#8255=ORIENTED_EDGE('',*,*,#5590,.F.);
#8256=ORIENTED_EDGE('',*,*,#5585,.T.);
#8257=ORIENTED_EDGE('',*,*,#5591,.T.);
#8258=ORIENTED_EDGE('',*,*,#5582,.F.);
#8259=ORIENTED_EDGE('',*,*,#5591,.F.);
#8260=ORIENTED_EDGE('',*,*,#5578,.T.);
#8261=ORIENTED_EDGE('',*,*,#5574,.T.);
#8262=ORIENTED_EDGE('',*,*,#5592,.F.);
#8263=ORIENTED_EDGE('',*,*,#5577,.F.);
#8264=ORIENTED_EDGE('',*,*,#5583,.F.);
#8265=ORIENTED_EDGE('',*,*,#5592,.T.);
#8266=ORIENTED_EDGE('',*,*,#5573,.T.);
#8267=ORIENTED_EDGE('',*,*,#5570,.F.);
#8268=ORIENTED_EDGE('',*,*,#5572,.F.);
#8269=ORIENTED_EDGE('',*,*,#5555,.T.);
#8270=ORIENTED_EDGE('',*,*,#5567,.T.);
#8271=ORIENTED_EDGE('',*,*,#5593,.F.);
#8272=ORIENTED_EDGE('',*,*,#5541,.T.);
#8273=ORIENTED_EDGE('',*,*,#5566,.F.);
#8274=ORIENTED_EDGE('',*,*,#5594,.F.);
#8275=ORIENTED_EDGE('',*,*,#5542,.F.);
#8276=ORIENTED_EDGE('',*,*,#5593,.T.);
#8277=ORIENTED_EDGE('',*,*,#5594,.T.);
#8278=ORIENTED_EDGE('',*,*,#5565,.T.);
#8279=ORIENTED_EDGE('',*,*,#5595,.F.);
#8280=ORIENTED_EDGE('',*,*,#5543,.T.);
#8281=ORIENTED_EDGE('',*,*,#5564,.F.);
#8282=ORIENTED_EDGE('',*,*,#5596,.F.);
#8283=ORIENTED_EDGE('',*,*,#5544,.F.);
#8284=ORIENTED_EDGE('',*,*,#5595,.T.);
#8285=ORIENTED_EDGE('',*,*,#5596,.T.);
#8286=ORIENTED_EDGE('',*,*,#5563,.T.);
#8287=ORIENTED_EDGE('',*,*,#5597,.F.);
#8288=ORIENTED_EDGE('',*,*,#5545,.T.);
#8289=ORIENTED_EDGE('',*,*,#5562,.F.);
#8290=ORIENTED_EDGE('',*,*,#5598,.F.);
#8291=ORIENTED_EDGE('',*,*,#5546,.F.);
#8292=ORIENTED_EDGE('',*,*,#5597,.T.);
#8293=ORIENTED_EDGE('',*,*,#5556,.F.);
#8294=ORIENTED_EDGE('',*,*,#5553,.T.);
#8295=ORIENTED_EDGE('',*,*,#5599,.T.);
#8296=ORIENTED_EDGE('',*,*,#5557,.T.);
#8297=ORIENTED_EDGE('',*,*,#5558,.F.);
#8298=ORIENTED_EDGE('',*,*,#5599,.F.);
#8299=ORIENTED_EDGE('',*,*,#5552,.F.);
#8300=ORIENTED_EDGE('',*,*,#5600,.T.);
#8301=ORIENTED_EDGE('',*,*,#5601,.T.);
#8302=ORIENTED_EDGE('',*,*,#5559,.T.);
#8303=ORIENTED_EDGE('',*,*,#5600,.F.);
#8304=ORIENTED_EDGE('',*,*,#5551,.T.);
#8305=ORIENTED_EDGE('',*,*,#5549,.T.);
#8306=ORIENTED_EDGE('',*,*,#5560,.F.);
#8307=ORIENTED_EDGE('',*,*,#5601,.F.);
#8308=ORIENTED_EDGE('',*,*,#5548,.F.);
#8309=ORIENTED_EDGE('',*,*,#5602,.T.);
#8310=ORIENTED_EDGE('',*,*,#5598,.T.);
#8311=ORIENTED_EDGE('',*,*,#5561,.T.);
#8312=ORIENTED_EDGE('',*,*,#5602,.F.);
#8313=ORIENTED_EDGE('',*,*,#5547,.T.);
#8314=ORIENTED_EDGE('',*,*,#5603,.F.);
#8315=ORIENTED_EDGE('',*,*,#5604,.T.);
#8316=ORIENTED_EDGE('',*,*,#5603,.T.);
#8317=ORIENTED_EDGE('',*,*,#5604,.F.);
#8318=ORIENTED_EDGE('',*,*,#5605,.F.);
#8319=ORIENTED_EDGE('',*,*,#5606,.F.);
#8320=ORIENTED_EDGE('',*,*,#5606,.T.);
#8321=ORIENTED_EDGE('',*,*,#5607,.T.);
#8322=ORIENTED_EDGE('',*,*,#5608,.F.);
#8323=ORIENTED_EDGE('',*,*,#5607,.F.);
#8324=ORIENTED_EDGE('',*,*,#5609,.T.);
#8325=ORIENTED_EDGE('',*,*,#5608,.T.);
#8326=ORIENTED_EDGE('',*,*,#5609,.F.);
#8327=ORIENTED_EDGE('',*,*,#5610,.T.);
#8328=ORIENTED_EDGE('',*,*,#5605,.T.);
#8329=ORIENTED_EDGE('',*,*,#5610,.F.);
#8330=ORIENTED_EDGE('',*,*,#5611,.T.);
#8331=ORIENTED_EDGE('',*,*,#5612,.F.);
#8332=ORIENTED_EDGE('',*,*,#5611,.F.);
#8333=ORIENTED_EDGE('',*,*,#5613,.T.);
#8334=ORIENTED_EDGE('',*,*,#5614,.T.);
#8335=ORIENTED_EDGE('',*,*,#5613,.F.);
#8336=ORIENTED_EDGE('',*,*,#5614,.F.);
#8337=ORIENTED_EDGE('',*,*,#5615,.T.);
#8338=ORIENTED_EDGE('',*,*,#5615,.F.);
#8339=ORIENTED_EDGE('',*,*,#5616,.F.);
#8340=ORIENTED_EDGE('',*,*,#5617,.T.);
#8341=ORIENTED_EDGE('',*,*,#5612,.T.);
#8342=ORIENTED_EDGE('',*,*,#5617,.F.);
#8343=ORIENTED_EDGE('',*,*,#5618,.F.);
#8344=ORIENTED_EDGE('',*,*,#5616,.T.);
#8345=ORIENTED_EDGE('',*,*,#5619,.F.);
#8346=ORIENTED_EDGE('',*,*,#5619,.T.);
#8347=ORIENTED_EDGE('',*,*,#5618,.T.);
#8348=CYLINDRICAL_SURFACE('',#9277,2.25);
#8349=CYLINDRICAL_SURFACE('',#9279,2.25);
#8350=CYLINDRICAL_SURFACE('',#9280,2.25);
#8351=CYLINDRICAL_SURFACE('',#9281,2.25);
#8352=CYLINDRICAL_SURFACE('',#9282,2.25);
#8353=CYLINDRICAL_SURFACE('',#9284,2.25);
#8354=CYLINDRICAL_SURFACE('',#9289,1.25);
#8355=CYLINDRICAL_SURFACE('',#9294,1.25);
#8356=CYLINDRICAL_SURFACE('',#9297,3.5);
#8357=CYLINDRICAL_SURFACE('',#9408,3.5);
#8358=CYLINDRICAL_SURFACE('',#9507,4.2705);
#8359=CYLINDRICAL_SURFACE('',#9508,4.2705);
#8360=CYLINDRICAL_SURFACE('',#9509,4.2705);
#8361=CYLINDRICAL_SURFACE('',#9510,4.2705);
#8362=CYLINDRICAL_SURFACE('',#9511,4.2705);
#8363=CYLINDRICAL_SURFACE('',#9512,4.2705);
#8364=CYLINDRICAL_SURFACE('',#9513,4.2705);
#8365=CYLINDRICAL_SURFACE('',#9514,4.2705);
#8366=CYLINDRICAL_SURFACE('',#9515,4.2705);
#8367=CYLINDRICAL_SURFACE('',#9516,4.2705);
#8368=CYLINDRICAL_SURFACE('',#9517,4.2705);
#8369=CYLINDRICAL_SURFACE('',#9518,4.2705);
#8370=CYLINDRICAL_SURFACE('',#9519,4.2705);
#8371=CYLINDRICAL_SURFACE('',#9520,4.2705);
#8372=CYLINDRICAL_SURFACE('',#9521,4.2705);
#8373=CYLINDRICAL_SURFACE('',#9522,4.2705);
#8374=CYLINDRICAL_SURFACE('',#9523,6.);
#8375=CYLINDRICAL_SURFACE('',#9524,1.825);
#8376=CYLINDRICAL_SURFACE('',#9525,2.35);
#8377=CYLINDRICAL_SURFACE('',#9528,5.6245);
#8378=CYLINDRICAL_SURFACE('',#9529,5.6245);
#8379=CYLINDRICAL_SURFACE('',#9530,1.825);
#8380=CYLINDRICAL_SURFACE('',#9531,6.);
#8381=CYLINDRICAL_SURFACE('',#9532,6.);
#8382=CYLINDRICAL_SURFACE('',#9533,1.825);
#8383=CYLINDRICAL_SURFACE('',#9534,2.35);
#8384=CYLINDRICAL_SURFACE('',#9537,1.825);
#8385=CYLINDRICAL_SURFACE('',#9538,5.6245);
#8386=CYLINDRICAL_SURFACE('',#9539,5.6245);
#8387=CYLINDRICAL_SURFACE('',#9540,6.);
#8388=CYLINDRICAL_SURFACE('',#9541,6.);
#8389=CYLINDRICAL_SURFACE('',#9542,1.825);
#8390=CYLINDRICAL_SURFACE('',#9543,2.35);
#8391=CYLINDRICAL_SURFACE('',#9546,5.6245);
#8392=CYLINDRICAL_SURFACE('',#9547,5.6245);
#8393=CYLINDRICAL_SURFACE('',#9548,1.825);
#8394=CYLINDRICAL_SURFACE('',#9549,6.);
#8395=CYLINDRICAL_SURFACE('',#9550,6.);
#8396=CYLINDRICAL_SURFACE('',#9551,1.825);
#8397=CYLINDRICAL_SURFACE('',#9552,2.35);
#8398=CYLINDRICAL_SURFACE('',#9555,5.6245);
#8399=CYLINDRICAL_SURFACE('',#9556,5.6245);
#8400=CYLINDRICAL_SURFACE('',#9557,1.825);
#8401=CYLINDRICAL_SURFACE('',#9558,6.);
#8402=CYLINDRICAL_SURFACE('',#9559,6.);
#8403=CYLINDRICAL_SURFACE('',#9560,1.825);
#8404=CYLINDRICAL_SURFACE('',#9561,2.35);
#8405=CYLINDRICAL_SURFACE('',#9564,5.6245);
#8406=CYLINDRICAL_SURFACE('',#9565,5.6245);
#8407=CYLINDRICAL_SURFACE('',#9566,1.825);
#8408=CYLINDRICAL_SURFACE('',#9567,6.);
#8409=CYLINDRICAL_SURFACE('',#9568,6.);
#8410=CYLINDRICAL_SURFACE('',#9569,1.825);
#8411=CYLINDRICAL_SURFACE('',#9570,2.35);
#8412=CYLINDRICAL_SURFACE('',#9573,5.6245);
#8413=CYLINDRICAL_SURFACE('',#9574,5.6245);
#8414=CYLINDRICAL_SURFACE('',#9575,1.825);
#8415=CYLINDRICAL_SURFACE('',#9576,6.);
#8416=CYLINDRICAL_SURFACE('',#9577,6.);
#8417=CYLINDRICAL_SURFACE('',#9578,1.825);
#8418=CYLINDRICAL_SURFACE('',#9579,2.35);
#8419=CYLINDRICAL_SURFACE('',#9582,5.6245);
#8420=CYLINDRICAL_SURFACE('',#9583,5.6245);
#8421=CYLINDRICAL_SURFACE('',#9584,1.825);
#8422=CYLINDRICAL_SURFACE('',#9585,6.);
#8423=CYLINDRICAL_SURFACE('',#9586,6.);
#8424=CYLINDRICAL_SURFACE('',#9587,1.825);
#8425=CYLINDRICAL_SURFACE('',#9588,2.35);
#8426=CYLINDRICAL_SURFACE('',#9591,5.6245);
#8427=CYLINDRICAL_SURFACE('',#9592,5.6245);
#8428=CYLINDRICAL_SURFACE('',#9593,1.825);
#8429=CYLINDRICAL_SURFACE('',#9594,6.);
#8430=CYLINDRICAL_SURFACE('',#9595,6.);
#8431=CYLINDRICAL_SURFACE('',#9596,1.825);
#8432=CYLINDRICAL_SURFACE('',#9597,2.35);
#8433=CYLINDRICAL_SURFACE('',#9600,5.6245);
#8434=CYLINDRICAL_SURFACE('',#9601,5.6245);
#8435=CYLINDRICAL_SURFACE('',#9602,1.825);
#8436=CYLINDRICAL_SURFACE('',#9603,6.);
#8437=CYLINDRICAL_SURFACE('',#9604,6.);
#8438=CYLINDRICAL_SURFACE('',#9605,1.825);
#8439=CYLINDRICAL_SURFACE('',#9606,2.35);
#8440=CYLINDRICAL_SURFACE('',#9609,5.6245);
#8441=CYLINDRICAL_SURFACE('',#9610,5.6245);
#8442=CYLINDRICAL_SURFACE('',#9611,1.825);
#8443=CYLINDRICAL_SURFACE('',#9612,6.);
#8444=CYLINDRICAL_SURFACE('',#9613,6.);
#8445=CYLINDRICAL_SURFACE('',#9614,1.825);
#8446=CYLINDRICAL_SURFACE('',#9615,2.35);
#8447=CYLINDRICAL_SURFACE('',#9618,5.6245);
#8448=CYLINDRICAL_SURFACE('',#9619,5.6245);
#8449=CYLINDRICAL_SURFACE('',#9620,1.825);
#8450=CYLINDRICAL_SURFACE('',#9621,6.);
#8451=CYLINDRICAL_SURFACE('',#9622,6.);
#8452=CYLINDRICAL_SURFACE('',#9623,1.825);
#8453=CYLINDRICAL_SURFACE('',#9624,2.35);
#8454=CYLINDRICAL_SURFACE('',#9627,5.6245);
#8455=CYLINDRICAL_SURFACE('',#9628,5.6245);
#8456=CYLINDRICAL_SURFACE('',#9629,1.825);
#8457=CYLINDRICAL_SURFACE('',#9630,6.);
#8458=CYLINDRICAL_SURFACE('',#9631,6.);
#8459=CYLINDRICAL_SURFACE('',#9632,1.825);
#8460=CYLINDRICAL_SURFACE('',#9633,2.35);
#8461=CYLINDRICAL_SURFACE('',#9636,5.6245);
#8462=CYLINDRICAL_SURFACE('',#9637,5.6245);
#8463=CYLINDRICAL_SURFACE('',#9638,1.825);
#8464=CYLINDRICAL_SURFACE('',#9639,6.);
#8465=CYLINDRICAL_SURFACE('',#9640,6.);
#8466=CYLINDRICAL_SURFACE('',#9641,1.825);
#8467=CYLINDRICAL_SURFACE('',#9642,2.35);
#8468=CYLINDRICAL_SURFACE('',#9645,5.6245);
#8469=CYLINDRICAL_SURFACE('',#9646,5.6245);
#8470=CYLINDRICAL_SURFACE('',#9647,1.825);
#8471=CYLINDRICAL_SURFACE('',#9648,6.);
#8472=CYLINDRICAL_SURFACE('',#9649,6.);
#8473=CYLINDRICAL_SURFACE('',#9650,1.825);
#8474=CYLINDRICAL_SURFACE('',#9651,2.35);
#8475=CYLINDRICAL_SURFACE('',#9654,5.6245);
#8476=CYLINDRICAL_SURFACE('',#9655,5.6245);
#8477=CYLINDRICAL_SURFACE('',#9656,1.825);
#8478=CYLINDRICAL_SURFACE('',#9657,6.);
#8479=CYLINDRICAL_SURFACE('',#9658,6.);
#8480=CYLINDRICAL_SURFACE('',#9659,1.825);
#8481=CYLINDRICAL_SURFACE('',#9660,2.35);
#8482=CYLINDRICAL_SURFACE('',#9663,1.825);
#8483=CYLINDRICAL_SURFACE('',#9664,5.6245);
#8484=CYLINDRICAL_SURFACE('',#9665,5.6245);
#8485=CYLINDRICAL_SURFACE('',#9666,6.);
#8486=CYLINDRICAL_SURFACE('',#9670,3.);
#8487=CYLINDRICAL_SURFACE('',#9672,3.);
#8488=CYLINDRICAL_SURFACE('',#9679,0.9);
#8489=CYLINDRICAL_SURFACE('',#9688,1.5);
#8490=CYLINDRICAL_SURFACE('',#9692,1.5);
#8491=CYLINDRICAL_SURFACE('',#9698,1.6);
#8492=CYLINDRICAL_SURFACE('',#9709,1.116987298108);
#8493=CYLINDRICAL_SURFACE('',#9721,3.);
#8494=CYLINDRICAL_SURFACE('',#9732,0.25);
#8495=CYLINDRICAL_SURFACE('',#9756,0.25);
#8496=CYLINDRICAL_SURFACE('',#9758,0.25);
#8497=CYLINDRICAL_SURFACE('',#9760,0.25);
#8498=CYLINDRICAL_SURFACE('',#9762,0.25);
#8499=CYLINDRICAL_SURFACE('',#9763,0.25);
#8500=CYLINDRICAL_SURFACE('',#9765,0.25);
#8501=CYLINDRICAL_SURFACE('',#9767,0.25);
#8502=CYLINDRICAL_SURFACE('',#9769,0.25);
#8503=CYLINDRICAL_SURFACE('',#9771,0.25);
#8504=CYLINDRICAL_SURFACE('',#9773,0.25);
#8505=CYLINDRICAL_SURFACE('',#9775,0.25);
#8506=CYLINDRICAL_SURFACE('',#9780,1.);
#8507=CYLINDRICAL_SURFACE('',#9795,1.);
#8508=CYLINDRICAL_SURFACE('',#9816,3.8);
#8509=CYLINDRICAL_SURFACE('',#9818,3.8);
#8510=CYLINDRICAL_SURFACE('',#9820,3.8);
#8511=CYLINDRICAL_SURFACE('',#9822,3.8);
#8512=CYLINDRICAL_SURFACE('',#9840,1.);
#8513=CYLINDRICAL_SURFACE('',#9874,1.);
#8514=CYLINDRICAL_SURFACE('',#9888,1.);
#8515=CYLINDRICAL_SURFACE('',#9895,1.);
#8516=CYLINDRICAL_SURFACE('',#9898,11.8073463034);
#8517=CYLINDRICAL_SURFACE('',#9899,2.6);
#8518=CYLINDRICAL_SURFACE('',#9902,2.6);
#8519=CYLINDRICAL_SURFACE('',#9907,1.25);
#8520=CYLINDRICAL_SURFACE('',#9911,2.5);
#8521=CYLINDRICAL_SURFACE('',#9915,1.);
#8522=CYLINDRICAL_SURFACE('',#9920,1.);
#8523=CYLINDRICAL_SURFACE('',#9936,2.35);
#8524=CYLINDRICAL_SURFACE('',#9947,1.25);
#8525=CYLINDRICAL_SURFACE('',#9950,0.25);
#8526=CYLINDRICAL_SURFACE('',#9966,0.25);
#8527=CYLINDRICAL_SURFACE('',#9968,0.25);
#8528=CYLINDRICAL_SURFACE('',#9970,0.25);
#8529=CYLINDRICAL_SURFACE('',#9972,0.25);
#8530=CYLINDRICAL_SURFACE('',#9974,0.25);
#8531=CYLINDRICAL_SURFACE('',#9976,0.25);
#8532=CYLINDRICAL_SURFACE('',#9978,0.25);
#8533=CYLINDRICAL_SURFACE('',#9980,0.25);
#8534=CYLINDRICAL_SURFACE('',#9982,0.25);
#8535=CYLINDRICAL_SURFACE('',#9983,0.25);
#8536=CYLINDRICAL_SURFACE('',#9985,0.25);
#8537=CYLINDRICAL_SURFACE('',#9995,5.);
#8538=CYLINDRICAL_SURFACE('',#9999,4.);
#8539=CYLINDRICAL_SURFACE('',#10002,4.);
#8540=CYLINDRICAL_SURFACE('',#10008,6.);
#8541=CYLINDRICAL_SURFACE('',#10012,6.75);
#8542=CYLINDRICAL_SURFACE('',#10021,1.25);
#8543=CYLINDRICAL_SURFACE('',#10026,0.5);
#8544=CYLINDRICAL_SURFACE('',#10034,1.);
#8545=CYLINDRICAL_SURFACE('',#10039,0.5);
#8546=CYLINDRICAL_SURFACE('',#10042,0.5);
#8547=CYLINDRICAL_SURFACE('',#10046,3.);
#8548=CYLINDRICAL_SURFACE('',#10050,0.5);
#8549=CYLINDRICAL_SURFACE('',#10053,1.);
#8550=CYLINDRICAL_SURFACE('',#10060,8.);
#8551=CYLINDRICAL_SURFACE('',#10065,0.5);
#8552=CYLINDRICAL_SURFACE('',#10071,0.5);
#8553=CYLINDRICAL_SURFACE('',#10074,3.);
#8554=CYLINDRICAL_SURFACE('',#10081,1.);
#8555=CYLINDRICAL_SURFACE('',#10089,3.6);
#8556=CYLINDRICAL_SURFACE('',#10093,3.23);
#8557=CYLINDRICAL_SURFACE('',#10099,3.);
#8558=CYLINDRICAL_SURFACE('',#10102,1.);
#8559=CYLINDRICAL_SURFACE('',#10108,3.);
#8560=CYLINDRICAL_SURFACE('',#10109,3.);
#8561=CYLINDRICAL_SURFACE('',#10112,0.5);
#8562=CYLINDRICAL_SURFACE('',#10119,0.5);
#8563=CYLINDRICAL_SURFACE('',#10124,0.5);
#8564=CYLINDRICAL_SURFACE('',#10128,0.5);
#8565=CYLINDRICAL_SURFACE('',#10129,3.);
#8566=CYLINDRICAL_SURFACE('',#10130,0.5);
#8567=CYLINDRICAL_SURFACE('',#10131,0.5);
#8568=CYLINDRICAL_SURFACE('',#10136,4.);
#8569=CYLINDRICAL_SURFACE('',#10145,3.125);
#8570=CYLINDRICAL_SURFACE('',#10149,1.);
#8571=CYLINDRICAL_SURFACE('',#10158,4.);
#8572=CYLINDRICAL_SURFACE('',#10161,1.);
#8573=CYLINDRICAL_SURFACE('',#10163,1.);
#8574=CYLINDRICAL_SURFACE('',#10165,1.);
#8575=CYLINDRICAL_SURFACE('',#10167,1.);
#8576=CYLINDRICAL_SURFACE('',#10169,1.);
#8577=CYLINDRICAL_SURFACE('',#10179,2.5);
#8578=CYLINDRICAL_SURFACE('',#10183,3.8);
#8579=CYLINDRICAL_SURFACE('',#10188,6.65);
#8580=CYLINDRICAL_SURFACE('',#10192,5.65);
#8581=ADVANCED_FACE('',(#518),#8348,.T.);
#8582=ADVANCED_FACE('',(#519),#8349,.T.);
#8583=ADVANCED_FACE('',(#520),#8350,.T.);
#8584=ADVANCED_FACE('',(#521),#8351,.T.);
#8585=ADVANCED_FACE('',(#522),#8352,.T.);
#8586=ADVANCED_FACE('',(#523),#409,.F.);
#8587=ADVANCED_FACE('',(#524),#8353,.T.);
#8588=ADVANCED_FACE('',(#525),#323,.T.);
#8589=ADVANCED_FACE('',(#526),#324,.T.);
#8590=ADVANCED_FACE('',(#527),#410,.T.);
#8591=ADVANCED_FACE('',(#528),#325,.T.);
#8592=ADVANCED_FACE('',(#529),#326,.T.);
#8593=ADVANCED_FACE('',(#530),#327,.T.);
#8594=ADVANCED_FACE('',(#531),#328,.T.);
#8595=ADVANCED_FACE('',(#532),#329,.T.);
#8596=ADVANCED_FACE('',(#533),#330,.T.);
#8597=ADVANCED_FACE('',(#534,#288),#411,.T.);
#8598=ADVANCED_FACE('',(#535),#8354,.F.);
#8599=ADVANCED_FACE('',(#536),#412,.F.);
#8600=ADVANCED_FACE('',(#537),#331,.T.);
#8601=ADVANCED_FACE('',(#538),#332,.T.);
#8602=ADVANCED_FACE('',(#539),#333,.T.);
#8603=ADVANCED_FACE('',(#540),#334,.T.);
#8604=ADVANCED_FACE('',(#541),#335,.T.);
#8605=ADVANCED_FACE('',(#542),#336,.T.);
#8606=ADVANCED_FACE('',(#543),#337,.T.);
#8607=ADVANCED_FACE('',(#544),#338,.T.);
#8608=ADVANCED_FACE('',(#545),#339,.T.);
#8609=ADVANCED_FACE('',(#546),#340,.T.);
#8610=ADVANCED_FACE('',(#547),#413,.T.);
#8611=ADVANCED_FACE('',(#548),#414,.T.);
#8612=ADVANCED_FACE('',(#549),#8355,.F.);
#8613=ADVANCED_FACE('',(#550),#341,.T.);
#8614=ADVANCED_FACE('',(#551),#342,.T.);
#8615=ADVANCED_FACE('',(#552,#289),#415,.F.);
#8616=ADVANCED_FACE('',(#553),#8356,.T.);
#8617=ADVANCED_FACE('',(#554),#284,.T.);
#8618=ADVANCED_FACE('',(#555,#290),#416,.F.);
#8619=ADVANCED_FACE('',(#556),#417,.F.);
#8620=ADVANCED_FACE('',(#557),#418,.F.);
#8621=ADVANCED_FACE('',(#558),#419,.F.);
#8622=ADVANCED_FACE('',(#559),#420,.F.);
#8623=ADVANCED_FACE('',(#560),#421,.F.);
#8624=ADVANCED_FACE('',(#561),#422,.F.);
#8625=ADVANCED_FACE('',(#562,#291),#423,.T.);
#8626=ADVANCED_FACE('',(#563),#8357,.F.);
#8627=ADVANCED_FACE('',(#564,#292),#424,.T.);
#8628=ADVANCED_FACE('',(#565),#8358,.T.);
#8629=ADVANCED_FACE('',(#566),#8359,.T.);
#8630=ADVANCED_FACE('',(#567),#8360,.T.);
#8631=ADVANCED_FACE('',(#568),#8361,.T.);
#8632=ADVANCED_FACE('',(#569),#8362,.T.);
#8633=ADVANCED_FACE('',(#570),#8363,.T.);
#8634=ADVANCED_FACE('',(#571),#8364,.T.);
#8635=ADVANCED_FACE('',(#572),#8365,.T.);
#8636=ADVANCED_FACE('',(#573),#8366,.T.);
#8637=ADVANCED_FACE('',(#574),#8367,.T.);
#8638=ADVANCED_FACE('',(#575),#8368,.T.);
#8639=ADVANCED_FACE('',(#576),#8369,.T.);
#8640=ADVANCED_FACE('',(#577),#8370,.T.);
#8641=ADVANCED_FACE('',(#578),#8371,.T.);
#8642=ADVANCED_FACE('',(#579),#8372,.T.);
#8643=ADVANCED_FACE('',(#580),#8373,.T.);
#8644=ADVANCED_FACE('',(#581),#8374,.T.);
#8645=ADVANCED_FACE('',(#582),#8375,.T.);
#8646=ADVANCED_FACE('',(#583),#8376,.F.);
#8647=ADVANCED_FACE('',(#584),#8377,.T.);
#8648=ADVANCED_FACE('',(#585),#8378,.T.);
#8649=ADVANCED_FACE('',(#586),#8379,.T.);
#8650=ADVANCED_FACE('',(#587),#8380,.T.);
#8651=ADVANCED_FACE('',(#588),#8381,.T.);
#8652=ADVANCED_FACE('',(#589),#8382,.T.);
#8653=ADVANCED_FACE('',(#590),#8383,.F.);
#8654=ADVANCED_FACE('',(#591),#8384,.T.);
#8655=ADVANCED_FACE('',(#592),#8385,.T.);
#8656=ADVANCED_FACE('',(#593),#8386,.T.);
#8657=ADVANCED_FACE('',(#594),#8387,.T.);
#8658=ADVANCED_FACE('',(#595),#8388,.T.);
#8659=ADVANCED_FACE('',(#596),#8389,.T.);
#8660=ADVANCED_FACE('',(#597),#8390,.F.);
#8661=ADVANCED_FACE('',(#598),#8391,.T.);
#8662=ADVANCED_FACE('',(#599),#8392,.T.);
#8663=ADVANCED_FACE('',(#600),#8393,.T.);
#8664=ADVANCED_FACE('',(#601),#8394,.T.);
#8665=ADVANCED_FACE('',(#602),#8395,.T.);
#8666=ADVANCED_FACE('',(#603),#8396,.T.);
#8667=ADVANCED_FACE('',(#604),#8397,.F.);
#8668=ADVANCED_FACE('',(#605),#8398,.T.);
#8669=ADVANCED_FACE('',(#606),#8399,.T.);
#8670=ADVANCED_FACE('',(#607),#8400,.T.);
#8671=ADVANCED_FACE('',(#608),#8401,.T.);
#8672=ADVANCED_FACE('',(#609),#8402,.T.);
#8673=ADVANCED_FACE('',(#610),#8403,.T.);
#8674=ADVANCED_FACE('',(#611),#8404,.F.);
#8675=ADVANCED_FACE('',(#612),#8405,.T.);
#8676=ADVANCED_FACE('',(#613),#8406,.T.);
#8677=ADVANCED_FACE('',(#614),#8407,.T.);
#8678=ADVANCED_FACE('',(#615),#8408,.T.);
#8679=ADVANCED_FACE('',(#616),#8409,.T.);
#8680=ADVANCED_FACE('',(#617),#8410,.T.);
#8681=ADVANCED_FACE('',(#618),#8411,.F.);
#8682=ADVANCED_FACE('',(#619),#8412,.T.);
#8683=ADVANCED_FACE('',(#620),#8413,.T.);
#8684=ADVANCED_FACE('',(#621),#8414,.T.);
#8685=ADVANCED_FACE('',(#622),#8415,.T.);
#8686=ADVANCED_FACE('',(#623),#8416,.T.);
#8687=ADVANCED_FACE('',(#624),#8417,.T.);
#8688=ADVANCED_FACE('',(#625),#8418,.F.);
#8689=ADVANCED_FACE('',(#626),#8419,.T.);
#8690=ADVANCED_FACE('',(#627),#8420,.T.);
#8691=ADVANCED_FACE('',(#628),#8421,.T.);
#8692=ADVANCED_FACE('',(#629),#8422,.T.);
#8693=ADVANCED_FACE('',(#630),#8423,.T.);
#8694=ADVANCED_FACE('',(#631),#8424,.T.);
#8695=ADVANCED_FACE('',(#632),#8425,.F.);
#8696=ADVANCED_FACE('',(#633),#8426,.T.);
#8697=ADVANCED_FACE('',(#634),#8427,.T.);
#8698=ADVANCED_FACE('',(#635),#8428,.T.);
#8699=ADVANCED_FACE('',(#636),#8429,.T.);
#8700=ADVANCED_FACE('',(#637),#8430,.T.);
#8701=ADVANCED_FACE('',(#638),#8431,.T.);
#8702=ADVANCED_FACE('',(#639),#8432,.F.);
#8703=ADVANCED_FACE('',(#640),#8433,.T.);
#8704=ADVANCED_FACE('',(#641),#8434,.T.);
#8705=ADVANCED_FACE('',(#642),#8435,.T.);
#8706=ADVANCED_FACE('',(#643),#8436,.T.);
#8707=ADVANCED_FACE('',(#644),#8437,.T.);
#8708=ADVANCED_FACE('',(#645),#8438,.T.);
#8709=ADVANCED_FACE('',(#646),#8439,.F.);
#8710=ADVANCED_FACE('',(#647),#8440,.T.);
#8711=ADVANCED_FACE('',(#648),#8441,.T.);
#8712=ADVANCED_FACE('',(#649),#8442,.T.);
#8713=ADVANCED_FACE('',(#650),#8443,.T.);
#8714=ADVANCED_FACE('',(#651),#8444,.T.);
#8715=ADVANCED_FACE('',(#652),#8445,.T.);
#8716=ADVANCED_FACE('',(#653),#8446,.F.);
#8717=ADVANCED_FACE('',(#654),#8447,.T.);
#8718=ADVANCED_FACE('',(#655),#8448,.T.);
#8719=ADVANCED_FACE('',(#656),#8449,.T.);
#8720=ADVANCED_FACE('',(#657),#8450,.T.);
#8721=ADVANCED_FACE('',(#658),#8451,.T.);
#8722=ADVANCED_FACE('',(#659),#8452,.T.);
#8723=ADVANCED_FACE('',(#660),#8453,.F.);
#8724=ADVANCED_FACE('',(#661),#8454,.T.);
#8725=ADVANCED_FACE('',(#662),#8455,.T.);
#8726=ADVANCED_FACE('',(#663),#8456,.T.);
#8727=ADVANCED_FACE('',(#664),#8457,.T.);
#8728=ADVANCED_FACE('',(#665),#8458,.T.);
#8729=ADVANCED_FACE('',(#666),#8459,.T.);
#8730=ADVANCED_FACE('',(#667),#8460,.F.);
#8731=ADVANCED_FACE('',(#668),#8461,.T.);
#8732=ADVANCED_FACE('',(#669),#8462,.T.);
#8733=ADVANCED_FACE('',(#670),#8463,.T.);
#8734=ADVANCED_FACE('',(#671),#8464,.T.);
#8735=ADVANCED_FACE('',(#672),#8465,.T.);
#8736=ADVANCED_FACE('',(#673),#8466,.T.);
#8737=ADVANCED_FACE('',(#674),#8467,.F.);
#8738=ADVANCED_FACE('',(#675),#8468,.T.);
#8739=ADVANCED_FACE('',(#676),#8469,.T.);
#8740=ADVANCED_FACE('',(#677),#8470,.T.);
#8741=ADVANCED_FACE('',(#678),#8471,.T.);
#8742=ADVANCED_FACE('',(#679),#8472,.T.);
#8743=ADVANCED_FACE('',(#680),#8473,.T.);
#8744=ADVANCED_FACE('',(#681),#8474,.F.);
#8745=ADVANCED_FACE('',(#682),#8475,.T.);
#8746=ADVANCED_FACE('',(#683),#8476,.T.);
#8747=ADVANCED_FACE('',(#684),#8477,.T.);
#8748=ADVANCED_FACE('',(#685),#8478,.T.);
#8749=ADVANCED_FACE('',(#686),#8479,.T.);
#8750=ADVANCED_FACE('',(#687),#8480,.T.);
#8751=ADVANCED_FACE('',(#688),#8481,.F.);
#8752=ADVANCED_FACE('',(#689),#8482,.T.);
#8753=ADVANCED_FACE('',(#690),#8483,.T.);
#8754=ADVANCED_FACE('',(#691),#8484,.T.);
#8755=ADVANCED_FACE('',(#692),#8485,.T.);
#8756=ADVANCED_FACE('',(#693,#293),#425,.T.);
#8757=ADVANCED_FACE('',(#694),#8486,.T.);
#8758=ADVANCED_FACE('',(#695),#8487,.T.);
#8759=ADVANCED_FACE('',(#696,#294,#295),#207,.F.);
#8760=ADVANCED_FACE('',(#697),#285,.T.);
#8761=ADVANCED_FACE('',(#698),#8488,.F.);
#8762=ADVANCED_FACE('',(#699),#426,.T.);
#8763=ADVANCED_FACE('',(#700),#427,.T.);
#8764=ADVANCED_FACE('',(#701),#428,.T.);
#8765=ADVANCED_FACE('',(#702),#429,.T.);
#8766=ADVANCED_FACE('',(#703),#430,.T.);
#8767=ADVANCED_FACE('',(#704),#431,.T.);
#8768=ADVANCED_FACE('',(#705,#296),#432,.T.);
#8769=ADVANCED_FACE('',(#706),#8489,.F.);
#8770=ADVANCED_FACE('',(#707),#343,.T.);
#8771=ADVANCED_FACE('',(#708),#344,.T.);
#8772=ADVANCED_FACE('',(#709),#345,.T.);
#8773=ADVANCED_FACE('',(#710),#346,.T.);
#8774=ADVANCED_FACE('',(#711),#347,.T.);
#8775=ADVANCED_FACE('',(#712),#348,.T.);
#8776=ADVANCED_FACE('',(#713),#349,.T.);
#8777=ADVANCED_FACE('',(#714),#433,.F.);
#8778=ADVANCED_FACE('',(#715),#434,.T.);
#8779=ADVANCED_FACE('',(#716),#350,.T.);
#8780=ADVANCED_FACE('',(#717),#8490,.F.);
#8781=ADVANCED_FACE('',(#718),#351,.T.);
#8782=ADVANCED_FACE('',(#719),#352,.T.);
#8783=ADVANCED_FACE('',(#720),#353,.T.);
#8784=ADVANCED_FACE('',(#721),#354,.T.);
#8785=ADVANCED_FACE('',(#722),#355,.T.);
#8786=ADVANCED_FACE('',(#723),#356,.T.);
#8787=ADVANCED_FACE('',(#724),#357,.T.);
#8788=ADVANCED_FACE('',(#725),#435,.T.);
#8789=ADVANCED_FACE('',(#726,#297),#436,.F.);
#8790=ADVANCED_FACE('',(#727),#8491,.F.);
#8791=ADVANCED_FACE('',(#728,#298),#437,.T.);
#8792=ADVANCED_FACE('',(#729),#208,.T.);
#8793=ADVANCED_FACE('',(#730),#199,.T.);
#8794=ADVANCED_FACE('',(#731),#438,.T.);
#8795=ADVANCED_FACE('',(#732),#8492,.T.);
#8796=ADVANCED_FACE('',(#733),#358,.F.);
#8797=ADVANCED_FACE('',(#734),#359,.F.);
#8798=ADVANCED_FACE('',(#735),#200,.T.);
#8799=ADVANCED_FACE('',(#736),#360,.F.);
#8800=ADVANCED_FACE('',(#737),#361,.F.);
#8801=ADVANCED_FACE('',(#738),#362,.F.);
#8802=ADVANCED_FACE('',(#739),#363,.F.);
#8803=ADVANCED_FACE('',(#740),#364,.F.);
#8804=ADVANCED_FACE('',(#741),#365,.F.);
#8805=ADVANCED_FACE('',(#742),#366,.F.);
#8806=ADVANCED_FACE('',(#743),#367,.F.);
#8807=ADVANCED_FACE('',(#744),#368,.F.);
#8808=ADVANCED_FACE('',(#745),#209,.F.);
#8809=ADVANCED_FACE('',(#746),#201,.T.);
#8810=ADVANCED_FACE('',(#747),#439,.F.);
#8811=ADVANCED_FACE('',(#748),#369,.F.);
#8812=ADVANCED_FACE('',(#749,#299),#440,.T.);
#8813=ADVANCED_FACE('',(#750),#8493,.T.);
#8814=ADVANCED_FACE('',(#751),#127,.F.);
#8815=ADVANCED_FACE('',(#752),#441,.F.);
#8816=ADVANCED_FACE('',(#753),#8494,.F.);
#8817=ADVANCED_FACE('',(#754),#442,.T.);
#8818=ADVANCED_FACE('',(#755),#443,.F.);
#8819=ADVANCED_FACE('',(#756),#444,.F.);
#8820=ADVANCED_FACE('',(#757),#445,.F.);
#8821=ADVANCED_FACE('',(#758),#446,.F.);
#8822=ADVANCED_FACE('',(#759),#447,.F.);
#8823=ADVANCED_FACE('',(#760),#448,.F.);
#8824=ADVANCED_FACE('',(#761),#8495,.F.);
#8825=ADVANCED_FACE('',(#762),#449,.F.);
#8826=ADVANCED_FACE('',(#763),#8496,.F.);
#8827=ADVANCED_FACE('',(#764),#450,.F.);
#8828=ADVANCED_FACE('',(#765),#8497,.F.);
#8829=ADVANCED_FACE('',(#766),#451,.F.);
#8830=ADVANCED_FACE('',(#767),#8498,.T.);
#8831=ADVANCED_FACE('',(#768),#8499,.F.);
#8832=ADVANCED_FACE('',(#769),#452,.F.);
#8833=ADVANCED_FACE('',(#770),#8500,.T.);
#8834=ADVANCED_FACE('',(#771),#453,.F.);
#8835=ADVANCED_FACE('',(#772),#8501,.F.);
#8836=ADVANCED_FACE('',(#773),#454,.F.);
#8837=ADVANCED_FACE('',(#774),#8502,.F.);
#8838=ADVANCED_FACE('',(#775),#455,.F.);
#8839=ADVANCED_FACE('',(#776),#8503,.T.);
#8840=ADVANCED_FACE('',(#777),#456,.F.);
#8841=ADVANCED_FACE('',(#778),#8504,.T.);
#8842=ADVANCED_FACE('',(#779),#457,.F.);
#8843=ADVANCED_FACE('',(#780),#8505,.F.);
#8844=ADVANCED_FACE('',(#781),#458,.T.);
#8845=ADVANCED_FACE('',(#782),#8506,.T.);
#8846=ADVANCED_FACE('',(#783),#459,.T.);
#8847=ADVANCED_FACE('',(#784),#460,.T.);
#8848=ADVANCED_FACE('',(#785),#461,.T.);
#8849=ADVANCED_FACE('',(#786),#462,.T.);
#8850=ADVANCED_FACE('',(#787),#8507,.T.);
#8851=ADVANCED_FACE('',(#788),#128,.T.);
#8852=ADVANCED_FACE('',(#789),#210,.F.);
#8853=ADVANCED_FACE('',(#790),#129,.F.);
#8854=ADVANCED_FACE('',(#791),#211,.T.);
#8855=ADVANCED_FACE('',(#792),#130,.T.);
#8856=ADVANCED_FACE('',(#793),#131,.T.);
#8857=ADVANCED_FACE('',(#794),#463,.T.);
#8858=ADVANCED_FACE('',(#795),#132,.T.);
#8859=ADVANCED_FACE('',(#796),#133,.F.);
#8860=ADVANCED_FACE('',(#797),#8508,.T.);
#8861=ADVANCED_FACE('',(#798),#8509,.T.);
#8862=ADVANCED_FACE('',(#799),#8510,.T.);
#8863=ADVANCED_FACE('',(#800),#8511,.T.);
#8864=ADVANCED_FACE('',(#801),#134,.F.);
#8865=ADVANCED_FACE('',(#802),#135,.T.);
#8866=ADVANCED_FACE('',(#803),#136,.T.);
#8867=ADVANCED_FACE('',(#804),#137,.T.);
#8868=ADVANCED_FACE('',(#805),#138,.F.);
#8869=ADVANCED_FACE('',(#806),#139,.F.);
#8870=ADVANCED_FACE('',(#807),#212,.T.);
#8871=ADVANCED_FACE('',(#808),#140,.T.);
#8872=ADVANCED_FACE('',(#809),#141,.T.);
#8873=ADVANCED_FACE('',(#810),#142,.T.);
#8874=ADVANCED_FACE('',(#811),#8512,.T.);
#8875=ADVANCED_FACE('',(#812),#143,.T.);
#8876=ADVANCED_FACE('',(#813),#144,.T.);
#8877=ADVANCED_FACE('',(#814),#145,.T.);
#8878=ADVANCED_FACE('',(#815),#213,.T.);
#8879=ADVANCED_FACE('',(#816),#146,.F.);
#8880=ADVANCED_FACE('',(#817),#214,.F.);
#8881=ADVANCED_FACE('',(#818),#147,.T.);
#8882=ADVANCED_FACE('',(#819),#148,.T.);
#8883=ADVANCED_FACE('',(#820),#149,.F.);
#8884=ADVANCED_FACE('',(#821),#150,.F.);
#8885=ADVANCED_FACE('',(#822),#151,.F.);
#8886=ADVANCED_FACE('',(#823),#152,.F.);
#8887=ADVANCED_FACE('',(#824),#153,.T.);
#8888=ADVANCED_FACE('',(#825),#154,.T.);
#8889=ADVANCED_FACE('',(#826),#215,.F.);
#8890=ADVANCED_FACE('',(#827),#216,.T.);
#8891=ADVANCED_FACE('',(#828),#217,.F.);
#8892=ADVANCED_FACE('',(#829),#155,.T.);
#8893=ADVANCED_FACE('',(#830),#8513,.T.);
#8894=ADVANCED_FACE('',(#831),#156,.T.);
#8895=ADVANCED_FACE('',(#832),#218,.T.);
#8896=ADVANCED_FACE('',(#833),#157,.F.);
#8897=ADVANCED_FACE('',(#834),#202,.T.);
#8898=ADVANCED_FACE('',(#835),#158,.T.);
#8899=ADVANCED_FACE('',(#836),#464,.T.);
#8900=ADVANCED_FACE('',(#837),#159,.T.);
#8901=ADVANCED_FACE('',(#838),#203,.T.);
#8902=ADVANCED_FACE('',(#839),#160,.T.);
#8903=ADVANCED_FACE('',(#840),#8514,.T.);
#8904=ADVANCED_FACE('',(#841),#161,.T.);
#8905=ADVANCED_FACE('',(#842),#162,.T.);
#8906=ADVANCED_FACE('',(#843),#163,.T.);
#8907=ADVANCED_FACE('',(#844),#465,.T.);
#8908=ADVANCED_FACE('',(#845),#164,.T.);
#8909=ADVANCED_FACE('',(#846),#165,.T.);
#8910=ADVANCED_FACE('',(#847),#8515,.T.);
#8911=ADVANCED_FACE('',(#848),#166,.T.);
#8912=ADVANCED_FACE('',(#849),#167,.T.);
#8913=ADVANCED_FACE('',(#850,#300),#8516,.T.);
#8914=ADVANCED_FACE('',(#851),#8517,.F.);
#8915=ADVANCED_FACE('',(#852),#8518,.F.);
#8916=ADVANCED_FACE('',(#853),#204,.F.);
#8917=ADVANCED_FACE('',(#854),#8519,.F.);
#8918=ADVANCED_FACE('',(#855,#301),#466,.T.);
#8919=ADVANCED_FACE('',(#856),#8520,.F.);
#8920=ADVANCED_FACE('',(#857,#302),#467,.T.);
#8921=ADVANCED_FACE('',(#858),#168,.T.);
#8922=ADVANCED_FACE('',(#859),#169,.T.);
#8923=ADVANCED_FACE('',(#860),#8521,.T.);
#8924=ADVANCED_FACE('',(#861),#170,.T.);
#8925=ADVANCED_FACE('',(#862),#171,.T.);
#8926=ADVANCED_FACE('',(#863),#172,.F.);
#8927=ADVANCED_FACE('',(#864),#173,.T.);
#8928=ADVANCED_FACE('',(#865),#174,.T.);
#8929=ADVANCED_FACE('',(#866),#175,.F.);
#8930=ADVANCED_FACE('',(#867),#176,.T.);
#8931=ADVANCED_FACE('',(#868),#177,.F.);
#8932=ADVANCED_FACE('',(#869),#178,.F.);
#8933=ADVANCED_FACE('',(#870),#179,.F.);
#8934=ADVANCED_FACE('',(#871),#8522,.T.);
#8935=ADVANCED_FACE('',(#872,#303),#468,.T.);
#8936=ADVANCED_FACE('',(#873),#8523,.T.);
#8937=ADVANCED_FACE('',(#874),#205,.T.);
#8938=ADVANCED_FACE('',(#875),#219,.F.);
#8939=ADVANCED_FACE('',(#876),#206,.T.);
#8940=ADVANCED_FACE('',(#877),#8524,.T.);
#8941=ADVANCED_FACE('',(#878),#370,.F.);
#8942=ADVANCED_FACE('',(#879),#371,.F.);
#8943=ADVANCED_FACE('',(#880),#372,.F.);
#8944=ADVANCED_FACE('',(#881),#373,.F.);
#8945=ADVANCED_FACE('',(#882),#374,.F.);
#8946=ADVANCED_FACE('',(#883),#375,.F.);
#8947=ADVANCED_FACE('',(#884),#376,.F.);
#8948=ADVANCED_FACE('',(#885),#377,.F.);
#8949=ADVANCED_FACE('',(#886),#378,.F.);
#8950=ADVANCED_FACE('',(#887),#379,.F.);
#8951=ADVANCED_FACE('',(#888),#380,.F.);
#8952=ADVANCED_FACE('',(#889),#381,.F.);
#8953=ADVANCED_FACE('',(#890),#469,.F.);
#8954=ADVANCED_FACE('',(#891),#382,.F.);
#8955=ADVANCED_FACE('',(#892),#383,.F.);
#8956=ADVANCED_FACE('',(#893),#384,.F.);
#8957=ADVANCED_FACE('',(#894),#385,.F.);
#8958=ADVANCED_FACE('',(#895),#386,.F.);
#8959=ADVANCED_FACE('',(#896),#387,.F.);
#8960=ADVANCED_FACE('',(#897),#470,.F.);
#8961=ADVANCED_FACE('',(#898),#8525,.T.);
#8962=ADVANCED_FACE('',(#899),#471,.F.);
#8963=ADVANCED_FACE('',(#900),#472,.T.);
#8964=ADVANCED_FACE('',(#901),#473,.F.);
#8965=ADVANCED_FACE('',(#902),#8526,.T.);
#8966=ADVANCED_FACE('',(#903),#474,.F.);
#8967=ADVANCED_FACE('',(#904),#8527,.F.);
#8968=ADVANCED_FACE('',(#905),#475,.F.);
#8969=ADVANCED_FACE('',(#906),#8528,.F.);
#8970=ADVANCED_FACE('',(#907),#476,.F.);
#8971=ADVANCED_FACE('',(#908),#8529,.T.);
#8972=ADVANCED_FACE('',(#909),#477,.F.);
#8973=ADVANCED_FACE('',(#910),#8530,.F.);
#8974=ADVANCED_FACE('',(#911),#478,.F.);
#8975=ADVANCED_FACE('',(#912),#8531,.F.);
#8976=ADVANCED_FACE('',(#913),#479,.F.);
#8977=ADVANCED_FACE('',(#914),#8532,.T.);
#8978=ADVANCED_FACE('',(#915),#480,.F.);
#8979=ADVANCED_FACE('',(#916),#8533,.F.);
#8980=ADVANCED_FACE('',(#917),#481,.F.);
#8981=ADVANCED_FACE('',(#918),#8534,.F.);
#8982=ADVANCED_FACE('',(#919),#8535,.F.);
#8983=ADVANCED_FACE('',(#920),#482,.F.);
#8984=ADVANCED_FACE('',(#921),#8536,.F.);
#8985=ADVANCED_FACE('',(#922),#483,.F.);
#8986=ADVANCED_FACE('',(#923,#304),#484,.F.);
#8987=ADVANCED_FACE('',(#924),#220,.F.);
#8988=ADVANCED_FACE('',(#925),#8537,.T.);
#8989=ADVANCED_FACE('',(#926,#305),#485,.T.);
#8990=ADVANCED_FACE('',(#927),#8538,.F.);
#8991=ADVANCED_FACE('',(#928),#8539,.F.);
#8992=ADVANCED_FACE('',(#929),#486,.T.);
#8993=ADVANCED_FACE('',(#930),#388,.T.);
#8994=ADVANCED_FACE('',(#931),#389,.T.);
#8995=ADVANCED_FACE('',(#932),#390,.T.);
#8996=ADVANCED_FACE('',(#933),#391,.T.);
#8997=ADVANCED_FACE('',(#934),#392,.T.);
#8998=ADVANCED_FACE('',(#935),#393,.T.);
#8999=ADVANCED_FACE('',(#936),#394,.T.);
#9000=ADVANCED_FACE('',(#937),#395,.T.);
#9001=ADVANCED_FACE('',(#938),#396,.T.);
#9002=ADVANCED_FACE('',(#939),#397,.T.);
#9003=ADVANCED_FACE('',(#940),#398,.T.);
#9004=ADVANCED_FACE('',(#941),#399,.T.);
#9005=ADVANCED_FACE('',(#942),#487,.T.);
#9006=ADVANCED_FACE('',(#943,#306),#488,.T.);
#9007=ADVANCED_FACE('',(#944,#307),#8540,.F.);
#9008=ADVANCED_FACE('',(#945,#308),#489,.T.);
#9009=ADVANCED_FACE('',(#946),#8541,.F.);
#9010=ADVANCED_FACE('',(#947,#309,#310),#490,.T.);
#9011=ADVANCED_FACE('',(#948),#8542,.F.);
#9012=ADVANCED_FACE('',(#949,#311),#491,.F.);
#9013=ADVANCED_FACE('',(#950),#8543,.T.);
#9014=ADVANCED_FACE('',(#951),#180,.F.);
#9015=ADVANCED_FACE('',(#952),#221,.F.);
#9016=ADVANCED_FACE('',(#953),#181,.F.);
#9017=ADVANCED_FACE('',(#954),#8544,.F.);
#9018=ADVANCED_FACE('',(#955),#222,.T.);
#9019=ADVANCED_FACE('',(#956),#8545,.T.);
#9020=ADVANCED_FACE('',(#957),#492,.T.);
#9021=ADVANCED_FACE('',(#958),#8546,.T.);
#9022=ADVANCED_FACE('',(#959),#223,.T.);
#9023=ADVANCED_FACE('',(#960),#8547,.T.);
#9024=ADVANCED_FACE('',(#961),#224,.T.);
#9025=ADVANCED_FACE('',(#962),#8548,.T.);
#9026=ADVANCED_FACE('',(#963),#493,.T.);
#9027=ADVANCED_FACE('',(#964),#8549,.F.);
#9028=ADVANCED_FACE('',(#965),#225,.T.);
#9029=ADVANCED_FACE('',(#966),#226,.T.);
#9030=ADVANCED_FACE('',(#967),#8550,.T.);
#9031=ADVANCED_FACE('',(#968),#227,.T.);
#9032=ADVANCED_FACE('',(#969),#8551,.T.);
#9033=ADVANCED_FACE('',(#970),#494,.T.);
#9034=ADVANCED_FACE('',(#971),#182,.F.);
#9035=ADVANCED_FACE('',(#972),#183,.T.);
#9036=ADVANCED_FACE('',(#973),#8552,.T.);
#9037=ADVANCED_FACE('',(#974),#184,.T.);
#9038=ADVANCED_FACE('',(#975),#8553,.T.);
#9039=ADVANCED_FACE('',(#976),#185,.F.);
#9040=ADVANCED_FACE('',(#977),#186,.T.);
#9041=ADVANCED_FACE('',(#978),#187,.T.);
#9042=ADVANCED_FACE('',(#979),#188,.F.);
#9043=ADVANCED_FACE('',(#980),#189,.T.);
#9044=ADVANCED_FACE('',(#981),#8554,.T.);
#9045=ADVANCED_FACE('',(#982),#190,.F.);
#9046=ADVANCED_FACE('',(#983,#312),#495,.T.);
#9047=ADVANCED_FACE('',(#984),#8555,.F.);
#9048=ADVANCED_FACE('',(#985,#313),#496,.T.);
#9049=ADVANCED_FACE('',(#986),#8556,.F.);
#9050=ADVANCED_FACE('',(#987,#314),#497,.T.);
#9051=ADVANCED_FACE('',(#988),#8557,.T.);
#9052=ADVANCED_FACE('',(#989),#498,.F.);
#9053=ADVANCED_FACE('',(#990),#499,.F.);
#9054=ADVANCED_FACE('',(#991),#8558,.F.);
#9055=ADVANCED_FACE('',(#992),#191,.F.);
#9056=ADVANCED_FACE('',(#993),#192,.T.);
#9057=ADVANCED_FACE('',(#994),#500,.F.);
#9058=ADVANCED_FACE('',(#995),#8559,.T.);
#9059=ADVANCED_FACE('',(#996),#8560,.T.);
#9060=ADVANCED_FACE('',(#997),#193,.T.);
#9061=ADVANCED_FACE('',(#998),#8561,.T.);
#9062=ADVANCED_FACE('',(#999),#501,.F.);
#9063=ADVANCED_FACE('',(#1000),#194,.T.);
#9064=ADVANCED_FACE('',(#1001),#195,.T.);
#9065=ADVANCED_FACE('',(#1002),#196,.F.);
#9066=ADVANCED_FACE('',(#1003),#197,.T.);
#9067=ADVANCED_FACE('',(#1004),#502,.T.);
#9068=ADVANCED_FACE('',(#1005),#8562,.T.);
#9069=ADVANCED_FACE('',(#1006),#228,.T.);
#9070=ADVANCED_FACE('',(#1007),#8563,.T.);
#9071=ADVANCED_FACE('',(#1008),#229,.T.);
#9072=ADVANCED_FACE('',(#1009),#8564,.T.);
#9073=ADVANCED_FACE('',(#1010),#8565,.T.);
#9074=ADVANCED_FACE('',(#1011),#8566,.T.);
#9075=ADVANCED_FACE('',(#1012),#8567,.T.);
#9076=ADVANCED_FACE('',(#1013,#315),#503,.F.);
#9077=ADVANCED_FACE('',(#1014),#8568,.F.);
#9078=ADVANCED_FACE('',(#1015,#316),#504,.T.);
#9079=ADVANCED_FACE('',(#1016),#230,.T.);
#9080=ADVANCED_FACE('',(#1017,#317),#505,.F.);
#9081=ADVANCED_FACE('',(#1018),#8569,.F.);
#9082=ADVANCED_FACE('',(#1019,#318),#506,.T.);
#9083=ADVANCED_FACE('',(#1020),#198,.F.);
#9084=ADVANCED_FACE('',(#1021),#8570,.T.);
#9085=ADVANCED_FACE('',(#1022,#319),#507,.F.);
#9086=ADVANCED_FACE('',(#1023),#8571,.T.);
#9087=ADVANCED_FACE('',(#1024),#508,.F.);
#9088=ADVANCED_FACE('',(#1025),#400,.F.);
#9089=ADVANCED_FACE('',(#1026),#401,.F.);
#9090=ADVANCED_FACE('',(#1027),#402,.F.);
#9091=ADVANCED_FACE('',(#1028),#403,.F.);
#9092=ADVANCED_FACE('',(#1029),#404,.F.);
#9093=ADVANCED_FACE('',(#1030),#405,.F.);
#9094=ADVANCED_FACE('',(#1031),#406,.F.);
#9095=ADVANCED_FACE('',(#1032),#407,.F.);
#9096=ADVANCED_FACE('',(#1033),#408,.F.);
#9097=ADVANCED_FACE('',(#1034),#509,.T.);
#9098=ADVANCED_FACE('',(#1035),#8572,.T.);
#9099=ADVANCED_FACE('',(#1036),#510,.T.);
#9100=ADVANCED_FACE('',(#1037),#8573,.T.);
#9101=ADVANCED_FACE('',(#1038),#511,.T.);
#9102=ADVANCED_FACE('',(#1039),#8574,.T.);
#9103=ADVANCED_FACE('',(#1040),#512,.T.);
#9104=ADVANCED_FACE('',(#1041),#8575,.T.);
#9105=ADVANCED_FACE('',(#1042),#513,.T.);
#9106=ADVANCED_FACE('',(#1043),#8576,.T.);
#9107=ADVANCED_FACE('',(#1044),#514,.T.);
#9108=ADVANCED_FACE('',(#1045),#231,.T.);
#9109=ADVANCED_FACE('',(#1046,#320),#515,.F.);
#9110=ADVANCED_FACE('',(#1047),#8577,.F.);
#9111=ADVANCED_FACE('',(#1048,#321),#516,.T.);
#9112=ADVANCED_FACE('',(#1049),#8578,.T.);
#9113=ADVANCED_FACE('',(#1050,#322),#517,.T.);
#9114=ADVANCED_FACE('',(#1051),#8579,.T.);
#9115=ADVANCED_FACE('',(#1052),#286,.T.);
#9116=ADVANCED_FACE('',(#1053),#8580,.F.);
#9117=ADVANCED_FACE('',(#1054),#287,.F.);
#9118=CLOSED_SHELL('',(#8581,#8582,#8583,#8584,#8585,#8586,#8587,#8588,
#8589,#8590,#8591,#8592,#8593,#8594,#8595,#8596,#8597,#8598,#8599,#8600,
#8601,#8602,#8603,#8604,#8605,#8606,#8607,#8608,#8609,#8610,#8611,#8612,
#8613,#8614,#8615,#8616,#8617));
#9119=CLOSED_SHELL('',(#8618,#8619,#8620,#8621,#8622,#8623,#8624,#8625,
#8626,#8627,#8628,#8629,#8630,#8631,#8632,#8633,#8634,#8635,#8636,#8637,
#8638,#8639,#8640,#8641,#8642,#8643,#8644,#8645,#8646,#8647,#8648,#8649,
#8650,#8651,#8652,#8653,#8654,#8655,#8656,#8657,#8658,#8659,#8660,#8661,
#8662,#8663,#8664,#8665,#8666,#8667,#8668,#8669,#8670,#8671,#8672,#8673,
#8674,#8675,#8676,#8677,#8678,#8679,#8680,#8681,#8682,#8683,#8684,#8685,
#8686,#8687,#8688,#8689,#8690,#8691,#8692,#8693,#8694,#8695,#8696,#8697,
#8698,#8699,#8700,#8701,#8702,#8703,#8704,#8705,#8706,#8707,#8708,#8709,
#8710,#8711,#8712,#8713,#8714,#8715,#8716,#8717,#8718,#8719,#8720,#8721,
#8722,#8723,#8724,#8725,#8726,#8727,#8728,#8729,#8730,#8731,#8732,#8733,
#8734,#8735,#8736,#8737,#8738,#8739,#8740,#8741,#8742,#8743,#8744,#8745,
#8746,#8747,#8748,#8749,#8750,#8751,#8752,#8753,#8754,#8755));
#9120=CLOSED_SHELL('',(#8756,#8757,#8758,#8759,#8760,#8761,#8762,#8763,
#8764,#8765,#8766,#8767,#8768,#8769,#8770,#8771,#8772,#8773,#8774,#8775,
#8776,#8777,#8778,#8779,#8780,#8781,#8782,#8783,#8784,#8785,#8786,#8787,
#8788));
#9121=CLOSED_SHELL('',(#8789,#8790,#8791,#8792));
#9122=CLOSED_SHELL('',(#8793,#8794,#8795,#8796,#8797,#8798,#8799,#8800,
#8801,#8802,#8803,#8804,#8805,#8806,#8807,#8808,#8809,#8810,#8811,#8812,
#8813,#8814,#8815,#8816,#8817,#8818,#8819,#8820,#8821,#8822,#8823,#8824,
#8825,#8826,#8827,#8828,#8829,#8830,#8831,#8832,#8833,#8834,#8835,#8836,
#8837,#8838,#8839,#8840,#8841,#8842,#8843));
#9123=CLOSED_SHELL('',(#8844,#8845,#8846,#8847,#8848,#8849,#8850,#8851,
#8852,#8853,#8854,#8855,#8856,#8857,#8858,#8859,#8860,#8861,#8862,#8863,
#8864,#8865,#8866,#8867,#8868,#8869,#8870,#8871,#8872,#8873,#8874,#8875,
#8876,#8877,#8878,#8879,#8880,#8881,#8882,#8883,#8884,#8885,#8886,#8887,
#8888,#8889,#8890,#8891,#8892,#8893,#8894,#8895,#8896,#8897,#8898,#8899,
#8900,#8901,#8902,#8903,#8904,#8905,#8906,#8907,#8908,#8909,#8910,#8911,
#8912,#8913,#8914,#8915,#8916,#8917,#8918,#8919,#8920,#8921,#8922,#8923,
#8924,#8925,#8926,#8927,#8928,#8929,#8930,#8931,#8932,#8933,#8934));
#9124=CLOSED_SHELL('',(#8935,#8936,#8937,#8938,#8939,#8940,#8941,#8942,
#8943,#8944,#8945,#8946,#8947,#8948,#8949,#8950,#8951,#8952,#8953,#8954,
#8955,#8956,#8957,#8958,#8959,#8960,#8961,#8962,#8963,#8964,#8965,#8966,
#8967,#8968,#8969,#8970,#8971,#8972,#8973,#8974,#8975,#8976,#8977,#8978,
#8979,#8980,#8981,#8982,#8983,#8984,#8985));
#9125=CLOSED_SHELL('',(#8986,#8987,#8988,#8989,#8990,#8991,#8992,#8993,
#8994,#8995,#8996,#8997,#8998,#8999,#9000,#9001,#9002,#9003,#9004,#9005,
#9006,#9007,#9008,#9009,#9010,#9011,#9012,#9013,#9014,#9015,#9016,#9017,
#9018,#9019,#9020,#9021,#9022,#9023,#9024,#9025,#9026,#9027,#9028,#9029,
#9030,#9031,#9032,#9033,#9034,#9035,#9036,#9037,#9038,#9039,#9040,#9041,
#9042,#9043,#9044,#9045,#9046,#9047,#9048,#9049,#9050,#9051,#9052,#9053,
#9054,#9055,#9056,#9057,#9058,#9059,#9060,#9061,#9062,#9063,#9064,#9065,
#9066,#9067,#9068,#9069,#9070,#9071,#9072,#9073,#9074,#9075));
#9126=CLOSED_SHELL('',(#9076,#9077,#9078,#9079));
#9127=CLOSED_SHELL('',(#9080,#9081,#9082,#9083,#9084,#9085,#9086,#9087,
#9088,#9089,#9090,#9091,#9092,#9093,#9094,#9095,#9096,#9097,#9098,#9099,
#9100,#9101,#9102,#9103,#9104,#9105,#9106,#9107));
#9128=CLOSED_SHELL('',(#9108));
#9129=CLOSED_SHELL('',(#9109,#9110,#9111,#9112));
#9130=CLOSED_SHELL('',(#9113,#9114,#9115,#9116,#9117));
#9131=DERIVED_UNIT_ELEMENT(#9157,1.);
#9132=DERIVED_UNIT_ELEMENT(#52166,-3.);
#9133=DERIVED_UNIT_ELEMENT(#9157,1.);
#9134=DERIVED_UNIT_ELEMENT(#52166,-3.);
#9135=DERIVED_UNIT_ELEMENT(#9157,1.);
#9136=DERIVED_UNIT_ELEMENT(#52166,-3.);
#9137=DERIVED_UNIT_ELEMENT(#9157,1.);
#9138=DERIVED_UNIT_ELEMENT(#52166,-3.);
#9139=DERIVED_UNIT_ELEMENT(#9157,1.);
#9140=DERIVED_UNIT_ELEMENT(#52166,-3.);
#9141=DERIVED_UNIT_ELEMENT(#9157,1.);
#9142=DERIVED_UNIT_ELEMENT(#52166,-3.);
#9143=DERIVED_UNIT_ELEMENT(#9157,1.);
#9144=DERIVED_UNIT_ELEMENT(#52166,-3.);
#9145=DERIVED_UNIT_ELEMENT(#9157,1.);
#9146=DERIVED_UNIT_ELEMENT(#52166,-3.);
#9147=DERIVED_UNIT_ELEMENT(#9157,1.);
#9148=DERIVED_UNIT_ELEMENT(#52166,-3.);
#9149=DERIVED_UNIT_ELEMENT(#9157,1.);
#9150=DERIVED_UNIT_ELEMENT(#52166,-3.);
#9151=DERIVED_UNIT_ELEMENT(#9157,1.);
#9152=DERIVED_UNIT_ELEMENT(#52166,-3.);
#9153=DERIVED_UNIT_ELEMENT(#9157,1.);
#9154=DERIVED_UNIT_ELEMENT(#52166,-3.);
#9155=DERIVED_UNIT_ELEMENT(#9157,1.);
#9156=DERIVED_UNIT_ELEMENT(#52166,-3.);
#9157=(
MASS_UNIT()
NAMED_UNIT(*)
SI_UNIT(.KILO.,.GRAM.)
);
#9158=DERIVED_UNIT((#9131,#9132));
#9159=DERIVED_UNIT((#9133,#9134));
#9160=DERIVED_UNIT((#9135,#9136));
#9161=DERIVED_UNIT((#9137,#9138));
#9162=DERIVED_UNIT((#9139,#9140));
#9163=DERIVED_UNIT((#9141,#9142));
#9164=DERIVED_UNIT((#9143,#9144));
#9165=DERIVED_UNIT((#9145,#9146));
#9166=DERIVED_UNIT((#9147,#9148));
#9167=DERIVED_UNIT((#9149,#9150));
#9168=DERIVED_UNIT((#9151,#9152));
#9169=DERIVED_UNIT((#9153,#9154));
#9170=DERIVED_UNIT((#9155,#9156));
#9171=MEASURE_REPRESENTATION_ITEM('density measure',
POSITIVE_RATIO_MEASURE(0.),#9158);
#9172=MEASURE_REPRESENTATION_ITEM('density measure',
POSITIVE_RATIO_MEASURE(0.),#9159);
#9173=MEASURE_REPRESENTATION_ITEM('density measure',
POSITIVE_RATIO_MEASURE(0.),#9160);
#9174=MEASURE_REPRESENTATION_ITEM('density measure',
POSITIVE_RATIO_MEASURE(0.),#9161);
#9175=MEASURE_REPRESENTATION_ITEM('density measure',
POSITIVE_RATIO_MEASURE(0.),#9162);
#9176=MEASURE_REPRESENTATION_ITEM('density measure',
POSITIVE_RATIO_MEASURE(0.),#9163);
#9177=MEASURE_REPRESENTATION_ITEM('density measure',
POSITIVE_RATIO_MEASURE(0.),#9164);
#9178=MEASURE_REPRESENTATION_ITEM('density measure',
POSITIVE_RATIO_MEASURE(0.),#9165);
#9179=MEASURE_REPRESENTATION_ITEM('density measure',
POSITIVE_RATIO_MEASURE(0.),#9166);
#9180=MEASURE_REPRESENTATION_ITEM('density measure',
POSITIVE_RATIO_MEASURE(0.),#9167);
#9181=MEASURE_REPRESENTATION_ITEM('density measure',
POSITIVE_RATIO_MEASURE(0.),#9168);
#9182=MEASURE_REPRESENTATION_ITEM('density measure',
POSITIVE_RATIO_MEASURE(0.),#9169);
#9183=MEASURE_REPRESENTATION_ITEM('density measure',
POSITIVE_RATIO_MEASURE(0.),#9170);
#9184=PROPERTY_DEFINITION_REPRESENTATION(#9249,#9210);
#9185=PROPERTY_DEFINITION_REPRESENTATION(#9250,#9211);
#9186=PROPERTY_DEFINITION_REPRESENTATION(#9251,#9212);
#9187=PROPERTY_DEFINITION_REPRESENTATION(#9252,#9213);
#9188=PROPERTY_DEFINITION_REPRESENTATION(#9253,#9214);
#9189=PROPERTY_DEFINITION_REPRESENTATION(#9254,#9215);
#9190=PROPERTY_DEFINITION_REPRESENTATION(#9255,#9216);
#9191=PROPERTY_DEFINITION_REPRESENTATION(#9256,#9217);
#9192=PROPERTY_DEFINITION_REPRESENTATION(#9257,#9218);
#9193=PROPERTY_DEFINITION_REPRESENTATION(#9258,#9219);
#9194=PROPERTY_DEFINITION_REPRESENTATION(#9259,#9220);
#9195=PROPERTY_DEFINITION_REPRESENTATION(#9260,#9221);
#9196=PROPERTY_DEFINITION_REPRESENTATION(#9261,#9222);
#9197=PROPERTY_DEFINITION_REPRESENTATION(#9262,#9223);
#9198=PROPERTY_DEFINITION_REPRESENTATION(#9263,#9224);
#9199=PROPERTY_DEFINITION_REPRESENTATION(#9264,#9225);
#9200=PROPERTY_DEFINITION_REPRESENTATION(#9265,#9226);
#9201=PROPERTY_DEFINITION_REPRESENTATION(#9266,#9227);
#9202=PROPERTY_DEFINITION_REPRESENTATION(#9267,#9228);
#9203=PROPERTY_DEFINITION_REPRESENTATION(#9268,#9229);
#9204=PROPERTY_DEFINITION_REPRESENTATION(#9269,#9230);
#9205=PROPERTY_DEFINITION_REPRESENTATION(#9270,#9231);
#9206=PROPERTY_DEFINITION_REPRESENTATION(#9271,#9232);
#9207=PROPERTY_DEFINITION_REPRESENTATION(#9272,#9233);
#9208=PROPERTY_DEFINITION_REPRESENTATION(#9273,#9234);
#9209=PROPERTY_DEFINITION_REPRESENTATION(#9274,#9235);
#9210=REPRESENTATION('material name',(#9236),#52151);
#9211=REPRESENTATION('density',(#9171),#52151);
#9212=REPRESENTATION('material name',(#9237),#52152);
#9213=REPRESENTATION('density',(#9172),#52152);
#9214=REPRESENTATION('material name',(#9238),#52153);
#9215=REPRESENTATION('density',(#9173),#52153);
#9216=REPRESENTATION('material name',(#9239),#52154);
#9217=REPRESENTATION('density',(#9174),#52154);
#9218=REPRESENTATION('material name',(#9240),#52155);
#9219=REPRESENTATION('density',(#9175),#52155);
#9220=REPRESENTATION('material name',(#9241),#52156);
#9221=REPRESENTATION('density',(#9176),#52156);
#9222=REPRESENTATION('material name',(#9242),#52157);
#9223=REPRESENTATION('density',(#9177),#52157);
#9224=REPRESENTATION('material name',(#9243),#52158);
#9225=REPRESENTATION('density',(#9178),#52158);
#9226=REPRESENTATION('material name',(#9244),#52159);
#9227=REPRESENTATION('density',(#9179),#52159);
#9228=REPRESENTATION('material name',(#9245),#52160);
#9229=REPRESENTATION('density',(#9180),#52160);
#9230=REPRESENTATION('material name',(#9246),#52161);
#9231=REPRESENTATION('density',(#9181),#52161);
#9232=REPRESENTATION('material name',(#9247),#52162);
#9233=REPRESENTATION('density',(#9182),#52162);
#9234=REPRESENTATION('material name',(#9248),#52163);
#9235=REPRESENTATION('density',(#9183),#52163);
#9236=DESCRIPTIVE_REPRESENTATION_ITEM('MODELED_BY','MODELED_BY');
#9237=DESCRIPTIVE_REPRESENTATION_ITEM('MODELED_BY','MODELED_BY');
#9238=DESCRIPTIVE_REPRESENTATION_ITEM('MODELED_BY','MODELED_BY');
#9239=DESCRIPTIVE_REPRESENTATION_ITEM('MODELED_BY','MODELED_BY');
#9240=DESCRIPTIVE_REPRESENTATION_ITEM('MODELED_BY','MODELED_BY');
#9241=DESCRIPTIVE_REPRESENTATION_ITEM('MODELED_BY','MODELED_BY');
#9242=DESCRIPTIVE_REPRESENTATION_ITEM('MODELED_BY','MODELED_BY');
#9243=DESCRIPTIVE_REPRESENTATION_ITEM('MODELED_BY','MODELED_BY');
#9244=DESCRIPTIVE_REPRESENTATION_ITEM('MODELED_BY','MODELED_BY');
#9245=DESCRIPTIVE_REPRESENTATION_ITEM('MODELED_BY','MODELED_BY');
#9246=DESCRIPTIVE_REPRESENTATION_ITEM('MODELED_BY','MODELED_BY');
#9247=DESCRIPTIVE_REPRESENTATION_ITEM('MODELED_BY','MODELED_BY');
#9248=DESCRIPTIVE_REPRESENTATION_ITEM('MODELED_BY','MODELED_BY');
#9249=PROPERTY_DEFINITION('material property','material name',#52226);
#9250=PROPERTY_DEFINITION('material property','density of part',#52226);
#9251=PROPERTY_DEFINITION('material property','material name',#52227);
#9252=PROPERTY_DEFINITION('material property','density of part',#52227);
#9253=PROPERTY_DEFINITION('material property','material name',#52228);
#9254=PROPERTY_DEFINITION('material property','density of part',#52228);
#9255=PROPERTY_DEFINITION('material property','material name',#52229);
#9256=PROPERTY_DEFINITION('material property','density of part',#52229);
#9257=PROPERTY_DEFINITION('material property','material name',#52230);
#9258=PROPERTY_DEFINITION('material property','density of part',#52230);
#9259=PROPERTY_DEFINITION('material property','material name',#52231);
#9260=PROPERTY_DEFINITION('material property','density of part',#52231);
#9261=PROPERTY_DEFINITION('material property','material name',#52232);
#9262=PROPERTY_DEFINITION('material property','density of part',#52232);
#9263=PROPERTY_DEFINITION('material property','material name',#52233);
#9264=PROPERTY_DEFINITION('material property','density of part',#52233);
#9265=PROPERTY_DEFINITION('material property','material name',#52234);
#9266=PROPERTY_DEFINITION('material property','density of part',#52234);
#9267=PROPERTY_DEFINITION('material property','material name',#52235);
#9268=PROPERTY_DEFINITION('material property','density of part',#52235);
#9269=PROPERTY_DEFINITION('material property','material name',#52236);
#9270=PROPERTY_DEFINITION('material property','density of part',#52236);
#9271=PROPERTY_DEFINITION('material property','material name',#52237);
#9272=PROPERTY_DEFINITION('material property','density of part',#52237);
#9273=PROPERTY_DEFINITION('material property','material name',#52238);
#9274=PROPERTY_DEFINITION('material property','density of part',#52238);
#9275=AXIS2_PLACEMENT_3D('',#12545,#10210,#10211);
#9276=AXIS2_PLACEMENT_3D('',#12546,#10212,#10213);
#9277=AXIS2_PLACEMENT_3D('',#12547,#10214,#10215);
#9278=AXIS2_PLACEMENT_3D('',#12606,#10218,#10219);
#9279=AXIS2_PLACEMENT_3D('',#12608,#10221,#10222);
#9280=AXIS2_PLACEMENT_3D('',#12718,#10224,#10225);
#9281=AXIS2_PLACEMENT_3D('',#12833,#10227,#10228);
#9282=AXIS2_PLACEMENT_3D('',#12948,#10230,#10231);
#9283=AXIS2_PLACEMENT_3D('',#13058,#10233,#10234);
#9284=AXIS2_PLACEMENT_3D('',#13086,#10235,#10236);
#9285=AXIS2_PLACEMENT_3D('',#13142,#10238,#10239);
#9286=AXIS2_PLACEMENT_3D('',#13605,#10242,#10243);
#9287=AXIS2_PLACEMENT_3D('',#15449,#10247,#10248);
#9288=AXIS2_PLACEMENT_3D('',#15452,#10249,#10250);
#9289=AXIS2_PLACEMENT_3D('',#15474,#10252,#10253);
#9290=AXIS2_PLACEMENT_3D('',#15517,#10255,#10256);
#9291=AXIS2_PLACEMENT_3D('',#18579,#10265,#10266);
#9292=AXIS2_PLACEMENT_3D('',#18684,#10268,#10269);
#9293=AXIS2_PLACEMENT_3D('',#18685,#10270,#10271);
#9294=AXIS2_PLACEMENT_3D('',#18687,#10273,#10274);
#9295=AXIS2_PLACEMENT_3D('',#18969,#10276,#10277);
#9296=AXIS2_PLACEMENT_3D('',#18971,#10278,#10279);
#9297=AXIS2_PLACEMENT_3D('',#18972,#10280,#10281);
#9298=AXIS2_PLACEMENT_3D('',#18975,#10282,#10283);
#9299=AXIS2_PLACEMENT_3D('',#18976,#10284,#10285);
#9300=AXIS2_PLACEMENT_3D('',#18978,#10287,#10288);
#9301=AXIS2_PLACEMENT_3D('',#18980,#10289,#10290);
#9302=AXIS2_PLACEMENT_3D('',#18981,#10291,#10292);
#9303=AXIS2_PLACEMENT_3D('',#18982,#10293,#10294);
#9304=AXIS2_PLACEMENT_3D('',#18985,#10295,#10296);
#9305=AXIS2_PLACEMENT_3D('',#18987,#10297,#10298);
#9306=AXIS2_PLACEMENT_3D('',#18989,#10299,#10300);
#9307=AXIS2_PLACEMENT_3D('',#18991,#10301,#10302);
#9308=AXIS2_PLACEMENT_3D('',#18993,#10303,#10304);
#9309=AXIS2_PLACEMENT_3D('',#18995,#10305,#10306);
#9310=AXIS2_PLACEMENT_3D('',#18997,#10307,#10308);
#9311=AXIS2_PLACEMENT_3D('',#18999,#10309,#10310);
#9312=AXIS2_PLACEMENT_3D('',#19001,#10311,#10312);
#9313=AXIS2_PLACEMENT_3D('',#19003,#10313,#10314);
#9314=AXIS2_PLACEMENT_3D('',#19005,#10315,#10316);
#9315=AXIS2_PLACEMENT_3D('',#19007,#10317,#10318);
#9316=AXIS2_PLACEMENT_3D('',#19009,#10319,#10320);
#9317=AXIS2_PLACEMENT_3D('',#19011,#10321,#10322);
#9318=AXIS2_PLACEMENT_3D('',#19013,#10323,#10324);
#9319=AXIS2_PLACEMENT_3D('',#19015,#10325,#10326);
#9320=AXIS2_PLACEMENT_3D('',#19017,#10327,#10328);
#9321=AXIS2_PLACEMENT_3D('',#19019,#10329,#10330);
#9322=AXIS2_PLACEMENT_3D('',#19021,#10331,#10332);
#9323=AXIS2_PLACEMENT_3D('',#19023,#10333,#10334);
#9324=AXIS2_PLACEMENT_3D('',#19025,#10335,#10336);
#9325=AXIS2_PLACEMENT_3D('',#19027,#10337,#10338);
#9326=AXIS2_PLACEMENT_3D('',#19029,#10339,#10340);
#9327=AXIS2_PLACEMENT_3D('',#19031,#10341,#10342);
#9328=AXIS2_PLACEMENT_3D('',#19033,#10343,#10344);
#9329=AXIS2_PLACEMENT_3D('',#19035,#10345,#10346);
#9330=AXIS2_PLACEMENT_3D('',#19037,#10347,#10348);
#9331=AXIS2_PLACEMENT_3D('',#19039,#10349,#10350);
#9332=AXIS2_PLACEMENT_3D('',#19041,#10351,#10352);
#9333=AXIS2_PLACEMENT_3D('',#19043,#10353,#10354);
#9334=AXIS2_PLACEMENT_3D('',#19045,#10355,#10356);
#9335=AXIS2_PLACEMENT_3D('',#19047,#10357,#10358);
#9336=AXIS2_PLACEMENT_3D('',#19049,#10359,#10360);
#9337=AXIS2_PLACEMENT_3D('',#19051,#10361,#10362);
#9338=AXIS2_PLACEMENT_3D('',#19053,#10363,#10364);
#9339=AXIS2_PLACEMENT_3D('',#19055,#10365,#10366);
#9340=AXIS2_PLACEMENT_3D('',#19057,#10367,#10368);
#9341=AXIS2_PLACEMENT_3D('',#19059,#10369,#10370);
#9342=AXIS2_PLACEMENT_3D('',#19061,#10371,#10372);
#9343=AXIS2_PLACEMENT_3D('',#19063,#10373,#10374);
#9344=AXIS2_PLACEMENT_3D('',#19065,#10375,#10376);
#9345=AXIS2_PLACEMENT_3D('',#19067,#10377,#10378);
#9346=AXIS2_PLACEMENT_3D('',#19069,#10379,#10380);
#9347=AXIS2_PLACEMENT_3D('',#19071,#10381,#10382);
#9348=AXIS2_PLACEMENT_3D('',#19073,#10383,#10384);
#9349=AXIS2_PLACEMENT_3D('',#19075,#10385,#10386);
#9350=AXIS2_PLACEMENT_3D('',#19077,#10387,#10388);
#9351=AXIS2_PLACEMENT_3D('',#19079,#10389,#10390);
#9352=AXIS2_PLACEMENT_3D('',#19081,#10391,#10392);
#9353=AXIS2_PLACEMENT_3D('',#19083,#10393,#10394);
#9354=AXIS2_PLACEMENT_3D('',#19085,#10395,#10396);
#9355=AXIS2_PLACEMENT_3D('',#19087,#10397,#10398);
#9356=AXIS2_PLACEMENT_3D('',#19089,#10399,#10400);
#9357=AXIS2_PLACEMENT_3D('',#19091,#10401,#10402);
#9358=AXIS2_PLACEMENT_3D('',#19093,#10403,#10404);
#9359=AXIS2_PLACEMENT_3D('',#19095,#10405,#10406);
#9360=AXIS2_PLACEMENT_3D('',#19097,#10407,#10408);
#9361=AXIS2_PLACEMENT_3D('',#19099,#10409,#10410);
#9362=AXIS2_PLACEMENT_3D('',#19101,#10411,#10412);
#9363=AXIS2_PLACEMENT_3D('',#19103,#10413,#10414);
#9364=AXIS2_PLACEMENT_3D('',#19105,#10415,#10416);
#9365=AXIS2_PLACEMENT_3D('',#19107,#10417,#10418);
#9366=AXIS2_PLACEMENT_3D('',#19109,#10419,#10420);
#9367=AXIS2_PLACEMENT_3D('',#19111,#10421,#10422);
#9368=AXIS2_PLACEMENT_3D('',#19113,#10423,#10424);
#9369=AXIS2_PLACEMENT_3D('',#19115,#10425,#10426);
#9370=AXIS2_PLACEMENT_3D('',#19117,#10427,#10428);
#9371=AXIS2_PLACEMENT_3D('',#19119,#10429,#10430);
#9372=AXIS2_PLACEMENT_3D('',#19121,#10431,#10432);
#9373=AXIS2_PLACEMENT_3D('',#19123,#10433,#10434);
#9374=AXIS2_PLACEMENT_3D('',#19125,#10435,#10436);
#9375=AXIS2_PLACEMENT_3D('',#19127,#10437,#10438);
#9376=AXIS2_PLACEMENT_3D('',#19129,#10439,#10440);
#9377=AXIS2_PLACEMENT_3D('',#19131,#10441,#10442);
#9378=AXIS2_PLACEMENT_3D('',#19133,#10443,#10444);
#9379=AXIS2_PLACEMENT_3D('',#19135,#10445,#10446);
#9380=AXIS2_PLACEMENT_3D('',#19137,#10447,#10448);
#9381=AXIS2_PLACEMENT_3D('',#19139,#10449,#10450);
#9382=AXIS2_PLACEMENT_3D('',#19141,#10451,#10452);
#9383=AXIS2_PLACEMENT_3D('',#19143,#10453,#10454);
#9384=AXIS2_PLACEMENT_3D('',#19145,#10455,#10456);
#9385=AXIS2_PLACEMENT_3D('',#19147,#10457,#10458);
#9386=AXIS2_PLACEMENT_3D('',#19149,#10459,#10460);
#9387=AXIS2_PLACEMENT_3D('',#19151,#10461,#10462);
#9388=AXIS2_PLACEMENT_3D('',#19153,#10463,#10464);
#9389=AXIS2_PLACEMENT_3D('',#19155,#10465,#10466);
#9390=AXIS2_PLACEMENT_3D('',#19157,#10467,#10468);
#9391=AXIS2_PLACEMENT_3D('',#19159,#10469,#10470);
#9392=AXIS2_PLACEMENT_3D('',#19161,#10471,#10472);
#9393=AXIS2_PLACEMENT_3D('',#19163,#10473,#10474);
#9394=AXIS2_PLACEMENT_3D('',#19165,#10475,#10476);
#9395=AXIS2_PLACEMENT_3D('',#19167,#10477,#10478);
#9396=AXIS2_PLACEMENT_3D('',#19169,#10479,#10480);
#9397=AXIS2_PLACEMENT_3D('',#19171,#10481,#10482);
#9398=AXIS2_PLACEMENT_3D('',#19173,#10483,#10484);
#9399=AXIS2_PLACEMENT_3D('',#19174,#10485,#10486);
#9400=AXIS2_PLACEMENT_3D('',#19187,#10493,#10494);
#9401=AXIS2_PLACEMENT_3D('',#19193,#10498,#10499);
#9402=AXIS2_PLACEMENT_3D('',#19197,#10502,#10503);
#9403=AXIS2_PLACEMENT_3D('',#19201,#10506,#10507);
#9404=AXIS2_PLACEMENT_3D('',#19205,#10510,#10511);
#9405=AXIS2_PLACEMENT_3D('',#19209,#10514,#10515);
#9406=AXIS2_PLACEMENT_3D('',#19211,#10517,#10518);
#9407=AXIS2_PLACEMENT_3D('',#19213,#10519,#10520);
#9408=AXIS2_PLACEMENT_3D('',#19214,#10521,#10522);
#9409=AXIS2_PLACEMENT_3D('',#19217,#10524,#10525);
#9410=AXIS2_PLACEMENT_3D('',#19218,#10526,#10527);
#9411=AXIS2_PLACEMENT_3D('',#19221,#10528,#10529);
#9412=AXIS2_PLACEMENT_3D('',#19223,#10530,#10531);
#9413=AXIS2_PLACEMENT_3D('',#19225,#10532,#10533);
#9414=AXIS2_PLACEMENT_3D('',#19227,#10534,#10535);
#9415=AXIS2_PLACEMENT_3D('',#19229,#10536,#10537);
#9416=AXIS2_PLACEMENT_3D('',#19231,#10538,#10539);
#9417=AXIS2_PLACEMENT_3D('',#19233,#10540,#10541);
#9418=AXIS2_PLACEMENT_3D('',#19235,#10542,#10543);
#9419=AXIS2_PLACEMENT_3D('',#19237,#10544,#10545);
#9420=AXIS2_PLACEMENT_3D('',#19239,#10546,#10547);
#9421=AXIS2_PLACEMENT_3D('',#19241,#10548,#10549);
#9422=AXIS2_PLACEMENT_3D('',#19243,#10550,#10551);
#9423=AXIS2_PLACEMENT_3D('',#19245,#10552,#10553);
#9424=AXIS2_PLACEMENT_3D('',#19247,#10554,#10555);
#9425=AXIS2_PLACEMENT_3D('',#19249,#10556,#10557);
#9426=AXIS2_PLACEMENT_3D('',#19251,#10558,#10559);
#9427=AXIS2_PLACEMENT_3D('',#19253,#10560,#10561);
#9428=AXIS2_PLACEMENT_3D('',#19255,#10562,#10563);
#9429=AXIS2_PLACEMENT_3D('',#19257,#10564,#10565);
#9430=AXIS2_PLACEMENT_3D('',#19259,#10566,#10567);
#9431=AXIS2_PLACEMENT_3D('',#19261,#10568,#10569);
#9432=AXIS2_PLACEMENT_3D('',#19263,#10570,#10571);
#9433=AXIS2_PLACEMENT_3D('',#19265,#10572,#10573);
#9434=AXIS2_PLACEMENT_3D('',#19267,#10574,#10575);
#9435=AXIS2_PLACEMENT_3D('',#19269,#10576,#10577);
#9436=AXIS2_PLACEMENT_3D('',#19271,#10578,#10579);
#9437=AXIS2_PLACEMENT_3D('',#19273,#10580,#10581);
#9438=AXIS2_PLACEMENT_3D('',#19275,#10582,#10583);
#9439=AXIS2_PLACEMENT_3D('',#19277,#10584,#10585);
#9440=AXIS2_PLACEMENT_3D('',#19279,#10586,#10587);
#9441=AXIS2_PLACEMENT_3D('',#19281,#10588,#10589);
#9442=AXIS2_PLACEMENT_3D('',#19283,#10590,#10591);
#9443=AXIS2_PLACEMENT_3D('',#19285,#10592,#10593);
#9444=AXIS2_PLACEMENT_3D('',#19287,#10594,#10595);
#9445=AXIS2_PLACEMENT_3D('',#19289,#10596,#10597);
#9446=AXIS2_PLACEMENT_3D('',#19291,#10598,#10599);
#9447=AXIS2_PLACEMENT_3D('',#19293,#10600,#10601);
#9448=AXIS2_PLACEMENT_3D('',#19295,#10602,#10603);
#9449=AXIS2_PLACEMENT_3D('',#19297,#10604,#10605);
#9450=AXIS2_PLACEMENT_3D('',#19299,#10606,#10607);
#9451=AXIS2_PLACEMENT_3D('',#19301,#10608,#10609);
#9452=AXIS2_PLACEMENT_3D('',#19303,#10610,#10611);
#9453=AXIS2_PLACEMENT_3D('',#19305,#10612,#10613);
#9454=AXIS2_PLACEMENT_3D('',#19307,#10614,#10615);
#9455=AXIS2_PLACEMENT_3D('',#19309,#10616,#10617);
#9456=AXIS2_PLACEMENT_3D('',#19311,#10618,#10619);
#9457=AXIS2_PLACEMENT_3D('',#19313,#10620,#10621);
#9458=AXIS2_PLACEMENT_3D('',#19315,#10622,#10623);
#9459=AXIS2_PLACEMENT_3D('',#19317,#10624,#10625);
#9460=AXIS2_PLACEMENT_3D('',#19319,#10626,#10627);
#9461=AXIS2_PLACEMENT_3D('',#19321,#10628,#10629);
#9462=AXIS2_PLACEMENT_3D('',#19323,#10630,#10631);
#9463=AXIS2_PLACEMENT_3D('',#19325,#10632,#10633);
#9464=AXIS2_PLACEMENT_3D('',#19327,#10634,#10635);
#9465=AXIS2_PLACEMENT_3D('',#19329,#10636,#10637);
#9466=AXIS2_PLACEMENT_3D('',#19331,#10638,#10639);
#9467=AXIS2_PLACEMENT_3D('',#19333,#10640,#10641);
#9468=AXIS2_PLACEMENT_3D('',#19335,#10642,#10643);
#9469=AXIS2_PLACEMENT_3D('',#19337,#10644,#10645);
#9470=AXIS2_PLACEMENT_3D('',#19339,#10646,#10647);
#9471=AXIS2_PLACEMENT_3D('',#19341,#10648,#10649);
#9472=AXIS2_PLACEMENT_3D('',#19343,#10650,#10651);
#9473=AXIS2_PLACEMENT_3D('',#19345,#10652,#10653);
#9474=AXIS2_PLACEMENT_3D('',#19347,#10654,#10655);
#9475=AXIS2_PLACEMENT_3D('',#19349,#10656,#10657);
#9476=AXIS2_PLACEMENT_3D('',#19351,#10658,#10659);
#9477=AXIS2_PLACEMENT_3D('',#19353,#10660,#10661);
#9478=AXIS2_PLACEMENT_3D('',#19355,#10662,#10663);
#9479=AXIS2_PLACEMENT_3D('',#19357,#10664,#10665);
#9480=AXIS2_PLACEMENT_3D('',#19359,#10666,#10667);
#9481=AXIS2_PLACEMENT_3D('',#19361,#10668,#10669);
#9482=AXIS2_PLACEMENT_3D('',#19363,#10670,#10671);
#9483=AXIS2_PLACEMENT_3D('',#19365,#10672,#10673);
#9484=AXIS2_PLACEMENT_3D('',#19367,#10674,#10675);
#9485=AXIS2_PLACEMENT_3D('',#19369,#10676,#10677);
#9486=AXIS2_PLACEMENT_3D('',#19371,#10678,#10679);
#9487=AXIS2_PLACEMENT_3D('',#19373,#10680,#10681);
#9488=AXIS2_PLACEMENT_3D('',#19375,#10682,#10683);
#9489=AXIS2_PLACEMENT_3D('',#19377,#10684,#10685);
#9490=AXIS2_PLACEMENT_3D('',#19379,#10686,#10687);
#9491=AXIS2_PLACEMENT_3D('',#19381,#10688,#10689);
#9492=AXIS2_PLACEMENT_3D('',#19383,#10690,#10691);
#9493=AXIS2_PLACEMENT_3D('',#19385,#10692,#10693);
#9494=AXIS2_PLACEMENT_3D('',#19387,#10694,#10695);
#9495=AXIS2_PLACEMENT_3D('',#19389,#10696,#10697);
#9496=AXIS2_PLACEMENT_3D('',#19391,#10698,#10699);
#9497=AXIS2_PLACEMENT_3D('',#19393,#10700,#10701);
#9498=AXIS2_PLACEMENT_3D('',#19395,#10702,#10703);
#9499=AXIS2_PLACEMENT_3D('',#19397,#10704,#10705);
#9500=AXIS2_PLACEMENT_3D('',#19399,#10706,#10707);
#9501=AXIS2_PLACEMENT_3D('',#19401,#10708,#10709);
#9502=AXIS2_PLACEMENT_3D('',#19403,#10710,#10711);
#9503=AXIS2_PLACEMENT_3D('',#19405,#10712,#10713);
#9504=AXIS2_PLACEMENT_3D('',#19407,#10714,#10715);
#9505=AXIS2_PLACEMENT_3D('',#19409,#10716,#10717);
#9506=AXIS2_PLACEMENT_3D('',#19410,#10718,#10719);
#9507=AXIS2_PLACEMENT_3D('',#19411,#10720,#10721);
#9508=AXIS2_PLACEMENT_3D('',#19414,#10724,#10725);
#9509=AXIS2_PLACEMENT_3D('',#19417,#10728,#10729);
#9510=AXIS2_PLACEMENT_3D('',#19420,#10732,#10733);
#9511=AXIS2_PLACEMENT_3D('',#19423,#10736,#10737);
#9512=AXIS2_PLACEMENT_3D('',#19426,#10740,#10741);
#9513=AXIS2_PLACEMENT_3D('',#19429,#10744,#10745);
#9514=AXIS2_PLACEMENT_3D('',#19432,#10748,#10749);
#9515=AXIS2_PLACEMENT_3D('',#19435,#10752,#10753);
#9516=AXIS2_PLACEMENT_3D('',#19438,#10756,#10757);
#9517=AXIS2_PLACEMENT_3D('',#19441,#10760,#10761);
#9518=AXIS2_PLACEMENT_3D('',#19444,#10764,#10765);
#9519=AXIS2_PLACEMENT_3D('',#19447,#10768,#10769);
#9520=AXIS2_PLACEMENT_3D('',#19450,#10772,#10773);
#9521=AXIS2_PLACEMENT_3D('',#19453,#10776,#10777);
#9522=AXIS2_PLACEMENT_3D('',#19456,#10780,#10781);
#9523=AXIS2_PLACEMENT_3D('',#19459,#10784,#10785);
#9524=AXIS2_PLACEMENT_3D('',#19461,#10787,#10788);
#9525=AXIS2_PLACEMENT_3D('',#19476,#10791,#10792);
#9526=AXIS2_PLACEMENT_3D('',#19478,#10793,#10794);
#9527=AXIS2_PLACEMENT_3D('',#19494,#10795,#10796);
#9528=AXIS2_PLACEMENT_3D('',#19495,#10797,#10798);
#9529=AXIS2_PLACEMENT_3D('',#19497,#10800,#10801);
#9530=AXIS2_PLACEMENT_3D('',#19499,#10803,#10804);
#9531=AXIS2_PLACEMENT_3D('',#19501,#10806,#10807);
#9532=AXIS2_PLACEMENT_3D('',#19502,#10808,#10809);
#9533=AXIS2_PLACEMENT_3D('',#19504,#10811,#10812);
#9534=AXIS2_PLACEMENT_3D('',#19520,#10815,#10816);
#9535=AXIS2_PLACEMENT_3D('',#19537,#10817,#10818);
#9536=AXIS2_PLACEMENT_3D('',#19538,#10819,#10820);
#9537=AXIS2_PLACEMENT_3D('',#19539,#10821,#10822);
#9538=AXIS2_PLACEMENT_3D('',#19543,#10826,#10827);
#9539=AXIS2_PLACEMENT_3D('',#19544,#10828,#10829);
#9540=AXIS2_PLACEMENT_3D('',#19545,#10830,#10831);
#9541=AXIS2_PLACEMENT_3D('',#19546,#10832,#10833);
#9542=AXIS2_PLACEMENT_3D('',#19548,#10835,#10836);
#9543=AXIS2_PLACEMENT_3D('',#19563,#10839,#10840);
#9544=AXIS2_PLACEMENT_3D('',#19565,#10841,#10842);
#9545=AXIS2_PLACEMENT_3D('',#19581,#10843,#10844);
#9546=AXIS2_PLACEMENT_3D('',#19582,#10845,#10846);
#9547=AXIS2_PLACEMENT_3D('',#19584,#10848,#10849);
#9548=AXIS2_PLACEMENT_3D('',#19586,#10851,#10852);
#9549=AXIS2_PLACEMENT_3D('',#19588,#10854,#10855);
#9550=AXIS2_PLACEMENT_3D('',#19589,#10856,#10857);
#9551=AXIS2_PLACEMENT_3D('',#19591,#10859,#10860);
#9552=AXIS2_PLACEMENT_3D('',#19606,#10863,#10864);
#9553=AXIS2_PLACEMENT_3D('',#19608,#10865,#10866);
#9554=AXIS2_PLACEMENT_3D('',#19624,#10867,#10868);
#9555=AXIS2_PLACEMENT_3D('',#19625,#10869,#10870);
#9556=AXIS2_PLACEMENT_3D('',#19627,#10872,#10873);
#9557=AXIS2_PLACEMENT_3D('',#19629,#10875,#10876);
#9558=AXIS2_PLACEMENT_3D('',#19631,#10878,#10879);
#9559=AXIS2_PLACEMENT_3D('',#19632,#10880,#10881);
#9560=AXIS2_PLACEMENT_3D('',#19634,#10883,#10884);
#9561=AXIS2_PLACEMENT_3D('',#19649,#10887,#10888);
#9562=AXIS2_PLACEMENT_3D('',#19651,#10889,#10890);
#9563=AXIS2_PLACEMENT_3D('',#19667,#10891,#10892);
#9564=AXIS2_PLACEMENT_3D('',#19668,#10893,#10894);
#9565=AXIS2_PLACEMENT_3D('',#19670,#10896,#10897);
#9566=AXIS2_PLACEMENT_3D('',#19672,#10899,#10900);
#9567=AXIS2_PLACEMENT_3D('',#19674,#10902,#10903);
#9568=AXIS2_PLACEMENT_3D('',#19675,#10904,#10905);
#9569=AXIS2_PLACEMENT_3D('',#19677,#10907,#10908);
#9570=AXIS2_PLACEMENT_3D('',#19692,#10911,#10912);
#9571=AXIS2_PLACEMENT_3D('',#19694,#10913,#10914);
#9572=AXIS2_PLACEMENT_3D('',#19710,#10915,#10916);
#9573=AXIS2_PLACEMENT_3D('',#19711,#10917,#10918);
#9574=AXIS2_PLACEMENT_3D('',#19713,#10920,#10921);
#9575=AXIS2_PLACEMENT_3D('',#19715,#10923,#10924);
#9576=AXIS2_PLACEMENT_3D('',#19717,#10926,#10927);
#9577=AXIS2_PLACEMENT_3D('',#19718,#10928,#10929);
#9578=AXIS2_PLACEMENT_3D('',#19720,#10931,#10932);
#9579=AXIS2_PLACEMENT_3D('',#19735,#10935,#10936);
#9580=AXIS2_PLACEMENT_3D('',#19737,#10937,#10938);
#9581=AXIS2_PLACEMENT_3D('',#19753,#10939,#10940);
#9582=AXIS2_PLACEMENT_3D('',#19754,#10941,#10942);
#9583=AXIS2_PLACEMENT_3D('',#19756,#10944,#10945);
#9584=AXIS2_PLACEMENT_3D('',#19758,#10947,#10948);
#9585=AXIS2_PLACEMENT_3D('',#19760,#10950,#10951);
#9586=AXIS2_PLACEMENT_3D('',#19761,#10952,#10953);
#9587=AXIS2_PLACEMENT_3D('',#19763,#10955,#10956);
#9588=AXIS2_PLACEMENT_3D('',#19778,#10959,#10960);
#9589=AXIS2_PLACEMENT_3D('',#19780,#10961,#10962);
#9590=AXIS2_PLACEMENT_3D('',#19796,#10963,#10964);
#9591=AXIS2_PLACEMENT_3D('',#19797,#10965,#10966);
#9592=AXIS2_PLACEMENT_3D('',#19799,#10968,#10969);
#9593=AXIS2_PLACEMENT_3D('',#19801,#10971,#10972);
#9594=AXIS2_PLACEMENT_3D('',#19803,#10974,#10975);
#9595=AXIS2_PLACEMENT_3D('',#19804,#10976,#10977);
#9596=AXIS2_PLACEMENT_3D('',#19806,#10979,#10980);
#9597=AXIS2_PLACEMENT_3D('',#19821,#10983,#10984);
#9598=AXIS2_PLACEMENT_3D('',#19823,#10985,#10986);
#9599=AXIS2_PLACEMENT_3D('',#19839,#10987,#10988);
#9600=AXIS2_PLACEMENT_3D('',#19840,#10989,#10990);
#9601=AXIS2_PLACEMENT_3D('',#19842,#10992,#10993);
#9602=AXIS2_PLACEMENT_3D('',#19844,#10995,#10996);
#9603=AXIS2_PLACEMENT_3D('',#19846,#10998,#10999);
#9604=AXIS2_PLACEMENT_3D('',#19847,#11000,#11001);
#9605=AXIS2_PLACEMENT_3D('',#19849,#11003,#11004);
#9606=AXIS2_PLACEMENT_3D('',#19864,#11007,#11008);
#9607=AXIS2_PLACEMENT_3D('',#19866,#11009,#11010);
#9608=AXIS2_PLACEMENT_3D('',#19882,#11011,#11012);
#9609=AXIS2_PLACEMENT_3D('',#19883,#11013,#11014);
#9610=AXIS2_PLACEMENT_3D('',#19885,#11016,#11017);
#9611=AXIS2_PLACEMENT_3D('',#19887,#11019,#11020);
#9612=AXIS2_PLACEMENT_3D('',#19889,#11022,#11023);
#9613=AXIS2_PLACEMENT_3D('',#19890,#11024,#11025);
#9614=AXIS2_PLACEMENT_3D('',#19892,#11027,#11028);
#9615=AXIS2_PLACEMENT_3D('',#19907,#11031,#11032);
#9616=AXIS2_PLACEMENT_3D('',#19909,#11033,#11034);
#9617=AXIS2_PLACEMENT_3D('',#19925,#11035,#11036);
#9618=AXIS2_PLACEMENT_3D('',#19926,#11037,#11038);
#9619=AXIS2_PLACEMENT_3D('',#19928,#11040,#11041);
#9620=AXIS2_PLACEMENT_3D('',#19930,#11043,#11044);
#9621=AXIS2_PLACEMENT_3D('',#19932,#11046,#11047);
#9622=AXIS2_PLACEMENT_3D('',#19933,#11048,#11049);
#9623=AXIS2_PLACEMENT_3D('',#19935,#11051,#11052);
#9624=AXIS2_PLACEMENT_3D('',#19950,#11055,#11056);
#9625=AXIS2_PLACEMENT_3D('',#19952,#11057,#11058);
#9626=AXIS2_PLACEMENT_3D('',#19968,#11059,#11060);
#9627=AXIS2_PLACEMENT_3D('',#19969,#11061,#11062);
#9628=AXIS2_PLACEMENT_3D('',#19971,#11064,#11065);
#9629=AXIS2_PLACEMENT_3D('',#19973,#11067,#11068);
#9630=AXIS2_PLACEMENT_3D('',#19975,#11070,#11071);
#9631=AXIS2_PLACEMENT_3D('',#19976,#11072,#11073);
#9632=AXIS2_PLACEMENT_3D('',#19978,#11075,#11076);
#9633=AXIS2_PLACEMENT_3D('',#19993,#11079,#11080);
#9634=AXIS2_PLACEMENT_3D('',#19995,#11081,#11082);
#9635=AXIS2_PLACEMENT_3D('',#20011,#11083,#11084);
#9636=AXIS2_PLACEMENT_3D('',#20012,#11085,#11086);
#9637=AXIS2_PLACEMENT_3D('',#20014,#11088,#11089);
#9638=AXIS2_PLACEMENT_3D('',#20016,#11091,#11092);
#9639=AXIS2_PLACEMENT_3D('',#20018,#11094,#11095);
#9640=AXIS2_PLACEMENT_3D('',#20019,#11096,#11097);
#9641=AXIS2_PLACEMENT_3D('',#20021,#11099,#11100);
#9642=AXIS2_PLACEMENT_3D('',#20036,#11103,#11104);
#9643=AXIS2_PLACEMENT_3D('',#20038,#11105,#11106);
#9644=AXIS2_PLACEMENT_3D('',#20054,#11107,#11108);
#9645=AXIS2_PLACEMENT_3D('',#20055,#11109,#11110);
#9646=AXIS2_PLACEMENT_3D('',#20057,#11112,#11113);
#9647=AXIS2_PLACEMENT_3D('',#20059,#11115,#11116);
#9648=AXIS2_PLACEMENT_3D('',#20061,#11118,#11119);
#9649=AXIS2_PLACEMENT_3D('',#20062,#11120,#11121);
#9650=AXIS2_PLACEMENT_3D('',#20064,#11123,#11124);
#9651=AXIS2_PLACEMENT_3D('',#20079,#11127,#11128);
#9652=AXIS2_PLACEMENT_3D('',#20081,#11129,#11130);
#9653=AXIS2_PLACEMENT_3D('',#20097,#11131,#11132);
#9654=AXIS2_PLACEMENT_3D('',#20098,#11133,#11134);
#9655=AXIS2_PLACEMENT_3D('',#20100,#11136,#11137);
#9656=AXIS2_PLACEMENT_3D('',#20102,#11139,#11140);
#9657=AXIS2_PLACEMENT_3D('',#20104,#11142,#11143);
#9658=AXIS2_PLACEMENT_3D('',#20105,#11144,#11145);
#9659=AXIS2_PLACEMENT_3D('',#20107,#11147,#11148);
#9660=AXIS2_PLACEMENT_3D('',#20123,#11151,#11152);
#9661=AXIS2_PLACEMENT_3D('',#20140,#11153,#11154);
#9662=AXIS2_PLACEMENT_3D('',#20141,#11155,#11156);
#9663=AXIS2_PLACEMENT_3D('',#20142,#11157,#11158);
#9664=AXIS2_PLACEMENT_3D('',#20146,#11162,#11163);
#9665=AXIS2_PLACEMENT_3D('',#20147,#11164,#11165);
#9666=AXIS2_PLACEMENT_3D('',#20148,#11166,#11167);
#9667=AXIS2_PLACEMENT_3D('',#20149,#11168,#11169);
#9668=AXIS2_PLACEMENT_3D('',#20150,#11170,#11171);
#9669=AXIS2_PLACEMENT_3D('',#20152,#11172,#11173);
#9670=AXIS2_PLACEMENT_3D('',#20165,#11180,#11181);
#9671=AXIS2_PLACEMENT_3D('',#20168,#11183,#11184);
#9672=AXIS2_PLACEMENT_3D('',#20169,#11185,#11186);
#9673=AXIS2_PLACEMENT_3D('',#20171,#11187,#11188);
#9674=AXIS2_PLACEMENT_3D('',#20174,#11190,#11191);
#9675=AXIS2_PLACEMENT_3D('',#20175,#11192,#11193);
#9676=AXIS2_PLACEMENT_3D('',#20176,#11194,#11195);
#9677=AXIS2_PLACEMENT_3D('',#20279,#11196,#11197);
#9678=AXIS2_PLACEMENT_3D('',#20281,#11198,#11199);
#9679=AXIS2_PLACEMENT_3D('',#20282,#11200,#11201);
#9680=AXIS2_PLACEMENT_3D('',#20284,#11203,#11204);
#9681=AXIS2_PLACEMENT_3D('',#20290,#11208,#11209);
#9682=AXIS2_PLACEMENT_3D('',#20294,#11212,#11213);
#9683=AXIS2_PLACEMENT_3D('',#20298,#11216,#11217);
#9684=AXIS2_PLACEMENT_3D('',#20302,#11220,#11221);
#9685=AXIS2_PLACEMENT_3D('',#20306,#11224,#11225);
#9686=AXIS2_PLACEMENT_3D('',#20308,#11227,#11228);
#9687=AXIS2_PLACEMENT_3D('',#20316,#11229,#11230);
#9688=AXIS2_PLACEMENT_3D('',#20399,#11232,#11233);
#9689=AXIS2_PLACEMENT_3D('',#23024,#11241,#11242);
#9690=AXIS2_PLACEMENT_3D('',#23042,#11245,#11246);
#9691=AXIS2_PLACEMENT_3D('',#23059,#11247,#11248);
#9692=AXIS2_PLACEMENT_3D('',#23446,#11250,#11251);
#9693=AXIS2_PLACEMENT_3D('',#25137,#11257,#11258);
#9694=AXIS2_PLACEMENT_3D('',#25138,#11259,#11260);
#9695=AXIS2_PLACEMENT_3D('',#25139,#11261,#11262);
#9696=AXIS2_PLACEMENT_3D('',#25141,#11263,#11264);
#9697=AXIS2_PLACEMENT_3D('',#25143,#11265,#11266);
#9698=AXIS2_PLACEMENT_3D('',#25144,#11267,#11268);
#9699=AXIS2_PLACEMENT_3D('',#25147,#11270,#11271);
#9700=AXIS2_PLACEMENT_3D('',#25148,#11272,#11273);
#9701=AXIS2_PLACEMENT_3D('',#25150,#11274,#11275);
#9702=AXIS2_PLACEMENT_3D('',#25151,#11276,#11277);
#9703=AXIS2_PLACEMENT_3D('',#25152,#11278,#11279);
#9704=AXIS2_PLACEMENT_3D('',#25153,#11280,#11281);
#9705=AXIS2_PLACEMENT_3D('',#25154,#11282,#11283);
#9706=AXIS2_PLACEMENT_3D('',#25175,#11285,#11286);
#9707=AXIS2_PLACEMENT_3D('',#25176,#11287,#11288);
#9708=AXIS2_PLACEMENT_3D('',#25179,#11289,#11290);
#9709=AXIS2_PLACEMENT_3D('',#25199,#11291,#11292);
#9710=AXIS2_PLACEMENT_3D('',#25203,#11294,#11295);
#9711=AXIS2_PLACEMENT_3D('',#26199,#11299,#11300);
#9712=AXIS2_PLACEMENT_3D('',#28764,#11308,#11309);
#9713=AXIS2_PLACEMENT_3D('',#28766,#11310,#11311);
#9714=AXIS2_PLACEMENT_3D('',#28767,#11312,#11313);
#9715=AXIS2_PLACEMENT_3D('',#28769,#11314,#11315);
#9716=AXIS2_PLACEMENT_3D('',#28770,#11316,#11317);
#9717=AXIS2_PLACEMENT_3D('',#28771,#11318,#11319);
#9718=AXIS2_PLACEMENT_3D('',#28773,#11321,#11322);
#9719=AXIS2_PLACEMENT_3D('',#28920,#11323,#11324);
#9720=AXIS2_PLACEMENT_3D('',#28922,#11325,#11326);
#9721=AXIS2_PLACEMENT_3D('',#28923,#11327,#11328);
#9722=AXIS2_PLACEMENT_3D('',#28927,#11330,#11331);
#9723=AXIS2_PLACEMENT_3D('',#28928,#11332,#11333);
#9724=AXIS2_PLACEMENT_3D('',#28986,#11334,#11335);
#9725=AXIS2_PLACEMENT_3D('',#29009,#11336,#11337);
#9726=AXIS2_PLACEMENT_3D('',#29014,#11338,#11339);
#9727=AXIS2_PLACEMENT_3D('',#29037,#11340,#11341);
#9728=AXIS2_PLACEMENT_3D('',#29088,#11342,#11343);
#9729=AXIS2_PLACEMENT_3D('',#29111,#11344,#11345);
#9730=AXIS2_PLACEMENT_3D('',#29134,#11346,#11347);
#9731=AXIS2_PLACEMENT_3D('',#29155,#11348,#11349);
#9732=AXIS2_PLACEMENT_3D('',#29161,#11353,#11354);
#9733=AXIS2_PLACEMENT_3D('',#29163,#11355,#11356);
#9734=AXIS2_PLACEMENT_3D('',#29165,#11358,#11359);
#9735=AXIS2_PLACEMENT_3D('',#29170,#11361,#11362);
#9736=AXIS2_PLACEMENT_3D('',#29174,#11364,#11365);
#9737=AXIS2_PLACEMENT_3D('',#29178,#11367,#11368);
#9738=AXIS2_PLACEMENT_3D('',#29181,#11370,#11371);
#9739=AXIS2_PLACEMENT_3D('',#29185,#11373,#11374);
#9740=AXIS2_PLACEMENT_3D('',#29189,#11376,#11377);
#9741=AXIS2_PLACEMENT_3D('',#29193,#11379,#11380);
#9742=AXIS2_PLACEMENT_3D('',#29197,#11382,#11383);
#9743=AXIS2_PLACEMENT_3D('',#29201,#11385,#11386);
#9744=AXIS2_PLACEMENT_3D('',#29205,#11388,#11389);
#9745=AXIS2_PLACEMENT_3D('',#29208,#11391,#11392);
#9746=AXIS2_PLACEMENT_3D('',#29209,#11393,#11394);
#9747=AXIS2_PLACEMENT_3D('',#29214,#11398,#11399);
#9748=AXIS2_PLACEMENT_3D('',#29219,#11402,#11403);
#9749=AXIS2_PLACEMENT_3D('',#29220,#11404,#11405);
#9750=AXIS2_PLACEMENT_3D('',#29225,#11408,#11409);
#9751=AXIS2_PLACEMENT_3D('',#29226,#11410,#11411);
#9752=AXIS2_PLACEMENT_3D('',#29231,#11414,#11415);
#9753=AXIS2_PLACEMENT_3D('',#29232,#11416,#11417);
#9754=AXIS2_PLACEMENT_3D('',#29235,#11419,#11420);
#9755=AXIS2_PLACEMENT_3D('',#29236,#11421,#11422);
#9756=AXIS2_PLACEMENT_3D('',#29239,#11425,#11426);
#9757=AXIS2_PLACEMENT_3D('',#29241,#11428,#11429);
#9758=AXIS2_PLACEMENT_3D('',#29243,#11431,#11432);
#9759=AXIS2_PLACEMENT_3D('',#29244,#11433,#11434);
#9760=AXIS2_PLACEMENT_3D('',#29247,#11437,#11438);
#9761=AXIS2_PLACEMENT_3D('',#29249,#11440,#11441);
#9762=AXIS2_PLACEMENT_3D('',#29251,#11443,#11444);
#9763=AXIS2_PLACEMENT_3D('',#29252,#11445,#11446);
#9764=AXIS2_PLACEMENT_3D('',#29254,#11448,#11449);
#9765=AXIS2_PLACEMENT_3D('',#29256,#11451,#11452);
#9766=AXIS2_PLACEMENT_3D('',#29258,#11454,#11455);
#9767=AXIS2_PLACEMENT_3D('',#29260,#11457,#11458);
#9768=AXIS2_PLACEMENT_3D('',#29262,#11460,#11461);
#9769=AXIS2_PLACEMENT_3D('',#29264,#11463,#11464);
#9770=AXIS2_PLACEMENT_3D('',#29266,#11466,#11467);
#9771=AXIS2_PLACEMENT_3D('',#29268,#11469,#11470);
#9772=AXIS2_PLACEMENT_3D('',#29270,#11472,#11473);
#9773=AXIS2_PLACEMENT_3D('',#29271,#11474,#11475);
#9774=AXIS2_PLACEMENT_3D('',#29273,#11477,#11478);
#9775=AXIS2_PLACEMENT_3D('',#29275,#11480,#11481);
#9776=AXIS2_PLACEMENT_3D('',#29276,#11482,#11483);
#9777=AXIS2_PLACEMENT_3D('',#29277,#11484,#11485);
#9778=AXIS2_PLACEMENT_3D('',#29362,#11489,#11490);
#9779=AXIS2_PLACEMENT_3D('',#29378,#11491,#11492);
#9780=AXIS2_PLACEMENT_3D('',#29386,#11493,#11494);
#9781=AXIS2_PLACEMENT_3D('',#29390,#11496,#11497);
#9782=AXIS2_PLACEMENT_3D('',#29391,#11498,#11499);
#9783=AXIS2_PLACEMENT_3D('',#29392,#11500,#11501);
#9784=AXIS2_PLACEMENT_3D('',#29397,#11503,#11504);
#9785=AXIS2_PLACEMENT_3D('',#29398,#11505,#11506);
#9786=AXIS2_PLACEMENT_3D('',#29399,#11507,#11508);
#9787=AXIS2_PLACEMENT_3D('',#29404,#11510,#11511);
#9788=AXIS2_PLACEMENT_3D('',#29405,#11512,#11513);
#9789=AXIS2_PLACEMENT_3D('',#29406,#11514,#11515);
#9790=AXIS2_PLACEMENT_3D('',#29408,#11516,#11517);
#9791=AXIS2_PLACEMENT_3D('',#29409,#11518,#11519);
#9792=AXIS2_PLACEMENT_3D('',#29410,#11520,#11521);
#9793=AXIS2_PLACEMENT_3D('',#29415,#11523,#11524);
#9794=AXIS2_PLACEMENT_3D('',#29416,#11525,#11526);
#9795=AXIS2_PLACEMENT_3D('',#29417,#11527,#11528);
#9796=AXIS2_PLACEMENT_3D('',#29419,#11529,#11530);
#9797=AXIS2_PLACEMENT_3D('',#29422,#11532,#11533);
#9798=AXIS2_PLACEMENT_3D('',#29515,#11534,#11535);
#9799=AXIS2_PLACEMENT_3D('',#29516,#11536,#11537);
#9800=AXIS2_PLACEMENT_3D('',#29518,#11538,#11539);
#9801=AXIS2_PLACEMENT_3D('',#29520,#11540,#11541);
#9802=AXIS2_PLACEMENT_3D('',#29521,#11542,#11543);
#9803=AXIS2_PLACEMENT_3D('',#29622,#11544,#11545);
#9804=AXIS2_PLACEMENT_3D('',#29623,#11546,#11547);
#9805=AXIS2_PLACEMENT_3D('',#29625,#11548,#11549);
#9806=AXIS2_PLACEMENT_3D('',#29627,#11550,#11551);
#9807=AXIS2_PLACEMENT_3D('',#29628,#11552,#11553);
#9808=AXIS2_PLACEMENT_3D('',#29666,#11554,#11555);
#9809=AXIS2_PLACEMENT_3D('',#29667,#11556,#11557);
#9810=AXIS2_PLACEMENT_3D('',#29701,#11558,#11559);
#9811=AXIS2_PLACEMENT_3D('',#29703,#11560,#11561);
#9812=AXIS2_PLACEMENT_3D('',#29738,#11562,#11563);
#9813=AXIS2_PLACEMENT_3D('',#29799,#11566,#11567);
#9814=AXIS2_PLACEMENT_3D('',#29801,#11568,#11569);
#9815=AXIS2_PLACEMENT_3D('',#29934,#11570,#11571);
#9816=AXIS2_PLACEMENT_3D('',#29941,#11572,#11573);
#9817=AXIS2_PLACEMENT_3D('',#30123,#11574,#11575);
#9818=AXIS2_PLACEMENT_3D('',#30152,#11576,#11577);
#9819=AXIS2_PLACEMENT_3D('',#30216,#11578,#11579);
#9820=AXIS2_PLACEMENT_3D('',#30333,#11580,#11581);
#9821=AXIS2_PLACEMENT_3D('',#30335,#11582,#11583);
#9822=AXIS2_PLACEMENT_3D('',#30406,#11584,#11585);
#9823=AXIS2_PLACEMENT_3D('',#30448,#11586,#11587);
#9824=AXIS2_PLACEMENT_3D('',#30450,#11588,#11589);
#9825=AXIS2_PLACEMENT_3D('',#30666,#11590,#11591);
#9826=AXIS2_PLACEMENT_3D('',#30708,#11592,#11593);
#9827=AXIS2_PLACEMENT_3D('',#30719,#11594,#11595);
#9828=AXIS2_PLACEMENT_3D('',#30791,#11596,#11597);
#9829=AXIS2_PLACEMENT_3D('',#30919,#11598,#11599);
#9830=AXIS2_PLACEMENT_3D('',#30992,#11600,#11601);
#9831=AXIS2_PLACEMENT_3D('',#31060,#11602,#11603);
#9832=AXIS2_PLACEMENT_3D('',#31061,#11604,#11605);
#9833=AXIS2_PLACEMENT_3D('',#31063,#11606,#11607);
#9834=AXIS2_PLACEMENT_3D('',#31064,#11608,#11609);
#9835=AXIS2_PLACEMENT_3D('',#31102,#11610,#11611);
#9836=AXIS2_PLACEMENT_3D('',#31103,#11612,#11613);
#9837=AXIS2_PLACEMENT_3D('',#31137,#11614,#11615);
#9838=AXIS2_PLACEMENT_3D('',#31138,#11616,#11617);
#9839=AXIS2_PLACEMENT_3D('',#31237,#11618,#11619);
#9840=AXIS2_PLACEMENT_3D('',#31238,#11620,#11621);
#9841=AXIS2_PLACEMENT_3D('',#31325,#11623,#11624);
#9842=AXIS2_PLACEMENT_3D('',#31367,#11625,#11626);
#9843=AXIS2_PLACEMENT_3D('',#31401,#11627,#11628);
#9844=AXIS2_PLACEMENT_3D('',#31402,#11629,#11630);
#9845=AXIS2_PLACEMENT_3D('',#31452,#11631,#11632);
#9846=AXIS2_PLACEMENT_3D('',#31453,#11633,#11634);
#9847=AXIS2_PLACEMENT_3D('',#31454,#11635,#11636);
#9848=AXIS2_PLACEMENT_3D('',#31455,#11637,#11638);
#9849=AXIS2_PLACEMENT_3D('',#31457,#11639,#11640);
#9850=AXIS2_PLACEMENT_3D('',#31459,#11641,#11642);
#9851=AXIS2_PLACEMENT_3D('',#31524,#11643,#11644);
#9852=AXIS2_PLACEMENT_3D('',#31525,#11645,#11646);
#9853=AXIS2_PLACEMENT_3D('',#31526,#11647,#11648);
#9854=AXIS2_PLACEMENT_3D('',#31568,#11649,#11650);
#9855=AXIS2_PLACEMENT_3D('',#31569,#11651,#11652);
#9856=AXIS2_PLACEMENT_3D('',#31610,#11653,#11654);
#9857=AXIS2_PLACEMENT_3D('',#31611,#11655,#11656);
#9858=AXIS2_PLACEMENT_3D('',#31713,#11657,#11658);
#9859=AXIS2_PLACEMENT_3D('',#31746,#11659,#11660);
#9860=AXIS2_PLACEMENT_3D('',#31779,#11661,#11662);
#9861=AXIS2_PLACEMENT_3D('',#31843,#11663,#11664);
#9862=AXIS2_PLACEMENT_3D('',#31888,#11665,#11666);
#9863=AXIS2_PLACEMENT_3D('',#31953,#11667,#11668);
#9864=AXIS2_PLACEMENT_3D('',#31954,#11669,#11670);
#9865=AXIS2_PLACEMENT_3D('',#31955,#11671,#11672);
#9866=AXIS2_PLACEMENT_3D('',#31957,#11673,#11674);
#9867=AXIS2_PLACEMENT_3D('',#31958,#11675,#11676);
#9868=AXIS2_PLACEMENT_3D('',#31959,#11677,#11678);
#9869=AXIS2_PLACEMENT_3D('',#31960,#11679,#11680);
#9870=AXIS2_PLACEMENT_3D('',#31990,#11681,#11682);
#9871=AXIS2_PLACEMENT_3D('',#31991,#11683,#11684);
#9872=AXIS2_PLACEMENT_3D('',#32036,#11685,#11686);
#9873=AXIS2_PLACEMENT_3D('',#32037,#11687,#11688);
#9874=AXIS2_PLACEMENT_3D('',#32038,#11689,#11690);
#9875=AXIS2_PLACEMENT_3D('',#32039,#11691,#11692);
#9876=AXIS2_PLACEMENT_3D('',#32089,#11693,#11694);
#9877=AXIS2_PLACEMENT_3D('',#32091,#11695,#11696);
#9878=AXIS2_PLACEMENT_3D('',#32092,#11697,#11698);
#9879=AXIS2_PLACEMENT_3D('',#32093,#11699,#11700);
#9880=AXIS2_PLACEMENT_3D('',#32094,#11701,#11702);
#9881=AXIS2_PLACEMENT_3D('',#32159,#11703,#11704);
#9882=AXIS2_PLACEMENT_3D('',#32161,#11705,#11706);
#9883=AXIS2_PLACEMENT_3D('',#32402,#11710,#11711);
#9884=AXIS2_PLACEMENT_3D('',#32403,#11712,#11713);
#9885=AXIS2_PLACEMENT_3D('',#32440,#11716,#11717);
#9886=AXIS2_PLACEMENT_3D('',#32442,#11719,#11720);
#9887=AXIS2_PLACEMENT_3D('',#32746,#11722,#11723);
#9888=AXIS2_PLACEMENT_3D('',#32747,#11724,#11725);
#9889=AXIS2_PLACEMENT_3D('',#32833,#11727,#11728);
#9890=AXIS2_PLACEMENT_3D('',#32834,#11729,#11730);
#9891=AXIS2_PLACEMENT_3D('',#32901,#11732,#11733);
#9892=AXIS2_PLACEMENT_3D('',#32902,#11734,#11735);
#9893=AXIS2_PLACEMENT_3D('',#32938,#11738,#11739);
#9894=AXIS2_PLACEMENT_3D('',#33004,#11740,#11741);
#9895=AXIS2_PLACEMENT_3D('',#33005,#11742,#11743);
#9896=AXIS2_PLACEMENT_3D('',#33069,#11745,#11746);
#9897=AXIS2_PLACEMENT_3D('',#33392,#11747,#11748);
#9898=AXIS2_PLACEMENT_3D('',#33393,#11749,#11750);
#9899=AXIS2_PLACEMENT_3D('',#33642,#11752,#11753);
#9900=AXIS2_PLACEMENT_3D('',#33644,#11754,#11755);
#9901=AXIS2_PLACEMENT_3D('',#33645,#11756,#11757);
#9902=AXIS2_PLACEMENT_3D('',#33646,#11758,#11759);
#9903=AXIS2_PLACEMENT_3D('',#33647,#11760,#11761);
#9904=AXIS2_PLACEMENT_3D('',#33648,#11762,#11763);
#9905=AXIS2_PLACEMENT_3D('',#33651,#11764,#11765);
#9906=AXIS2_PLACEMENT_3D('',#33653,#11767,#11768);
#9907=AXIS2_PLACEMENT_3D('',#33654,#11769,#11770);
#9908=AXIS2_PLACEMENT_3D('',#33657,#11772,#11773);
#9909=AXIS2_PLACEMENT_3D('',#33658,#11774,#11775);
#9910=AXIS2_PLACEMENT_3D('',#33660,#11776,#11777);
#9911=AXIS2_PLACEMENT_3D('',#33661,#11778,#11779);
#9912=AXIS2_PLACEMENT_3D('',#33664,#11781,#11782);
#9913=AXIS2_PLACEMENT_3D('',#33665,#11783,#11784);
#9914=AXIS2_PLACEMENT_3D('',#33794,#11785,#11786);
#9915=AXIS2_PLACEMENT_3D('',#33859,#11787,#11788);
#9916=AXIS2_PLACEMENT_3D('',#34040,#11789,#11790);
#9917=AXIS2_PLACEMENT_3D('',#34165,#11791,#11792);
#9918=AXIS2_PLACEMENT_3D('',#34460,#11793,#11794);
#9919=AXIS2_PLACEMENT_3D('',#34493,#11795,#11796);
#9920=AXIS2_PLACEMENT_3D('',#34526,#11797,#11798);
#9921=AXIS2_PLACEMENT_3D('',#34527,#11799,#11800);
#9922=AXIS2_PLACEMENT_3D('',#34528,#11801,#11802);
#9923=AXIS2_PLACEMENT_3D('',#34530,#11803,#11804);
#9924=AXIS2_PLACEMENT_3D('',#34533,#11805,#11806);
#9925=AXIS2_PLACEMENT_3D('',#34537,#11808,#11809);
#9926=AXIS2_PLACEMENT_3D('',#34541,#11811,#11812);
#9927=AXIS2_PLACEMENT_3D('',#34545,#11814,#11815);
#9928=AXIS2_PLACEMENT_3D('',#34549,#11817,#11818);
#9929=AXIS2_PLACEMENT_3D('',#34553,#11820,#11821);
#9930=AXIS2_PLACEMENT_3D('',#34557,#11823,#11824);
#9931=AXIS2_PLACEMENT_3D('',#34561,#11826,#11827);
#9932=AXIS2_PLACEMENT_3D('',#34565,#11829,#11830);
#9933=AXIS2_PLACEMENT_3D('',#34569,#11832,#11833);
#9934=AXIS2_PLACEMENT_3D('',#34573,#11835,#11836);
#9935=AXIS2_PLACEMENT_3D('',#34577,#11838,#11839);
#9936=AXIS2_PLACEMENT_3D('',#34579,#11841,#11842);
#9937=AXIS2_PLACEMENT_3D('',#34582,#11844,#11845);
#9938=AXIS2_PLACEMENT_3D('',#34583,#11846,#11847);
#9939=AXIS2_PLACEMENT_3D('',#34586,#11849,#11850);
#9940=AXIS2_PLACEMENT_3D('',#34587,#11851,#11852);
#9941=AXIS2_PLACEMENT_3D('',#34589,#11853,#11854);
#9942=AXIS2_PLACEMENT_3D('',#34591,#11855,#11856);
#9943=AXIS2_PLACEMENT_3D('',#34592,#11857,#11858);
#9944=AXIS2_PLACEMENT_3D('',#34593,#11859,#11860);
#9945=AXIS2_PLACEMENT_3D('',#34601,#11861,#11862);
#9946=AXIS2_PLACEMENT_3D('',#34603,#11864,#11865);
#9947=AXIS2_PLACEMENT_3D('',#34604,#11866,#11867);
#9948=AXIS2_PLACEMENT_3D('',#38869,#11879,#11880);
#9949=AXIS2_PLACEMENT_3D('',#39800,#11886,#11887);
#9950=AXIS2_PLACEMENT_3D('',#39801,#11888,#11889);
#9951=AXIS2_PLACEMENT_3D('',#39805,#11891,#11892);
#9952=AXIS2_PLACEMENT_3D('',#39807,#11894,#11895);
#9953=AXIS2_PLACEMENT_3D('',#39811,#11898,#11899);
#9954=AXIS2_PLACEMENT_3D('',#39816,#11901,#11902);
#9955=AXIS2_PLACEMENT_3D('',#39820,#11904,#11905);
#9956=AXIS2_PLACEMENT_3D('',#39823,#11907,#11908);
#9957=AXIS2_PLACEMENT_3D('',#39827,#11910,#11911);
#9958=AXIS2_PLACEMENT_3D('',#39831,#11913,#11914);
#9959=AXIS2_PLACEMENT_3D('',#39835,#11916,#11917);
#9960=AXIS2_PLACEMENT_3D('',#39839,#11919,#11920);
#9961=AXIS2_PLACEMENT_3D('',#39843,#11922,#11923);
#9962=AXIS2_PLACEMENT_3D('',#39847,#11925,#11926);
#9963=AXIS2_PLACEMENT_3D('',#39851,#11928,#11929);
#9964=AXIS2_PLACEMENT_3D('',#39854,#11931,#11932);
#9965=AXIS2_PLACEMENT_3D('',#39855,#11933,#11934);
#9966=AXIS2_PLACEMENT_3D('',#39858,#11937,#11938);
#9967=AXIS2_PLACEMENT_3D('',#39860,#11940,#11941);
#9968=AXIS2_PLACEMENT_3D('',#39862,#11943,#11944);
#9969=AXIS2_PLACEMENT_3D('',#39864,#11946,#11947);
#9970=AXIS2_PLACEMENT_3D('',#39866,#11949,#11950);
#9971=AXIS2_PLACEMENT_3D('',#39868,#11952,#11953);
#9972=AXIS2_PLACEMENT_3D('',#39870,#11955,#11956);
#9973=AXIS2_PLACEMENT_3D('',#39872,#11958,#11959);
#9974=AXIS2_PLACEMENT_3D('',#39874,#11961,#11962);
#9975=AXIS2_PLACEMENT_3D('',#39876,#11964,#11965);
#9976=AXIS2_PLACEMENT_3D('',#39878,#11967,#11968);
#9977=AXIS2_PLACEMENT_3D('',#39880,#11970,#11971);
#9978=AXIS2_PLACEMENT_3D('',#39882,#11973,#11974);
#9979=AXIS2_PLACEMENT_3D('',#39884,#11976,#11977);
#9980=AXIS2_PLACEMENT_3D('',#39886,#11979,#11980);
#9981=AXIS2_PLACEMENT_3D('',#39888,#11982,#11983);
#9982=AXIS2_PLACEMENT_3D('',#39890,#11985,#11986);
#9983=AXIS2_PLACEMENT_3D('',#39891,#11987,#11988);
#9984=AXIS2_PLACEMENT_3D('',#39893,#11990,#11991);
#9985=AXIS2_PLACEMENT_3D('',#39895,#11993,#11994);
#9986=AXIS2_PLACEMENT_3D('',#39897,#11996,#11997);
#9987=AXIS2_PLACEMENT_3D('',#39898,#11998,#11999);
#9988=AXIS2_PLACEMENT_3D('',#39899,#12000,#12001);
#9989=AXIS2_PLACEMENT_3D('',#39921,#12006,#12007);
#9990=AXIS2_PLACEMENT_3D('',#39923,#12008,#12009);
#9991=AXIS2_PLACEMENT_3D('',#39924,#12010,#12011);
#9992=AXIS2_PLACEMENT_3D('',#39927,#12012,#12013);
#9993=AXIS2_PLACEMENT_3D('',#39928,#12014,#12015);
#9994=AXIS2_PLACEMENT_3D('',#39929,#12016,#12017);
#9995=AXIS2_PLACEMENT_3D('',#39930,#12018,#12019);
#9996=AXIS2_PLACEMENT_3D('',#39932,#12020,#12021);
#9997=AXIS2_PLACEMENT_3D('',#39934,#12023,#12024);
#9998=AXIS2_PLACEMENT_3D('',#39936,#12025,#12026);
#9999=AXIS2_PLACEMENT_3D('',#39937,#12027,#12028);
#10000=AXIS2_PLACEMENT_3D('',#39940,#12029,#12030);
#10001=AXIS2_PLACEMENT_3D('',#39941,#12031,#12032);
#10002=AXIS2_PLACEMENT_3D('',#39943,#12034,#12035);
#10003=AXIS2_PLACEMENT_3D('',#39945,#12036,#12037);
#10004=AXIS2_PLACEMENT_3D('',#40065,#12040,#12041);
#10005=AXIS2_PLACEMENT_3D('',#43371,#12051,#12052);
#10006=AXIS2_PLACEMENT_3D('',#43372,#12053,#12054);
#10007=AXIS2_PLACEMENT_3D('',#43374,#12055,#12056);
#10008=AXIS2_PLACEMENT_3D('',#43375,#12057,#12058);
#10009=AXIS2_PLACEMENT_3D('',#43378,#12060,#12061);
#10010=AXIS2_PLACEMENT_3D('',#43426,#12062,#12063);
#10011=AXIS2_PLACEMENT_3D('',#43428,#12064,#12065);
#10012=AXIS2_PLACEMENT_3D('',#43429,#12066,#12067);
#10013=AXIS2_PLACEMENT_3D('',#43432,#12069,#12070);
#10014=AXIS2_PLACEMENT_3D('',#43433,#12071,#12072);
#10015=AXIS2_PLACEMENT_3D('',#43636,#12076,#12077);
#10016=AXIS2_PLACEMENT_3D('',#43638,#12078,#12079);
#10017=AXIS2_PLACEMENT_3D('',#43642,#12081,#12082);
#10018=AXIS2_PLACEMENT_3D('',#43646,#12084,#12085);
#10019=AXIS2_PLACEMENT_3D('',#43648,#12086,#12087);
#10020=AXIS2_PLACEMENT_3D('',#43651,#12089,#12090);
#10021=AXIS2_PLACEMENT_3D('',#43652,#12091,#12092);
#10022=AXIS2_PLACEMENT_3D('',#43654,#12093,#12094);
#10023=AXIS2_PLACEMENT_3D('',#43656,#12096,#12097);
#10024=AXIS2_PLACEMENT_3D('',#43661,#12099,#12100);
#10025=AXIS2_PLACEMENT_3D('',#43664,#12102,#12103);
#10026=AXIS2_PLACEMENT_3D('',#43665,#12104,#12105);
#10027=AXIS2_PLACEMENT_3D('',#43667,#12106,#12107);
#10028=AXIS2_PLACEMENT_3D('',#43822,#12109,#12110);
#10029=AXIS2_PLACEMENT_3D('',#43824,#12111,#12112);
#10030=AXIS2_PLACEMENT_3D('',#43839,#12113,#12114);
#10031=AXIS2_PLACEMENT_3D('',#43841,#12115,#12116);
#10032=AXIS2_PLACEMENT_3D('',#43842,#12117,#12118);
#10033=AXIS2_PLACEMENT_3D('',#43905,#12119,#12120);
#10034=AXIS2_PLACEMENT_3D('',#44049,#12121,#12122);
#10035=AXIS2_PLACEMENT_3D('',#44052,#12123,#12124);
#10036=AXIS2_PLACEMENT_3D('',#44055,#12127,#12128);
#10037=AXIS2_PLACEMENT_3D('',#44056,#12129,#12130);
#10038=AXIS2_PLACEMENT_3D('',#44057,#12131,#12132);
#10039=AXIS2_PLACEMENT_3D('',#44058,#12133,#12134);
#10040=AXIS2_PLACEMENT_3D('',#44061,#12136,#12137);
#10041=AXIS2_PLACEMENT_3D('',#44062,#12138,#12139);
#10042=AXIS2_PLACEMENT_3D('',#44066,#12142,#12143);
#10043=AXIS2_PLACEMENT_3D('',#44067,#12144,#12145);
#10044=AXIS2_PLACEMENT_3D('',#44068,#12146,#12147);
#10045=AXIS2_PLACEMENT_3D('',#44069,#12148,#12149);
#10046=AXIS2_PLACEMENT_3D('',#44070,#12150,#12151);
#10047=AXIS2_PLACEMENT_3D('',#44072,#12152,#12153);
#10048=AXIS2_PLACEMENT_3D('',#44074,#12155,#12156);
#10049=AXIS2_PLACEMENT_3D('',#44075,#12157,#12158);
#10050=AXIS2_PLACEMENT_3D('',#44076,#12159,#12160);
#10051=AXIS2_PLACEMENT_3D('',#44079,#12162,#12163);
#10052=AXIS2_PLACEMENT_3D('',#44080,#12164,#12165);
#10053=AXIS2_PLACEMENT_3D('',#44082,#12167,#12168);
#10054=AXIS2_PLACEMENT_3D('',#44084,#12169,#12170);
#10055=AXIS2_PLACEMENT_3D('',#44086,#12172,#12173);
#10056=AXIS2_PLACEMENT_3D('',#44087,#12174,#12175);
#10057=AXIS2_PLACEMENT_3D('',#44088,#12176,#12177);
#10058=AXIS2_PLACEMENT_3D('',#44090,#12178,#12179);
#10059=AXIS2_PLACEMENT_3D('',#44091,#12180,#12181);
#10060=AXIS2_PLACEMENT_3D('',#44092,#12182,#12183);
#10061=AXIS2_PLACEMENT_3D('',#44094,#12184,#12185);
#10062=AXIS2_PLACEMENT_3D('',#44098,#12187,#12188);
#10063=AXIS2_PLACEMENT_3D('',#44100,#12190,#12191);
#10064=AXIS2_PLACEMENT_3D('',#44101,#12192,#12193);
#10065=AXIS2_PLACEMENT_3D('',#44102,#12194,#12195);
#10066=AXIS2_PLACEMENT_3D('',#44105,#12197,#12198);
#10067=AXIS2_PLACEMENT_3D('',#44106,#12199,#12200);
#10068=AXIS2_PLACEMENT_3D('',#44369,#12203,#12204);
#10069=AXIS2_PLACEMENT_3D('',#44371,#12205,#12206);
#10070=AXIS2_PLACEMENT_3D('',#44496,#12207,#12208);
#10071=AXIS2_PLACEMENT_3D('',#44497,#12209,#12210);
#10072=AXIS2_PLACEMENT_3D('',#44500,#12212,#12213);
#10073=AXIS2_PLACEMENT_3D('',#44540,#12214,#12215);
#10074=AXIS2_PLACEMENT_3D('',#44541,#12216,#12217);
#10075=AXIS2_PLACEMENT_3D('',#44545,#12219,#12220);
#10076=AXIS2_PLACEMENT_3D('',#44797,#12222,#12223);
#10077=AXIS2_PLACEMENT_3D('',#44842,#12224,#12225);
#10078=AXIS2_PLACEMENT_3D('',#44915,#12226,#12227);
#10079=AXIS2_PLACEMENT_3D('',#44973,#12228,#12229);
#10080=AXIS2_PLACEMENT_3D('',#45113,#12230,#12231);
#10081=AXIS2_PLACEMENT_3D('',#45181,#12232,#12233);
#10082=AXIS2_PLACEMENT_3D('',#45183,#12234,#12235);
#10083=AXIS2_PLACEMENT_3D('',#45196,#12237,#12238);
#10084=AXIS2_PLACEMENT_3D('',#45197,#12239,#12240);
#10085=AXIS2_PLACEMENT_3D('',#45198,#12241,#12242);
#10086=AXIS2_PLACEMENT_3D('',#45199,#12243,#12244);
#10087=AXIS2_PLACEMENT_3D('',#45204,#12247,#12248);
#10088=AXIS2_PLACEMENT_3D('',#45207,#12250,#12251);
#10089=AXIS2_PLACEMENT_3D('',#45208,#12252,#12253);
#10090=AXIS2_PLACEMENT_3D('',#45210,#12254,#12255);
#10091=AXIS2_PLACEMENT_3D('',#45212,#12257,#12258);
#10092=AXIS2_PLACEMENT_3D('',#45214,#12259,#12260);
#10093=AXIS2_PLACEMENT_3D('',#45215,#12261,#12262);
#10094=AXIS2_PLACEMENT_3D('',#45217,#12263,#12264);
#10095=AXIS2_PLACEMENT_3D('',#45220,#12267,#12268);
#10096=AXIS2_PLACEMENT_3D('',#45223,#12269,#12270);
#10097=AXIS2_PLACEMENT_3D('',#45227,#12272,#12273);
#10098=AXIS2_PLACEMENT_3D('',#45231,#12275,#12276);
#10099=AXIS2_PLACEMENT_3D('',#45234,#12279,#12280);
#10100=AXIS2_PLACEMENT_3D('',#45237,#12283,#12284);
#10101=AXIS2_PLACEMENT_3D('',#45238,#12285,#12286);
#10102=AXIS2_PLACEMENT_3D('',#45242,#12289,#12290);
#10103=AXIS2_PLACEMENT_3D('',#45243,#12291,#12292);
#10104=AXIS2_PLACEMENT_3D('',#45440,#12293,#12294);
#10105=AXIS2_PLACEMENT_3D('',#45528,#12295,#12296);
#10106=AXIS2_PLACEMENT_3D('',#45529,#12297,#12298);
#10107=AXIS2_PLACEMENT_3D('',#45530,#12299,#12300);
#10108=AXIS2_PLACEMENT_3D('',#45535,#12304,#12305);
#10109=AXIS2_PLACEMENT_3D('',#45536,#12306,#12307);
#10110=AXIS2_PLACEMENT_3D('',#45646,#12309,#12310);
#10111=AXIS2_PLACEMENT_3D('',#45706,#12311,#12312);
#10112=AXIS2_PLACEMENT_3D('',#45707,#12313,#12314);
#10113=AXIS2_PLACEMENT_3D('',#45711,#12317,#12318);
#10114=AXIS2_PLACEMENT_3D('',#45712,#12319,#12320);
#10115=AXIS2_PLACEMENT_3D('',#45746,#12321,#12322);
#10116=AXIS2_PLACEMENT_3D('',#45747,#12323,#12324);
#10117=AXIS2_PLACEMENT_3D('',#45941,#12325,#12326);
#10118=AXIS2_PLACEMENT_3D('',#46030,#12327,#12328);
#10119=AXIS2_PLACEMENT_3D('',#46034,#12331,#12332);
#10120=AXIS2_PLACEMENT_3D('',#46035,#12333,#12334);
#10121=AXIS2_PLACEMENT_3D('',#46036,#12335,#12336);
#10122=AXIS2_PLACEMENT_3D('',#46037,#12337,#12338);
#10123=AXIS2_PLACEMENT_3D('',#46038,#12339,#12340);
#10124=AXIS2_PLACEMENT_3D('',#46039,#12341,#12342);
#10125=AXIS2_PLACEMENT_3D('',#46040,#12343,#12344);
#10126=AXIS2_PLACEMENT_3D('',#46041,#12345,#12346);
#10127=AXIS2_PLACEMENT_3D('',#46042,#12347,#12348);
#10128=AXIS2_PLACEMENT_3D('',#46043,#12349,#12350);
#10129=AXIS2_PLACEMENT_3D('',#46044,#12351,#12352);
#10130=AXIS2_PLACEMENT_3D('',#46045,#12353,#12354);
#10131=AXIS2_PLACEMENT_3D('',#46046,#12355,#12356);
#10132=AXIS2_PLACEMENT_3D('',#46047,#12357,#12358);
#10133=AXIS2_PLACEMENT_3D('',#46048,#12359,#12360);
#10134=AXIS2_PLACEMENT_3D('',#46050,#12361,#12362);
#10135=AXIS2_PLACEMENT_3D('',#46052,#12363,#12364);
#10136=AXIS2_PLACEMENT_3D('',#46053,#12365,#12366);
#10137=AXIS2_PLACEMENT_3D('',#46056,#12368,#12369);
#10138=AXIS2_PLACEMENT_3D('',#46057,#12370,#12371);
#10139=AXIS2_PLACEMENT_3D('',#46059,#12372,#12373);
#10140=AXIS2_PLACEMENT_3D('',#46060,#12374,#12375);
#10141=AXIS2_PLACEMENT_3D('',#46061,#12376,#12377);
#10142=AXIS2_PLACEMENT_3D('',#46062,#12378,#12379);
#10143=AXIS2_PLACEMENT_3D('',#46063,#12380,#12381);
#10144=AXIS2_PLACEMENT_3D('',#46202,#12382,#12383);
#10145=AXIS2_PLACEMENT_3D('',#46203,#12384,#12385);
#10146=AXIS2_PLACEMENT_3D('',#46205,#12386,#12387);
#10147=AXIS2_PLACEMENT_3D('',#46207,#12389,#12390);
#10148=AXIS2_PLACEMENT_3D('',#46209,#12391,#12392);
#10149=AXIS2_PLACEMENT_3D('',#46380,#12393,#12394);
#10150=AXIS2_PLACEMENT_3D('',#46383,#12395,#12396);
#10151=AXIS2_PLACEMENT_3D('',#46386,#12399,#12400);
#10152=AXIS2_PLACEMENT_3D('',#46390,#12402,#12403);
#10153=AXIS2_PLACEMENT_3D('',#46394,#12405,#12406);
#10154=AXIS2_PLACEMENT_3D('',#46398,#12408,#12409);
#10155=AXIS2_PLACEMENT_3D('',#46402,#12411,#12412);
#10156=AXIS2_PLACEMENT_3D('',#46406,#12414,#12415);
#10157=AXIS2_PLACEMENT_3D('',#46409,#12417,#12418);
#10158=AXIS2_PLACEMENT_3D('',#46410,#12419,#12420);
#10159=AXIS2_PLACEMENT_3D('',#46488,#12423,#12424);
#10160=AXIS2_PLACEMENT_3D('',#52059,#12431,#12432);
#10161=AXIS2_PLACEMENT_3D('',#52061,#12434,#12435);
#10162=AXIS2_PLACEMENT_3D('',#52063,#12437,#12438);
#10163=AXIS2_PLACEMENT_3D('',#52065,#12440,#12441);
#10164=AXIS2_PLACEMENT_3D('',#52067,#12443,#12444);
#10165=AXIS2_PLACEMENT_3D('',#52069,#12446,#12447);
#10166=AXIS2_PLACEMENT_3D('',#52071,#12449,#12450);
#10167=AXIS2_PLACEMENT_3D('',#52073,#12452,#12453);
#10168=AXIS2_PLACEMENT_3D('',#52075,#12455,#12456);
#10169=AXIS2_PLACEMENT_3D('',#52077,#12458,#12459);
#10170=AXIS2_PLACEMENT_3D('',#52079,#12461,#12462);
#10171=AXIS2_PLACEMENT_3D('',#52080,#12463,#12464);
#10172=AXIS2_PLACEMENT_3D('',#52081,#12465,#12466);
#10173=AXIS2_PLACEMENT_3D('',#52083,#12467,#12468);
#10174=AXIS2_PLACEMENT_3D('',#52084,#12469,#12470);
#10175=AXIS2_PLACEMENT_3D('',#52085,#12471,#12472);
#10176=AXIS2_PLACEMENT_3D('',#52086,#12473,#12474);
#10177=AXIS2_PLACEMENT_3D('',#52088,#12475,#12476);
#10178=AXIS2_PLACEMENT_3D('',#52090,#12477,#12478);
#10179=AXIS2_PLACEMENT_3D('',#52091,#12479,#12480);
#10180=AXIS2_PLACEMENT_3D('',#52094,#12482,#12483);
#10181=AXIS2_PLACEMENT_3D('',#52095,#12484,#12485);
#10182=AXIS2_PLACEMENT_3D('',#52097,#12486,#12487);
#10183=AXIS2_PLACEMENT_3D('',#52098,#12488,#12489);
#10184=AXIS2_PLACEMENT_3D('',#52100,#12491,#12492);
#10185=AXIS2_PLACEMENT_3D('',#52101,#12493,#12494);
#10186=AXIS2_PLACEMENT_3D('',#52103,#12495,#12496);
#10187=AXIS2_PLACEMENT_3D('',#52105,#12497,#12498);
#10188=AXIS2_PLACEMENT_3D('',#52106,#12499,#12500);
#10189=AXIS2_PLACEMENT_3D('',#52109,#12502,#12503);
#10190=AXIS2_PLACEMENT_3D('',#52110,#12504,#12505);
#10191=AXIS2_PLACEMENT_3D('',#52112,#12506,#12507);
#10192=AXIS2_PLACEMENT_3D('',#52113,#12508,#12509);
#10193=AXIS2_PLACEMENT_3D('',#52116,#12510,#12511);
#10194=AXIS2_PLACEMENT_3D('',#52118,#12513,#12514);
#10195=AXIS2_PLACEMENT_3D('',#52119,#12515,#12516);
#10196=AXIS2_PLACEMENT_3D('',#52121,#12517,#12518);
#10197=AXIS2_PLACEMENT_3D('',#52122,#12519,#12520);
#10198=AXIS2_PLACEMENT_3D('',#52123,#12521,#12522);
#10199=AXIS2_PLACEMENT_3D('',#52124,#12523,#12524);
#10200=AXIS2_PLACEMENT_3D('',#52125,#12525,#12526);
#10201=AXIS2_PLACEMENT_3D('',#52126,#12527,#12528);
#10202=AXIS2_PLACEMENT_3D('',#52127,#12529,#12530);
#10203=AXIS2_PLACEMENT_3D('',#52128,#12531,#12532);
#10204=AXIS2_PLACEMENT_3D('',#52129,#12533,#12534);
#10205=AXIS2_PLACEMENT_3D('',#52130,#12535,#12536);
#10206=AXIS2_PLACEMENT_3D('',#52131,#12537,#12538);
#10207=AXIS2_PLACEMENT_3D('',#52132,#12539,#12540);
#10208=AXIS2_PLACEMENT_3D('',#52133,#12541,#12542);
#10209=AXIS2_PLACEMENT_3D('',#52134,#12543,#12544);
#10210=DIRECTION('axis',(0.,0.,1.));
#10211=DIRECTION('refdir',(1.,0.,0.));
#10212=DIRECTION('axis',(0.,0.,1.));
#10213=DIRECTION('refdir',(1.,0.,0.));
#10214=DIRECTION('center_axis',(1.,0.,0.));
#10215=DIRECTION('ref_axis',(0.,0.,1.));
#10216=DIRECTION('',(-1.,0.,0.));
#10217=DIRECTION('',(-1.,0.,0.));
#10218=DIRECTION('center_axis',(1.,0.,0.));
#10219=DIRECTION('ref_axis',(0.,0.,1.));
#10220=DIRECTION('',(1.,0.,0.));
#10221=DIRECTION('center_axis',(1.,0.,0.));
#10222=DIRECTION('ref_axis',(0.,0.,1.));
#10223=DIRECTION('',(-1.,0.,0.));
#10224=DIRECTION('center_axis',(1.,0.,0.));
#10225=DIRECTION('ref_axis',(0.,0.,1.));
#10226=DIRECTION('',(-1.,0.,0.));
#10227=DIRECTION('center_axis',(1.,0.,0.));
#10228=DIRECTION('ref_axis',(0.,0.,1.));
#10229=DIRECTION('',(-1.,0.,0.));
#10230=DIRECTION('center_axis',(1.,0.,0.));
#10231=DIRECTION('ref_axis',(0.,0.,1.));
#10232=DIRECTION('',(-1.,0.,0.));
#10233=DIRECTION('center_axis',(0.,1.,0.));
#10234=DIRECTION('ref_axis',(0.,0.,1.));
#10235=DIRECTION('center_axis',(1.,0.,0.));
#10236=DIRECTION('ref_axis',(0.,0.,1.));
#10237=DIRECTION('',(-1.,0.,0.));
#10238=DIRECTION('center_axis',(1.,0.,0.));
#10239=DIRECTION('ref_axis',(0.,0.,-1.));
#10240=DIRECTION('',(1.,0.,0.));
#10241=DIRECTION('',(-0.364960948531691,0.,0.931022827887076));
#10242=DIRECTION('center_axis',(0.,1.,0.));
#10243=DIRECTION('ref_axis',(0.,0.,1.));
#10244=DIRECTION('',(-0.364960948531691,0.,-0.931022827887076));
#10245=DIRECTION('',(-1.,0.,0.));
#10246=DIRECTION('',(-1.,0.,0.));
#10247=DIRECTION('center_axis',(1.,0.,0.));
#10248=DIRECTION('ref_axis',(0.,0.,1.));
#10249=DIRECTION('center_axis',(-1.,0.,0.));
#10250=DIRECTION('ref_axis',(0.,-0.939692620785897,0.342020143325699));
#10251=DIRECTION('',(0.,0.,1.));
#10252=DIRECTION('center_axis',(1.,0.,0.));
#10253=DIRECTION('ref_axis',(0.,0.820913047490338,0.571053209832609));
#10254=DIRECTION('',(-1.,0.,0.));
#10255=DIRECTION('center_axis',(0.,-1.,0.));
#10256=DIRECTION('ref_axis',(0.,0.,1.));
#10257=DIRECTION('',(-0.500000000000004,0.750000000000006,-0.433012701892204));
#10258=DIRECTION('',(-0.500000000000004,-0.750000000000006,0.433012701892204));
#10259=DIRECTION('',(-1.,0.,0.));
#10260=DIRECTION('',(-1.,0.,0.));
#10261=DIRECTION('',(-0.500000000000004,-0.750000000000006,-0.433012701892204));
#10262=DIRECTION('',(-0.500000000000004,0.750000000000006,0.433012701892204));
#10263=DIRECTION('',(-0.500000000000017,-3.68592187288512E-14,-0.866025403784429));
#10264=DIRECTION('',(-0.500000000000017,2.10167360932807E-14,0.866025403784429));
#10265=DIRECTION('center_axis',(1.,0.,0.));
#10266=DIRECTION('ref_axis',(0.,-1.,0.));
#10267=DIRECTION('',(0.,0.866025403784429,-0.500000000000017));
#10268=DIRECTION('center_axis',(1.,0.,0.));
#10269=DIRECTION('ref_axis',(0.,0.766044443118957,0.642787609686564));
#10270=DIRECTION('center_axis',(0.,0.500000000000017,0.866025403784429));
#10271=DIRECTION('ref_axis',(0.,0.866025403784429,-0.500000000000017));
#10272=DIRECTION('',(1.,1.9378438248E-14,-1.9378438248E-14));
#10273=DIRECTION('center_axis',(1.,0.,0.));
#10274=DIRECTION('ref_axis',(0.,-1.,0.));
#10275=DIRECTION('',(-1.,0.,0.));
#10276=DIRECTION('center_axis',(-1.,0.,0.));
#10277=DIRECTION('ref_axis',(0.,-1.,0.));
#10278=DIRECTION('center_axis',(-1.,0.,0.));
#10279=DIRECTION('ref_axis',(0.,-1.,0.));
#10280=DIRECTION('center_axis',(-1.,0.,0.));
#10281=DIRECTION('ref_axis',(0.,-1.,0.));
#10282=DIRECTION('center_axis',(-1.,0.,0.));
#10283=DIRECTION('ref_axis',(0.,0.,-1.));
#10284=DIRECTION('center_axis',(-1.,0.,0.));
#10285=DIRECTION('ref_axis',(0.,0.,-1.));
#10286=DIRECTION('',(1.,0.,0.));
#10287=DIRECTION('center_axis',(-1.,0.,-6.12323399573677E-17));
#10288=DIRECTION('ref_axis',(0.,0.,-1.));
#10289=DIRECTION('center_axis',(0.,1.,-1.22464679914735E-16));
#10290=DIRECTION('ref_axis',(0.,1.22464679914735E-16,1.));
#10291=DIRECTION('axis',(0.,0.,1.));
#10292=DIRECTION('refdir',(1.,0.,0.));
#10293=DIRECTION('center_axis',(1.,0.,0.));
#10294=DIRECTION('ref_axis',(0.,-1.,0.));
#10295=DIRECTION('center_axis',(-1.,0.,0.));
#10296=DIRECTION('ref_axis',(0.,-0.522204744824901,-0.852820147793402));
#10297=DIRECTION('center_axis',(-1.,0.,0.));
#10298=DIRECTION('ref_axis',(0.,0.582193477502481,-0.813050278121574));
#10299=DIRECTION('center_axis',(-1.,0.,0.));
#10300=DIRECTION('ref_axis',(0.,0.47208694179479,-0.881551994715481));
#10301=DIRECTION('center_axis',(-1.,0.,0.));
#10302=DIRECTION('ref_axis',(0.,-0.689355356245991,-0.72442335192549));
#10303=DIRECTION('center_axis',(-1.,0.,0.));
#10304=DIRECTION('ref_axis',(0.,-0.996328365176441,0.0856141854183135));
#10305=DIRECTION('center_axis',(-1.,0.,0.));
#10306=DIRECTION('ref_axis',(0.,-0.881551994715417,0.472086941794909));
#10307=DIRECTION('center_axis',(-1.,0.,0.));
#10308=DIRECTION('ref_axis',(0.,-0.808814416871714,-0.58806397531261));
#10309=DIRECTION('center_axis',(-1.,0.,0.));
#10310=DIRECTION('ref_axis',(0.,0.226735766709209,-0.973956309130336));
#10311=DIRECTION('center_axis',(-1.,0.,0.));
#10312=DIRECTION('ref_axis',(0.,0.0987961199440696,-0.995107696022896));
#10313=DIRECTION('center_axis',(-1.,0.,0.));
#10314=DIRECTION('ref_axis',(0.,-0.914106119062975,-0.405475033869689));
#10315=DIRECTION('center_axis',(-1.,0.,0.));
#10316=DIRECTION('ref_axis',(0.,-0.887724253911928,0.460375552149015));
#10317=DIRECTION('center_axis',(-1.,0.,0.));
#10318=DIRECTION('ref_axis',(0.,-0.633787993501308,0.77350680623611));
#10319=DIRECTION('center_axis',(-1.,0.,0.));
#10320=DIRECTION('ref_axis',(0.,-0.972289425870717,-0.233780393403704));
#10321=DIRECTION('center_axis',(-1.,0.,0.));
#10322=DIRECTION('ref_axis',(0.,-0.163240409200793,-0.986586321009955));
#10323=DIRECTION('center_axis',(-1.,0.,0.));
#10324=DIRECTION('ref_axis',(0.,-0.289535515579091,-0.95716727128457));
#10325=DIRECTION('center_axis',(-1.,0.,0.));
#10326=DIRECTION('ref_axis',(0.,-0.999692511645211,-0.0247968175476203));
#10327=DIRECTION('center_axis',(-1.,0.,0.));
#10328=DIRECTION('ref_axis',(0.,-0.643972172229716,0.76504891437982));
#10329=DIRECTION('center_axis',(-1.,0.,0.));
#10330=DIRECTION('ref_axis',(0.,-0.289535515578999,0.957167271284598));
#10331=DIRECTION('center_axis',(-1.,0.,0.));
#10332=DIRECTION('ref_axis',(0.,-0.987742183606507,0.156094134176301));
#10333=DIRECTION('center_axis',(-1.,0.,0.));
#10334=DIRECTION('ref_axis',(0.,-0.528364712587889,-0.849017508943083));
#10335=DIRECTION('center_axis',(-1.,0.,0.));
#10336=DIRECTION('ref_axis',(0.,-0.633787993501308,-0.773506806236109));
#10337=DIRECTION('center_axis',(-1.,0.,0.));
#10338=DIRECTION('ref_axis',(0.,-0.933084781564671,0.359656489462389));
#10339=DIRECTION('center_axis',(-1.,0.,0.));
#10340=DIRECTION('ref_axis',(0.,-0.302181164947791,0.953250514581973));
#10341=DIRECTION('center_axis',(-1.,0.,0.));
#10342=DIRECTION('ref_axis',(0.,0.098796119944139,0.99510769602289));
#10343=DIRECTION('center_axis',(-1.,0.,0.));
#10344=DIRECTION('ref_axis',(0.,-0.852820147793402,0.522204744824901));
#10345=DIRECTION('center_axis',(-1.,0.,0.));
#10346=DIRECTION('ref_axis',(0.,-0.813050278121574,-0.582193477502481));
#10347=DIRECTION('center_axis',(-1.,0.,0.));
#10348=DIRECTION('ref_axis',(0.,-0.881551994715481,-0.47208694179479));
#10349=DIRECTION('center_axis',(-1.,0.,0.));
#10350=DIRECTION('ref_axis',(0.,-0.72442335192549,0.689355356245991));
#10351=DIRECTION('center_axis',(-1.,0.,0.));
#10352=DIRECTION('ref_axis',(0.,0.0856141854183135,0.996328365176441));
#10353=DIRECTION('center_axis',(-1.,0.,0.));
#10354=DIRECTION('ref_axis',(0.,0.472086941794909,0.881551994715417));
#10355=DIRECTION('center_axis',(-1.,0.,0.));
#10356=DIRECTION('ref_axis',(0.,-0.58806397531261,0.808814416871714));
#10357=DIRECTION('center_axis',(-1.,0.,0.));
#10358=DIRECTION('ref_axis',(0.,-0.973956309130336,-0.226735766709209));
#10359=DIRECTION('center_axis',(-1.,0.,0.));
#10360=DIRECTION('ref_axis',(0.,-0.995107696022895,-0.0987961199440795));
#10361=DIRECTION('center_axis',(-1.,0.,0.));
#10362=DIRECTION('ref_axis',(0.,-0.405475033869689,0.914106119062975));
#10363=DIRECTION('center_axis',(-1.,0.,0.));
#10364=DIRECTION('ref_axis',(0.,0.460375552149015,0.887724253911928));
#10365=DIRECTION('center_axis',(-1.,0.,0.));
#10366=DIRECTION('ref_axis',(0.,0.77350680623611,0.633787993501308));
#10367=DIRECTION('center_axis',(-1.,0.,0.));
#10368=DIRECTION('ref_axis',(0.,-0.233780393403704,0.972289425870717));
#10369=DIRECTION('center_axis',(-1.,0.,0.));
#10370=DIRECTION('ref_axis',(0.,-0.986586321009955,0.163240409200793));
#10371=DIRECTION('center_axis',(-1.,0.,0.));
#10372=DIRECTION('ref_axis',(0.,-0.95716727128457,0.289535515579091));
#10373=DIRECTION('center_axis',(-1.,0.,0.));
#10374=DIRECTION('ref_axis',(0.,-0.0247968175476203,0.999692511645211));
#10375=DIRECTION('center_axis',(-1.,0.,0.));
#10376=DIRECTION('ref_axis',(0.,0.76504891437982,0.643972172229716));
#10377=DIRECTION('center_axis',(-1.,0.,0.));
#10378=DIRECTION('ref_axis',(0.,0.957167271284598,0.289535515578999));
#10379=DIRECTION('center_axis',(-1.,0.,0.));
#10380=DIRECTION('ref_axis',(0.,0.156094134176301,0.987742183606507));
#10381=DIRECTION('center_axis',(-1.,0.,0.));
#10382=DIRECTION('ref_axis',(0.,-0.849017508943083,0.528364712587889));
#10383=DIRECTION('center_axis',(-1.,0.,0.));
#10384=DIRECTION('ref_axis',(0.,-0.773506806236109,0.633787993501308));
#10385=DIRECTION('center_axis',(-1.,0.,0.));
#10386=DIRECTION('ref_axis',(0.,0.359656489462389,0.933084781564671));
#10387=DIRECTION('center_axis',(-1.,0.,0.));
#10388=DIRECTION('ref_axis',(0.,0.953250514581973,0.302181164947791));
#10389=DIRECTION('center_axis',(-1.,0.,0.));
#10390=DIRECTION('ref_axis',(0.,0.99510769602289,-0.098796119944139));
#10391=DIRECTION('center_axis',(-1.,0.,0.));
#10392=DIRECTION('ref_axis',(0.,0.522204744824901,0.852820147793402));
#10393=DIRECTION('center_axis',(-1.,0.,0.));
#10394=DIRECTION('ref_axis',(0.,-0.582193477502481,0.813050278121574));
#10395=DIRECTION('center_axis',(-1.,0.,0.));
#10396=DIRECTION('ref_axis',(0.,-0.47208694179479,0.881551994715481));
#10397=DIRECTION('center_axis',(-1.,0.,0.));
#10398=DIRECTION('ref_axis',(0.,0.689355356245991,0.72442335192549));
#10399=DIRECTION('center_axis',(-1.,0.,0.));
#10400=DIRECTION('ref_axis',(0.,0.996328365176441,-0.0856141854183135));
#10401=DIRECTION('center_axis',(-1.,0.,0.));
#10402=DIRECTION('ref_axis',(0.,0.881551994715417,-0.472086941794909));
#10403=DIRECTION('center_axis',(-1.,0.,0.));
#10404=DIRECTION('ref_axis',(0.,0.808814416871714,0.58806397531261));
#10405=DIRECTION('center_axis',(-1.,0.,0.));
#10406=DIRECTION('ref_axis',(0.,-0.226735766709209,0.973956309130336));
#10407=DIRECTION('center_axis',(-1.,0.,0.));
#10408=DIRECTION('ref_axis',(0.,-0.0987961199440696,0.995107696022896));
#10409=DIRECTION('center_axis',(-1.,0.,0.));
#10410=DIRECTION('ref_axis',(0.,0.914106119062975,0.405475033869689));
#10411=DIRECTION('center_axis',(-1.,0.,0.));
#10412=DIRECTION('ref_axis',(0.,0.887724253911928,-0.460375552149015));
#10413=DIRECTION('center_axis',(-1.,0.,0.));
#10414=DIRECTION('ref_axis',(0.,0.633787993501308,-0.77350680623611));
#10415=DIRECTION('center_axis',(-1.,0.,0.));
#10416=DIRECTION('ref_axis',(0.,0.972289425870717,0.233780393403704));
#10417=DIRECTION('center_axis',(-1.,0.,0.));
#10418=DIRECTION('ref_axis',(0.,0.163240409200793,0.986586321009955));
#10419=DIRECTION('center_axis',(-1.,0.,0.));
#10420=DIRECTION('ref_axis',(0.,0.289535515579091,0.95716727128457));
#10421=DIRECTION('center_axis',(-1.,0.,0.));
#10422=DIRECTION('ref_axis',(0.,0.999692511645211,0.0247968175476203));
#10423=DIRECTION('center_axis',(-1.,0.,0.));
#10424=DIRECTION('ref_axis',(0.,0.643972172229716,-0.76504891437982));
#10425=DIRECTION('center_axis',(-1.,0.,0.));
#10426=DIRECTION('ref_axis',(0.,0.289535515578999,-0.957167271284598));
#10427=DIRECTION('center_axis',(-1.,0.,0.));
#10428=DIRECTION('ref_axis',(0.,0.987742183606507,-0.156094134176301));
#10429=DIRECTION('center_axis',(-1.,0.,0.));
#10430=DIRECTION('ref_axis',(0.,0.528364712587889,0.849017508943083));
#10431=DIRECTION('center_axis',(-1.,0.,0.));
#10432=DIRECTION('ref_axis',(0.,0.633787993501308,0.773506806236109));
#10433=DIRECTION('center_axis',(-1.,0.,0.));
#10434=DIRECTION('ref_axis',(0.,0.933084781564671,-0.359656489462389));
#10435=DIRECTION('center_axis',(-1.,0.,0.));
#10436=DIRECTION('ref_axis',(0.,0.302181164947791,-0.953250514581973));
#10437=DIRECTION('center_axis',(-1.,0.,0.));
#10438=DIRECTION('ref_axis',(0.,-0.098796119944139,-0.99510769602289));
#10439=DIRECTION('center_axis',(-1.,0.,0.));
#10440=DIRECTION('ref_axis',(0.,0.852820147793402,-0.522204744824901));
#10441=DIRECTION('center_axis',(-1.,0.,0.));
#10442=DIRECTION('ref_axis',(0.,0.813050278121574,0.582193477502481));
#10443=DIRECTION('center_axis',(-1.,0.,0.));
#10444=DIRECTION('ref_axis',(0.,0.881551994715481,0.47208694179479));
#10445=DIRECTION('center_axis',(-1.,0.,0.));
#10446=DIRECTION('ref_axis',(0.,0.72442335192549,-0.689355356245991));
#10447=DIRECTION('center_axis',(-1.,0.,0.));
#10448=DIRECTION('ref_axis',(0.,-0.0856141854183135,-0.996328365176441));
#10449=DIRECTION('center_axis',(-1.,0.,0.));
#10450=DIRECTION('ref_axis',(0.,-0.472086941794909,-0.881551994715417));
#10451=DIRECTION('center_axis',(-1.,0.,0.));
#10452=DIRECTION('ref_axis',(0.,0.58806397531261,-0.808814416871714));
#10453=DIRECTION('center_axis',(-1.,0.,0.));
#10454=DIRECTION('ref_axis',(0.,0.973956309130336,0.226735766709209));
#10455=DIRECTION('center_axis',(-1.,0.,0.));
#10456=DIRECTION('ref_axis',(0.,0.995107696022895,0.0987961199440795));
#10457=DIRECTION('center_axis',(-1.,0.,0.));
#10458=DIRECTION('ref_axis',(0.,0.405475033869689,-0.914106119062975));
#10459=DIRECTION('center_axis',(-1.,0.,0.));
#10460=DIRECTION('ref_axis',(0.,-0.460375552149015,-0.887724253911928));
#10461=DIRECTION('center_axis',(-1.,0.,0.));
#10462=DIRECTION('ref_axis',(0.,-0.77350680623611,-0.633787993501308));
#10463=DIRECTION('center_axis',(-1.,0.,0.));
#10464=DIRECTION('ref_axis',(0.,0.233780393403704,-0.972289425870717));
#10465=DIRECTION('center_axis',(-1.,0.,0.));
#10466=DIRECTION('ref_axis',(0.,0.986586321009955,-0.163240409200793));
#10467=DIRECTION('center_axis',(-1.,0.,0.));
#10468=DIRECTION('ref_axis',(0.,0.95716727128457,-0.289535515579091));
#10469=DIRECTION('center_axis',(-1.,0.,0.));
#10470=DIRECTION('ref_axis',(0.,0.0247968175476203,-0.999692511645211));
#10471=DIRECTION('center_axis',(-1.,0.,0.));
#10472=DIRECTION('ref_axis',(0.,-0.76504891437982,-0.643972172229716));
#10473=DIRECTION('center_axis',(-1.,0.,0.));
#10474=DIRECTION('ref_axis',(0.,-0.957167271284598,-0.289535515578999));
#10475=DIRECTION('center_axis',(-1.,0.,0.));
#10476=DIRECTION('ref_axis',(0.,-0.156094134176301,-0.987742183606507));
#10477=DIRECTION('center_axis',(-1.,0.,0.));
#10478=DIRECTION('ref_axis',(0.,0.849017508943083,-0.528364712587889));
#10479=DIRECTION('center_axis',(-1.,0.,0.));
#10480=DIRECTION('ref_axis',(0.,0.773506806236109,-0.633787993501308));
#10481=DIRECTION('center_axis',(-1.,0.,0.));
#10482=DIRECTION('ref_axis',(0.,-0.359656489462389,-0.933084781564671));
#10483=DIRECTION('center_axis',(-1.,0.,0.));
#10484=DIRECTION('ref_axis',(0.,-0.953250514581973,-0.302181164947791));
#10485=DIRECTION('center_axis',(-1.,0.,0.));
#10486=DIRECTION('ref_axis',(0.,-0.99510769602289,0.098796119944139));
#10487=DIRECTION('',(0.,0.500000000000017,0.866025403784429));
#10488=DIRECTION('',(0.,-0.500000000000017,0.866025403784429));
#10489=DIRECTION('',(0.,-1.,0.));
#10490=DIRECTION('',(0.,-0.500000000000017,-0.866025403784429));
#10491=DIRECTION('',(0.,0.500000000000017,-0.866025403784429));
#10492=DIRECTION('',(0.,1.,0.));
#10493=DIRECTION('center_axis',(0.,-0.866025403784429,0.500000000000017));
#10494=DIRECTION('ref_axis',(0.,0.500000000000017,0.866025403784429));
#10495=DIRECTION('',(1.,0.,0.));
#10496=DIRECTION('',(0.,0.500000000000017,0.866025403784429));
#10497=DIRECTION('',(1.,0.,0.));
#10498=DIRECTION('center_axis',(0.,-0.866025403784429,-0.500000000000017));
#10499=DIRECTION('ref_axis',(0.,-0.500000000000017,0.866025403784429));
#10500=DIRECTION('',(0.,-0.500000000000017,0.866025403784429));
#10501=DIRECTION('',(1.,0.,0.));
#10502=DIRECTION('center_axis',(0.,0.,-1.));
#10503=DIRECTION('ref_axis',(0.,-1.,0.));
#10504=DIRECTION('',(0.,-1.,0.));
#10505=DIRECTION('',(1.,0.,0.));
#10506=DIRECTION('center_axis',(0.,0.866025403784429,-0.500000000000017));
#10507=DIRECTION('ref_axis',(0.,-0.500000000000017,-0.866025403784429));
#10508=DIRECTION('',(0.,-0.500000000000017,-0.866025403784429));
#10509=DIRECTION('',(1.,0.,0.));
#10510=DIRECTION('center_axis',(0.,0.866025403784429,0.500000000000017));
#10511=DIRECTION('ref_axis',(0.,0.500000000000017,-0.866025403784429));
#10512=DIRECTION('',(0.,0.500000000000017,-0.866025403784429));
#10513=DIRECTION('',(1.,0.,0.));
#10514=DIRECTION('center_axis',(0.,0.,1.));
#10515=DIRECTION('ref_axis',(0.,1.,0.));
#10516=DIRECTION('',(0.,1.,0.));
#10517=DIRECTION('center_axis',(1.,0.,0.));
#10518=DIRECTION('ref_axis',(0.,-1.,0.));
#10519=DIRECTION('center_axis',(1.,0.,0.));
#10520=DIRECTION('ref_axis',(0.,1.,0.));
#10521=DIRECTION('center_axis',(1.,0.,0.));
#10522=DIRECTION('ref_axis',(0.,-1.,0.));
#10523=DIRECTION('',(1.,0.,0.));
#10524=DIRECTION('center_axis',(-1.,0.,0.));
#10525=DIRECTION('ref_axis',(0.,-1.,0.));
#10526=DIRECTION('center_axis',(1.,0.,0.));
#10527=DIRECTION('ref_axis',(0.,-1.,0.));
#10528=DIRECTION('center_axis',(1.,0.,0.));
#10529=DIRECTION('ref_axis',(0.,-0.233780393403704,-0.972289425870717));
#10530=DIRECTION('center_axis',(-1.,0.,0.));
#10531=DIRECTION('ref_axis',(0.,-0.957167271284598,-0.289535515578999));
#10532=DIRECTION('center_axis',(-1.,0.,0.));
#10533=DIRECTION('ref_axis',(0.,-0.76504891437982,-0.643972172229716));
#10534=DIRECTION('center_axis',(-1.,0.,0.));
#10535=DIRECTION('ref_axis',(0.,0.0247968175476203,-0.999692511645211));
#10536=DIRECTION('center_axis',(-1.,0.,0.));
#10537=DIRECTION('ref_axis',(0.,0.957167271284598,-0.289535515578999));
#10538=DIRECTION('center_axis',(-1.,0.,0.));
#10539=DIRECTION('ref_axis',(0.,0.986586321009955,-0.163240409200793));
#10540=DIRECTION('center_axis',(1.,0.,0.));
#10541=DIRECTION('ref_axis',(0.,0.156094134176301,-0.987742183606507));
#10542=DIRECTION('center_axis',(-1.,0.,0.));
#10543=DIRECTION('ref_axis',(0.,-0.77350680623611,-0.633787993501308));
#10544=DIRECTION('center_axis',(-1.,0.,0.));
#10545=DIRECTION('ref_axis',(0.,-0.460375552149015,-0.887724253911928));
#10546=DIRECTION('center_axis',(-1.,0.,0.));
#10547=DIRECTION('ref_axis',(0.,0.405475033869689,-0.914106119062975));
#10548=DIRECTION('center_axis',(-1.,0.,0.));
#10549=DIRECTION('ref_axis',(0.,0.995107696022889,0.0987961199441488));
#10550=DIRECTION('center_axis',(-1.,0.,0.));
#10551=DIRECTION('ref_axis',(0.,0.973956309130336,0.226735766709209));
#10552=DIRECTION('center_axis',(1.,0.,0.));
#10553=DIRECTION('ref_axis',(0.,0.522204744824901,-0.852820147793402));
#10554=DIRECTION('center_axis',(-1.,0.,0.));
#10555=DIRECTION('ref_axis',(0.,-0.472086941794909,-0.881551994715417));
#10556=DIRECTION('center_axis',(-1.,0.,0.));
#10557=DIRECTION('ref_axis',(0.,-0.0856141854183135,-0.996328365176441));
#10558=DIRECTION('center_axis',(-1.,0.,0.));
#10559=DIRECTION('ref_axis',(0.,0.72442335192549,-0.689355356245991));
#10560=DIRECTION('center_axis',(-1.,0.,0.));
#10561=DIRECTION('ref_axis',(0.,0.881551994715417,0.472086941794909));
#10562=DIRECTION('center_axis',(-1.,0.,0.));
#10563=DIRECTION('ref_axis',(0.,0.813050278121574,0.582193477502481));
#10564=DIRECTION('center_axis',(1.,0.,0.));
#10565=DIRECTION('ref_axis',(0.,0.808814416871714,-0.58806397531261));
#10566=DIRECTION('center_axis',(-1.,0.,0.));
#10567=DIRECTION('ref_axis',(0.,-0.098796119944139,-0.99510769602289));
#10568=DIRECTION('center_axis',(-1.,0.,0.));
#10569=DIRECTION('ref_axis',(0.,0.302181164947791,-0.953250514581973));
#10570=DIRECTION('center_axis',(-1.,0.,0.));
#10571=DIRECTION('ref_axis',(0.,0.933084781564671,-0.359656489462389));
#10572=DIRECTION('center_axis',(-1.,0.,0.));
#10573=DIRECTION('ref_axis',(0.,0.633787993501308,0.773506806236109));
#10574=DIRECTION('center_axis',(-1.,0.,0.));
#10575=DIRECTION('ref_axis',(0.,0.528364712587889,0.849017508943083));
#10576=DIRECTION('center_axis',(1.,0.,0.));
#10577=DIRECTION('ref_axis',(0.,0.972289425870695,-0.233780393403799));
#10578=DIRECTION('center_axis',(-1.,0.,0.));
#10579=DIRECTION('ref_axis',(0.,0.289535515578999,-0.957167271284598));
#10580=DIRECTION('center_axis',(-1.,0.,0.));
#10581=DIRECTION('ref_axis',(0.,0.643972172229716,-0.76504891437982));
#10582=DIRECTION('center_axis',(-1.,0.,0.));
#10583=DIRECTION('ref_axis',(0.,0.999692511645211,0.0247968175476203));
#10584=DIRECTION('center_axis',(-1.,0.,0.));
#10585=DIRECTION('ref_axis',(0.,0.289535515578999,0.957167271284598));
#10586=DIRECTION('center_axis',(-1.,0.,0.));
#10587=DIRECTION('ref_axis',(0.,0.163240409200793,0.986586321009955));
#10588=DIRECTION('center_axis',(1.,0.,0.));
#10589=DIRECTION('ref_axis',(0.,0.987742183606507,0.156094134176301));
#10590=DIRECTION('center_axis',(-1.,0.,0.));
#10591=DIRECTION('ref_axis',(0.,0.633787993501308,-0.77350680623611));
#10592=DIRECTION('center_axis',(-1.,0.,0.));
#10593=DIRECTION('ref_axis',(0.,0.887724253911928,-0.460375552149015));
#10594=DIRECTION('center_axis',(-1.,0.,0.));
#10595=DIRECTION('ref_axis',(0.,0.914106119062975,0.405475033869689));
#10596=DIRECTION('center_axis',(-1.,0.,0.));
#10597=DIRECTION('ref_axis',(0.,-0.0987961199441488,0.995107696022889));
#10598=DIRECTION('center_axis',(-1.,0.,0.));
#10599=DIRECTION('ref_axis',(0.,-0.226735766709209,0.973956309130336));
#10600=DIRECTION('center_axis',(1.,0.,0.));
#10601=DIRECTION('ref_axis',(0.,0.852820147793402,0.522204744824901));
#10602=DIRECTION('center_axis',(-1.,0.,0.));
#10603=DIRECTION('ref_axis',(0.,0.881551994715417,-0.472086941794909));
#10604=DIRECTION('center_axis',(-1.,0.,0.));
#10605=DIRECTION('ref_axis',(0.,0.996328365176441,-0.0856141854183135));
#10606=DIRECTION('center_axis',(-1.,0.,0.));
#10607=DIRECTION('ref_axis',(0.,0.689355356245991,0.72442335192549));
#10608=DIRECTION('center_axis',(-1.,0.,0.));
#10609=DIRECTION('ref_axis',(0.,-0.472086941794909,0.881551994715417));
#10610=DIRECTION('center_axis',(-1.,0.,0.));
#10611=DIRECTION('ref_axis',(0.,-0.582193477502481,0.813050278121574));
#10612=DIRECTION('center_axis',(1.,0.,0.));
#10613=DIRECTION('ref_axis',(0.,0.58806397531261,0.808814416871714));
#10614=DIRECTION('center_axis',(-1.,0.,0.));
#10615=DIRECTION('ref_axis',(0.,0.99510769602289,-0.098796119944139));
#10616=DIRECTION('center_axis',(-1.,0.,0.));
#10617=DIRECTION('ref_axis',(0.,0.953250514581973,0.302181164947791));
#10618=DIRECTION('center_axis',(-1.,0.,0.));
#10619=DIRECTION('ref_axis',(0.,0.359656489462389,0.933084781564671));
#10620=DIRECTION('center_axis',(-1.,0.,0.));
#10621=DIRECTION('ref_axis',(0.,-0.773506806236109,0.633787993501308));
#10622=DIRECTION('center_axis',(-1.,0.,0.));
#10623=DIRECTION('ref_axis',(0.,-0.849017508943083,0.528364712587889));
#10624=DIRECTION('center_axis',(1.,0.,0.));
#10625=DIRECTION('ref_axis',(0.,0.233780393403799,0.972289425870695));
#10626=DIRECTION('center_axis',(-1.,0.,0.));
#10627=DIRECTION('ref_axis',(0.,0.957167271284598,0.289535515578999));
#10628=DIRECTION('center_axis',(-1.,0.,0.));
#10629=DIRECTION('ref_axis',(0.,0.76504891437982,0.643972172229716));
#10630=DIRECTION('center_axis',(-1.,0.,0.));
#10631=DIRECTION('ref_axis',(0.,-0.0247968175476203,0.999692511645211));
#10632=DIRECTION('center_axis',(-1.,0.,0.));
#10633=DIRECTION('ref_axis',(0.,-0.957167271284598,0.289535515578999));
#10634=DIRECTION('center_axis',(-1.,0.,0.));
#10635=DIRECTION('ref_axis',(0.,-0.986586321009955,0.163240409200793));
#10636=DIRECTION('center_axis',(1.,0.,0.));
#10637=DIRECTION('ref_axis',(0.,-0.156094134176301,0.987742183606507));
#10638=DIRECTION('center_axis',(-1.,0.,0.));
#10639=DIRECTION('ref_axis',(0.,0.77350680623611,0.633787993501308));
#10640=DIRECTION('center_axis',(-1.,0.,0.));
#10641=DIRECTION('ref_axis',(0.,0.460375552149015,0.887724253911928));
#10642=DIRECTION('center_axis',(-1.,0.,0.));
#10643=DIRECTION('ref_axis',(0.,-0.405475033869689,0.914106119062975));
#10644=DIRECTION('center_axis',(-1.,0.,0.));
#10645=DIRECTION('ref_axis',(0.,-0.995107696022889,-0.0987961199441488));
#10646=DIRECTION('center_axis',(-1.,0.,0.));
#10647=DIRECTION('ref_axis',(0.,-0.973956309130336,-0.226735766709209));
#10648=DIRECTION('center_axis',(1.,0.,0.));
#10649=DIRECTION('ref_axis',(0.,-0.522204744824901,0.852820147793402));
#10650=DIRECTION('center_axis',(-1.,0.,0.));
#10651=DIRECTION('ref_axis',(0.,0.472086941794909,0.881551994715417));
#10652=DIRECTION('center_axis',(-1.,0.,0.));
#10653=DIRECTION('ref_axis',(0.,0.0856141854183135,0.996328365176441));
#10654=DIRECTION('center_axis',(-1.,0.,0.));
#10655=DIRECTION('ref_axis',(0.,-0.72442335192549,0.689355356245991));
#10656=DIRECTION('center_axis',(-1.,0.,0.));
#10657=DIRECTION('ref_axis',(0.,-0.881551994715417,-0.472086941794909));
#10658=DIRECTION('center_axis',(-1.,0.,0.));
#10659=DIRECTION('ref_axis',(0.,-0.813050278121574,-0.582193477502481));
#10660=DIRECTION('center_axis',(1.,0.,0.));
#10661=DIRECTION('ref_axis',(0.,-0.808814416871714,0.58806397531261));
#10662=DIRECTION('center_axis',(-1.,0.,0.));
#10663=DIRECTION('ref_axis',(0.,0.098796119944139,0.99510769602289));
#10664=DIRECTION('center_axis',(-1.,0.,0.));
#10665=DIRECTION('ref_axis',(0.,-0.302181164947791,0.953250514581973));
#10666=DIRECTION('center_axis',(-1.,0.,0.));
#10667=DIRECTION('ref_axis',(0.,-0.933084781564671,0.359656489462389));
#10668=DIRECTION('center_axis',(-1.,0.,0.));
#10669=DIRECTION('ref_axis',(0.,-0.633787993501308,-0.773506806236109));
#10670=DIRECTION('center_axis',(-1.,0.,0.));
#10671=DIRECTION('ref_axis',(0.,-0.528364712587889,-0.849017508943083));
#10672=DIRECTION('center_axis',(1.,0.,0.));
#10673=DIRECTION('ref_axis',(0.,-0.972289425870717,0.233780393403704));
#10674=DIRECTION('center_axis',(-1.,0.,0.));
#10675=DIRECTION('ref_axis',(0.,-0.289535515578999,0.957167271284598));
#10676=DIRECTION('center_axis',(-1.,0.,0.));
#10677=DIRECTION('ref_axis',(0.,-0.643972172229716,0.76504891437982));
#10678=DIRECTION('center_axis',(-1.,0.,0.));
#10679=DIRECTION('ref_axis',(0.,-0.999692511645211,-0.0247968175476203));
#10680=DIRECTION('center_axis',(-1.,0.,0.));
#10681=DIRECTION('ref_axis',(0.,-0.289535515578999,-0.957167271284598));
#10682=DIRECTION('center_axis',(-1.,0.,0.));
#10683=DIRECTION('ref_axis',(0.,-0.163240409200793,-0.986586321009955));
#10684=DIRECTION('center_axis',(1.,0.,0.));
#10685=DIRECTION('ref_axis',(0.,-0.987742183606507,-0.156094134176301));
#10686=DIRECTION('center_axis',(-1.,0.,0.));
#10687=DIRECTION('ref_axis',(0.,-0.633787993501308,0.77350680623611));
#10688=DIRECTION('center_axis',(-1.,0.,0.));
#10689=DIRECTION('ref_axis',(0.,-0.887724253911928,0.460375552149015));
#10690=DIRECTION('center_axis',(-1.,0.,0.));
#10691=DIRECTION('ref_axis',(0.,-0.914106119062975,-0.405475033869689));
#10692=DIRECTION('center_axis',(-1.,0.,0.));
#10693=DIRECTION('ref_axis',(0.,0.0987961199441488,-0.995107696022889));
#10694=DIRECTION('center_axis',(-1.,0.,0.));
#10695=DIRECTION('ref_axis',(0.,0.226735766709209,-0.973956309130336));
#10696=DIRECTION('center_axis',(1.,0.,0.));
#10697=DIRECTION('ref_axis',(0.,-0.852820147793402,-0.522204744824901));
#10698=DIRECTION('center_axis',(-1.,0.,0.));
#10699=DIRECTION('ref_axis',(0.,-0.881551994715417,0.472086941794909));
#10700=DIRECTION('center_axis',(-1.,0.,0.));
#10701=DIRECTION('ref_axis',(0.,-0.996328365176441,0.0856141854183135));
#10702=DIRECTION('center_axis',(-1.,0.,0.));
#10703=DIRECTION('ref_axis',(0.,-0.689355356245991,-0.72442335192549));
#10704=DIRECTION('center_axis',(-1.,0.,0.));
#10705=DIRECTION('ref_axis',(0.,0.472086941794909,-0.881551994715417));
#10706=DIRECTION('center_axis',(-1.,0.,0.));
#10707=DIRECTION('ref_axis',(0.,0.582193477502481,-0.813050278121574));
#10708=DIRECTION('center_axis',(1.,0.,0.));
#10709=DIRECTION('ref_axis',(0.,-0.58806397531261,-0.808814416871714));
#10710=DIRECTION('center_axis',(-1.,0.,0.));
#10711=DIRECTION('ref_axis',(0.,-0.99510769602289,0.098796119944139));
#10712=DIRECTION('center_axis',(-1.,0.,0.));
#10713=DIRECTION('ref_axis',(0.,-0.953250514581973,-0.302181164947791));
#10714=DIRECTION('center_axis',(-1.,0.,0.));
#10715=DIRECTION('ref_axis',(0.,-0.359656489462389,-0.933084781564671));
#10716=DIRECTION('center_axis',(-1.,0.,0.));
#10717=DIRECTION('ref_axis',(0.,0.773506806236109,-0.633787993501308));
#10718=DIRECTION('center_axis',(-1.,0.,0.));
#10719=DIRECTION('ref_axis',(0.,0.849017508943083,-0.528364712587889));
#10720=DIRECTION('center_axis',(-1.,0.,0.));
#10721=DIRECTION('ref_axis',(0.,1.,0.));
#10722=DIRECTION('',(-1.,0.,0.));
#10723=DIRECTION('',(-1.,0.,0.));
#10724=DIRECTION('center_axis',(-1.,0.,0.));
#10725=DIRECTION('ref_axis',(0.,1.,0.));
#10726=DIRECTION('',(-1.,0.,0.));
#10727=DIRECTION('',(-1.,0.,0.));
#10728=DIRECTION('center_axis',(-1.,0.,0.));
#10729=DIRECTION('ref_axis',(0.,1.,0.));
#10730=DIRECTION('',(-1.,0.,0.));
#10731=DIRECTION('',(-1.,0.,0.));
#10732=DIRECTION('center_axis',(-1.,0.,0.));
#10733=DIRECTION('ref_axis',(0.,1.,0.));
#10734=DIRECTION('',(-1.,0.,0.));
#10735=DIRECTION('',(-1.,0.,0.));
#10736=DIRECTION('center_axis',(-1.,0.,0.));
#10737=DIRECTION('ref_axis',(0.,1.,0.));
#10738=DIRECTION('',(-1.,0.,0.));
#10739=DIRECTION('',(-1.,0.,0.));
#10740=DIRECTION('center_axis',(-1.,0.,0.));
#10741=DIRECTION('ref_axis',(0.,1.,0.));
#10742=DIRECTION('',(-1.,0.,0.));
#10743=DIRECTION('',(-1.,0.,0.));
#10744=DIRECTION('center_axis',(-1.,0.,0.));
#10745=DIRECTION('ref_axis',(0.,1.,0.));
#10746=DIRECTION('',(-1.,0.,0.));
#10747=DIRECTION('',(-1.,0.,0.));
#10748=DIRECTION('center_axis',(-1.,0.,0.));
#10749=DIRECTION('ref_axis',(0.,1.,0.));
#10750=DIRECTION('',(-1.,0.,0.));
#10751=DIRECTION('',(-1.,0.,0.));
#10752=DIRECTION('center_axis',(-1.,0.,0.));
#10753=DIRECTION('ref_axis',(0.,1.,0.));
#10754=DIRECTION('',(-1.,0.,0.));
#10755=DIRECTION('',(-1.,0.,0.));
#10756=DIRECTION('center_axis',(-1.,0.,0.));
#10757=DIRECTION('ref_axis',(0.,1.,0.));
#10758=DIRECTION('',(-1.,0.,0.));
#10759=DIRECTION('',(-1.,0.,0.));
#10760=DIRECTION('center_axis',(-1.,0.,0.));
#10761=DIRECTION('ref_axis',(0.,1.,0.));
#10762=DIRECTION('',(-1.,0.,0.));
#10763=DIRECTION('',(-1.,0.,0.));
#10764=DIRECTION('center_axis',(-1.,0.,0.));
#10765=DIRECTION('ref_axis',(0.,1.,0.));
#10766=DIRECTION('',(-1.,0.,0.));
#10767=DIRECTION('',(-1.,0.,0.));
#10768=DIRECTION('center_axis',(-1.,0.,0.));
#10769=DIRECTION('ref_axis',(0.,1.,0.));
#10770=DIRECTION('',(-1.,0.,0.));
#10771=DIRECTION('',(-1.,0.,0.));
#10772=DIRECTION('center_axis',(-1.,0.,0.));
#10773=DIRECTION('ref_axis',(0.,1.,0.));
#10774=DIRECTION('',(-1.,0.,0.));
#10775=DIRECTION('',(-1.,0.,0.));
#10776=DIRECTION('center_axis',(-1.,0.,0.));
#10777=DIRECTION('ref_axis',(0.,1.,0.));
#10778=DIRECTION('',(-1.,0.,0.));
#10779=DIRECTION('',(-1.,0.,0.));
#10780=DIRECTION('center_axis',(-1.,0.,0.));
#10781=DIRECTION('ref_axis',(0.,1.,0.));
#10782=DIRECTION('',(-1.,0.,0.));
#10783=DIRECTION('',(-1.,0.,0.));
#10784=DIRECTION('center_axis',(-1.,0.,0.));
#10785=DIRECTION('ref_axis',(0.,0.923879532511285,0.382683432365094));
#10786=DIRECTION('',(1.,0.,0.));
#10787=DIRECTION('center_axis',(-1.,0.,0.));
#10788=DIRECTION('ref_axis',(0.,0.923879532511285,0.382683432365094));
#10789=DIRECTION('',(1.,0.,0.));
#10790=DIRECTION('',(1.,0.,0.));
#10791=DIRECTION('center_axis',(0.,0.923879532511285,0.382683432365094));
#10792=DIRECTION('ref_axis',(1.22464679914735E-16,-0.382683432365094,0.923879532511285));
#10793=DIRECTION('center_axis',(-0.602056836120556,-0.305554823977325,0.737674600094575));
#10794=DIRECTION('ref_axis',(-0.797776104275275,0.192161019234803,-0.571513280802823));
#10795=DIRECTION('center_axis',(0.602056836120892,-0.30555482397723,0.737674600094341));
#10796=DIRECTION('ref_axis',(0.797776104275135,0.268242556610213,-0.539999276176187));
#10797=DIRECTION('center_axis',(-1.,0.,0.));
#10798=DIRECTION('ref_axis',(0.,0.923879532511285,0.382683432365094));
#10799=DIRECTION('',(1.,0.,0.));
#10800=DIRECTION('center_axis',(-1.,0.,0.));
#10801=DIRECTION('ref_axis',(0.,0.923879532511285,0.382683432365094));
#10802=DIRECTION('',(1.,0.,0.));
#10803=DIRECTION('center_axis',(-1.,0.,0.));
#10804=DIRECTION('ref_axis',(0.,0.923879532511285,0.382683432365094));
#10805=DIRECTION('',(1.,0.,0.));
#10806=DIRECTION('center_axis',(-1.,0.,0.));
#10807=DIRECTION('ref_axis',(0.,0.923879532511285,0.382683432365094));
#10808=DIRECTION('center_axis',(-1.,0.,0.));
#10809=DIRECTION('ref_axis',(0.,1.,0.));
#10810=DIRECTION('',(1.,0.,0.));
#10811=DIRECTION('center_axis',(-1.,0.,0.));
#10812=DIRECTION('ref_axis',(0.,1.,0.));
#10813=DIRECTION('',(1.,0.,0.));
#10814=DIRECTION('',(1.,0.,0.));
#10815=DIRECTION('center_axis',(0.,1.,0.));
#10816=DIRECTION('ref_axis',(1.22464679914735E-16,0.,1.));
#10817=DIRECTION('center_axis',(-0.602056836120766,0.,0.798453233496022));
#10818=DIRECTION('ref_axis',(-0.797776104274988,-0.0411750313262452,-0.601546261099765));
#10819=DIRECTION('center_axis',(0.602056836120813,0.,0.798453233495987));
#10820=DIRECTION('ref_axis',(0.797776104274953,0.0411750313262546,-0.601546261099811));
#10821=DIRECTION('center_axis',(-1.,0.,0.));
#10822=DIRECTION('ref_axis',(0.,1.,0.));
#10823=DIRECTION('',(1.,0.,0.));
#10824=DIRECTION('',(1.,0.,0.));
#10825=DIRECTION('',(1.,0.,0.));
#10826=DIRECTION('center_axis',(-1.,0.,0.));
#10827=DIRECTION('ref_axis',(0.,1.,0.));
#10828=DIRECTION('center_axis',(-1.,0.,0.));
#10829=DIRECTION('ref_axis',(0.,1.,0.));
#10830=DIRECTION('center_axis',(-1.,0.,0.));
#10831=DIRECTION('ref_axis',(0.,1.,0.));
#10832=DIRECTION('center_axis',(-1.,0.,0.));
#10833=DIRECTION('ref_axis',(0.,0.707106781186547,0.707106781186547));
#10834=DIRECTION('',(1.,0.,0.));
#10835=DIRECTION('center_axis',(-1.,0.,0.));
#10836=DIRECTION('ref_axis',(0.,0.707106781186548,0.707106781186548));
#10837=DIRECTION('',(1.,0.,0.));
#10838=DIRECTION('',(1.,0.,0.));
#10839=DIRECTION('center_axis',(0.,0.707106781186548,0.707106781186548));
#10840=DIRECTION('ref_axis',(1.22464679914735E-16,-0.707106781186548,0.707106781186548));
#10841=DIRECTION('center_axis',(-0.602056836120681,-0.564591695865409,0.564591695865408));
#10842=DIRECTION('ref_axis',(-0.797776104275146,0.396242296556752,-0.454472584285347));
#10843=DIRECTION('center_axis',(0.602056836120562,-0.564591695865472,0.564591695865472));
#10844=DIRECTION('ref_axis',(0.797776104275237,0.454472584285238,-0.396242296556694));
#10845=DIRECTION('center_axis',(-1.,0.,0.));
#10846=DIRECTION('ref_axis',(0.,0.707106781186548,0.707106781186548));
#10847=DIRECTION('',(1.,0.,0.));
#10848=DIRECTION('center_axis',(-1.,0.,0.));
#10849=DIRECTION('ref_axis',(0.,0.707106781186548,0.707106781186548));
#10850=DIRECTION('',(1.,0.,0.));
#10851=DIRECTION('center_axis',(-1.,0.,0.));
#10852=DIRECTION('ref_axis',(0.,0.707106781186548,0.707106781186548));
#10853=DIRECTION('',(1.,0.,0.));
#10854=DIRECTION('center_axis',(-1.,0.,0.));
#10855=DIRECTION('ref_axis',(0.,0.707106781186547,0.707106781186547));
#10856=DIRECTION('center_axis',(-1.,0.,0.));
#10857=DIRECTION('ref_axis',(0.,0.382683432365094,0.923879532511285));
#10858=DIRECTION('',(1.,0.,0.));
#10859=DIRECTION('center_axis',(-1.,0.,0.));
#10860=DIRECTION('ref_axis',(0.,0.382683432365094,0.923879532511285));
#10861=DIRECTION('',(1.,0.,0.));
#10862=DIRECTION('',(1.,0.,0.));
#10863=DIRECTION('center_axis',(0.,0.382683432365094,0.923879532511285));
#10864=DIRECTION('ref_axis',(1.22464679914735E-16,-0.923879532511285,0.382683432365094));
#10865=DIRECTION('center_axis',(-0.602056836120692,-0.73767460009448,0.305554823977286));
#10866=DIRECTION('ref_axis',(-0.797776104275363,0.539999276176976,-0.268242556607946));
#10867=DIRECTION('center_axis',(0.60205683612067,-0.737674600094496,0.305554823977293));
#10868=DIRECTION('ref_axis',(0.797776104275269,0.571513280802065,-0.192161019237087));
#10869=DIRECTION('center_axis',(-1.,0.,0.));
#10870=DIRECTION('ref_axis',(0.,0.382683432365094,0.923879532511285));
#10871=DIRECTION('',(1.,0.,0.));
#10872=DIRECTION('center_axis',(-1.,0.,0.));
#10873=DIRECTION('ref_axis',(0.,0.382683432365094,0.923879532511285));
#10874=DIRECTION('',(1.,0.,0.));
#10875=DIRECTION('center_axis',(-1.,0.,0.));
#10876=DIRECTION('ref_axis',(0.,0.382683432365094,0.923879532511285));
#10877=DIRECTION('',(1.,0.,0.));
#10878=DIRECTION('center_axis',(-1.,0.,0.));
#10879=DIRECTION('ref_axis',(0.,0.382683432365094,0.923879532511285));
#10880=DIRECTION('center_axis',(-1.,0.,0.));
#10881=DIRECTION('ref_axis',(0.,0.,1.));
#10882=DIRECTION('',(1.,0.,0.));
#10883=DIRECTION('center_axis',(-1.,0.,0.));
#10884=DIRECTION('ref_axis',(0.,0.,1.));
#10885=DIRECTION('',(1.,0.,0.));
#10886=DIRECTION('',(1.,0.,0.));
#10887=DIRECTION('center_axis',(0.,0.,1.));
#10888=DIRECTION('ref_axis',(1.22464679914735E-16,-1.,0.));
#10889=DIRECTION('center_axis',(-0.602056836120766,-0.798453233496022,0.));
#10890=DIRECTION('ref_axis',(-0.797776104274987,0.601546261099764,-0.0411750313262736));
#10891=DIRECTION('center_axis',(0.602056836120813,-0.798453233495987,0.));
#10892=DIRECTION('ref_axis',(0.797776104274952,0.601546261099811,0.0411750313262641));
#10893=DIRECTION('center_axis',(-1.,0.,0.));
#10894=DIRECTION('ref_axis',(0.,0.,1.));
#10895=DIRECTION('',(1.,0.,0.));
#10896=DIRECTION('center_axis',(-1.,0.,0.));
#10897=DIRECTION('ref_axis',(0.,0.,1.));
#10898=DIRECTION('',(1.,0.,0.));
#10899=DIRECTION('center_axis',(-1.,0.,0.));
#10900=DIRECTION('ref_axis',(0.,0.,1.));
#10901=DIRECTION('',(1.,0.,0.));
#10902=DIRECTION('center_axis',(-1.,0.,0.));
#10903=DIRECTION('ref_axis',(0.,0.,1.));
#10904=DIRECTION('center_axis',(-1.,0.,0.));
#10905=DIRECTION('ref_axis',(0.,-0.382683432365094,0.923879532511285));
#10906=DIRECTION('',(1.,0.,0.));
#10907=DIRECTION('center_axis',(-1.,0.,0.));
#10908=DIRECTION('ref_axis',(0.,-0.382683432365094,0.923879532511285));
#10909=DIRECTION('',(1.,0.,0.));
#10910=DIRECTION('',(1.,0.,0.));
#10911=DIRECTION('center_axis',(0.,-0.382683432365094,0.923879532511285));
#10912=DIRECTION('ref_axis',(1.22464679914735E-16,-0.923879532511285,-0.382683432365094));
#10913=DIRECTION('center_axis',(-0.602056836120637,-0.737674600094518,-0.305554823977304));
#10914=DIRECTION('ref_axis',(-0.797776104275215,0.571513280802905,0.192161019234811));
#10915=DIRECTION('center_axis',(0.60205683612087,-0.737674600094356,-0.305554823977236));
#10916=DIRECTION('ref_axis',(0.797776104275151,0.539999276176162,0.268242556610214));
#10917=DIRECTION('center_axis',(-1.,0.,0.));
#10918=DIRECTION('ref_axis',(0.,-0.382683432365094,0.923879532511285));
#10919=DIRECTION('',(1.,0.,0.));
#10920=DIRECTION('center_axis',(-1.,0.,0.));
#10921=DIRECTION('ref_axis',(0.,-0.382683432365094,0.923879532511285));
#10922=DIRECTION('',(1.,0.,0.));
#10923=DIRECTION('center_axis',(-1.,0.,0.));
#10924=DIRECTION('ref_axis',(0.,-0.382683432365094,0.923879532511285));
#10925=DIRECTION('',(1.,0.,0.));
#10926=DIRECTION('center_axis',(-1.,0.,0.));
#10927=DIRECTION('ref_axis',(0.,-0.382683432365094,0.923879532511285));
#10928=DIRECTION('center_axis',(-1.,0.,0.));
#10929=DIRECTION('ref_axis',(0.,-0.707106781186547,0.707106781186547));
#10930=DIRECTION('',(1.,0.,0.));
#10931=DIRECTION('center_axis',(-1.,0.,0.));
#10932=DIRECTION('ref_axis',(0.,-0.707106781186548,0.707106781186548));
#10933=DIRECTION('',(1.,0.,0.));
#10934=DIRECTION('',(1.,0.,0.));
#10935=DIRECTION('center_axis',(0.,-0.707106781186548,0.707106781186548));
#10936=DIRECTION('ref_axis',(1.22464679914735E-16,-0.707106781186548,-0.707106781186548));
#10937=DIRECTION('center_axis',(-0.602056836120681,-0.564591695865408,-0.564591695865409));
#10938=DIRECTION('ref_axis',(-0.797776104275146,0.454472584285347,0.396242296556752));
#10939=DIRECTION('center_axis',(0.602056836120562,-0.564591695865472,-0.564591695865472));
#10940=DIRECTION('ref_axis',(0.797776104275237,0.396242296556694,0.454472584285238));
#10941=DIRECTION('center_axis',(-1.,0.,0.));
#10942=DIRECTION('ref_axis',(0.,-0.707106781186548,0.707106781186548));
#10943=DIRECTION('',(1.,0.,0.));
#10944=DIRECTION('center_axis',(-1.,0.,0.));
#10945=DIRECTION('ref_axis',(0.,-0.707106781186548,0.707106781186548));
#10946=DIRECTION('',(1.,0.,0.));
#10947=DIRECTION('center_axis',(-1.,0.,0.));
#10948=DIRECTION('ref_axis',(0.,-0.707106781186548,0.707106781186548));
#10949=DIRECTION('',(1.,0.,0.));
#10950=DIRECTION('center_axis',(-1.,0.,0.));
#10951=DIRECTION('ref_axis',(0.,-0.707106781186547,0.707106781186547));
#10952=DIRECTION('center_axis',(-1.,0.,0.));
#10953=DIRECTION('ref_axis',(0.,-0.923879532511285,0.382683432365094));
#10954=DIRECTION('',(1.,0.,0.));
#10955=DIRECTION('center_axis',(-1.,0.,0.));
#10956=DIRECTION('ref_axis',(0.,-0.923879532511285,0.382683432365094));
#10957=DIRECTION('',(1.,0.,0.));
#10958=DIRECTION('',(1.,0.,0.));
#10959=DIRECTION('center_axis',(0.,-0.923879532511285,0.382683432365094));
#10960=DIRECTION('ref_axis',(1.22464679914735E-16,-0.382683432365094,-0.923879532511285));
#10961=DIRECTION('center_axis',(-0.602056836120692,-0.305554823977286,-0.737674600094481));
#10962=DIRECTION('ref_axis',(-0.797776104275363,0.268242556607946,0.539999276176976));
#10963=DIRECTION('center_axis',(0.60205683612067,-0.305554823977293,-0.737674600094496));
#10964=DIRECTION('ref_axis',(0.797776104275269,0.192161019237087,0.571513280802064));
#10965=DIRECTION('center_axis',(-1.,0.,0.));
#10966=DIRECTION('ref_axis',(0.,-0.923879532511285,0.382683432365094));
#10967=DIRECTION('',(1.,0.,0.));
#10968=DIRECTION('center_axis',(-1.,0.,0.));
#10969=DIRECTION('ref_axis',(0.,-0.923879532511285,0.382683432365094));
#10970=DIRECTION('',(1.,0.,0.));
#10971=DIRECTION('center_axis',(-1.,0.,0.));
#10972=DIRECTION('ref_axis',(0.,-0.923879532511285,0.382683432365094));
#10973=DIRECTION('',(1.,0.,0.));
#10974=DIRECTION('center_axis',(-1.,0.,0.));
#10975=DIRECTION('ref_axis',(0.,-0.923879532511285,0.382683432365094));
#10976=DIRECTION('center_axis',(-1.,0.,0.));
#10977=DIRECTION('ref_axis',(0.,-1.,0.));
#10978=DIRECTION('',(1.,0.,0.));
#10979=DIRECTION('center_axis',(-1.,0.,0.));
#10980=DIRECTION('ref_axis',(0.,-1.,0.));
#10981=DIRECTION('',(1.,0.,0.));
#10982=DIRECTION('',(1.,0.,0.));
#10983=DIRECTION('center_axis',(0.,-1.,0.));
#10984=DIRECTION('ref_axis',(1.22464679914735E-16,0.,-1.));
#10985=DIRECTION('center_axis',(-0.602056836120766,0.,-0.798453233496022));
#10986=DIRECTION('ref_axis',(-0.797776104274988,0.0411750313262452,0.601546261099765));
#10987=DIRECTION('center_axis',(0.602056836120813,0.,-0.798453233495987));
#10988=DIRECTION('ref_axis',(0.797776104274953,-0.0411750313262546,0.601546261099811));
#10989=DIRECTION('center_axis',(-1.,0.,0.));
#10990=DIRECTION('ref_axis',(0.,-1.,0.));
#10991=DIRECTION('',(1.,0.,0.));
#10992=DIRECTION('center_axis',(-1.,0.,0.));
#10993=DIRECTION('ref_axis',(0.,-1.,0.));
#10994=DIRECTION('',(1.,0.,0.));
#10995=DIRECTION('center_axis',(-1.,0.,0.));
#10996=DIRECTION('ref_axis',(0.,-1.,0.));
#10997=DIRECTION('',(1.,0.,0.));
#10998=DIRECTION('center_axis',(-1.,0.,0.));
#10999=DIRECTION('ref_axis',(0.,-1.,0.));
#11000=DIRECTION('center_axis',(-1.,0.,0.));
#11001=DIRECTION('ref_axis',(0.,-0.923879532511285,-0.382683432365094));
#11002=DIRECTION('',(1.,0.,0.));
#11003=DIRECTION('center_axis',(-1.,0.,0.));
#11004=DIRECTION('ref_axis',(0.,-0.923879532511285,-0.382683432365094));
#11005=DIRECTION('',(1.,0.,0.));
#11006=DIRECTION('',(1.,0.,0.));
#11007=DIRECTION('center_axis',(0.,-0.923879532511285,-0.382683432365094));
#11008=DIRECTION('ref_axis',(1.22464679914735E-16,0.382683432365094,-0.923879532511285));
#11009=DIRECTION('center_axis',(-0.602056836120556,0.305554823977325,-0.737674600094575));
#11010=DIRECTION('ref_axis',(-0.797776104275275,-0.192161019234803,0.571513280802823));
#11011=DIRECTION('center_axis',(0.602056836120892,0.30555482397723,-0.737674600094341));
#11012=DIRECTION('ref_axis',(0.797776104275135,-0.268242556610213,0.539999276176187));
#11013=DIRECTION('center_axis',(-1.,0.,0.));
#11014=DIRECTION('ref_axis',(0.,-0.923879532511285,-0.382683432365094));
#11015=DIRECTION('',(1.,0.,0.));
#11016=DIRECTION('center_axis',(-1.,0.,0.));
#11017=DIRECTION('ref_axis',(0.,-0.923879532511285,-0.382683432365094));
#11018=DIRECTION('',(1.,0.,0.));
#11019=DIRECTION('center_axis',(-1.,0.,0.));
#11020=DIRECTION('ref_axis',(0.,-0.923879532511285,-0.382683432365094));
#11021=DIRECTION('',(1.,0.,0.));
#11022=DIRECTION('center_axis',(-1.,0.,0.));
#11023=DIRECTION('ref_axis',(0.,-0.923879532511285,-0.382683432365094));
#11024=DIRECTION('center_axis',(-1.,0.,0.));
#11025=DIRECTION('ref_axis',(0.,-0.707106781186547,-0.707106781186547));
#11026=DIRECTION('',(1.,0.,0.));
#11027=DIRECTION('center_axis',(-1.,0.,0.));
#11028=DIRECTION('ref_axis',(0.,-0.707106781186548,-0.707106781186548));
#11029=DIRECTION('',(1.,0.,0.));
#11030=DIRECTION('',(1.,0.,0.));
#11031=DIRECTION('center_axis',(0.,-0.707106781186548,-0.707106781186548));
#11032=DIRECTION('ref_axis',(1.22464679914735E-16,0.707106781186548,-0.707106781186548));
#11033=DIRECTION('center_axis',(-0.602056836120681,0.564591695865409,-0.564591695865408));
#11034=DIRECTION('ref_axis',(-0.797776104275146,-0.396242296556752,0.454472584285347));
#11035=DIRECTION('center_axis',(0.602056836120562,0.564591695865472,-0.564591695865472));
#11036=DIRECTION('ref_axis',(0.797776104275237,-0.454472584285238,0.396242296556694));
#11037=DIRECTION('center_axis',(-1.,0.,0.));
#11038=DIRECTION('ref_axis',(0.,-0.707106781186548,-0.707106781186548));
#11039=DIRECTION('',(1.,0.,0.));
#11040=DIRECTION('center_axis',(-1.,0.,0.));
#11041=DIRECTION('ref_axis',(0.,-0.707106781186548,-0.707106781186548));
#11042=DIRECTION('',(1.,0.,0.));
#11043=DIRECTION('center_axis',(-1.,0.,0.));
#11044=DIRECTION('ref_axis',(0.,-0.707106781186548,-0.707106781186548));
#11045=DIRECTION('',(1.,0.,0.));
#11046=DIRECTION('center_axis',(-1.,0.,0.));
#11047=DIRECTION('ref_axis',(0.,-0.707106781186547,-0.707106781186547));
#11048=DIRECTION('center_axis',(-1.,0.,0.));
#11049=DIRECTION('ref_axis',(0.,-0.382683432365094,-0.923879532511285));
#11050=DIRECTION('',(1.,0.,0.));
#11051=DIRECTION('center_axis',(-1.,0.,0.));
#11052=DIRECTION('ref_axis',(0.,-0.382683432365094,-0.923879532511285));
#11053=DIRECTION('',(1.,0.,0.));
#11054=DIRECTION('',(1.,0.,0.));
#11055=DIRECTION('center_axis',(0.,-0.382683432365094,-0.923879532511285));
#11056=DIRECTION('ref_axis',(1.22464679914735E-16,0.923879532511285,-0.382683432365094));
#11057=DIRECTION('center_axis',(-0.602056836120692,0.73767460009448,-0.305554823977286));
#11058=DIRECTION('ref_axis',(-0.797776104275363,-0.539999276176976,0.268242556607946));
#11059=DIRECTION('center_axis',(0.60205683612067,0.737674600094496,-0.305554823977293));
#11060=DIRECTION('ref_axis',(0.797776104275269,-0.571513280802065,0.192161019237087));
#11061=DIRECTION('center_axis',(-1.,0.,0.));
#11062=DIRECTION('ref_axis',(0.,-0.382683432365094,-0.923879532511285));
#11063=DIRECTION('',(1.,0.,0.));
#11064=DIRECTION('center_axis',(-1.,0.,0.));
#11065=DIRECTION('ref_axis',(0.,-0.382683432365094,-0.923879532511285));
#11066=DIRECTION('',(1.,0.,0.));
#11067=DIRECTION('center_axis',(-1.,0.,0.));
#11068=DIRECTION('ref_axis',(0.,-0.382683432365094,-0.923879532511285));
#11069=DIRECTION('',(1.,0.,0.));
#11070=DIRECTION('center_axis',(-1.,0.,0.));
#11071=DIRECTION('ref_axis',(0.,-0.382683432365094,-0.923879532511285));
#11072=DIRECTION('center_axis',(-1.,0.,0.));
#11073=DIRECTION('ref_axis',(0.,0.,-1.));
#11074=DIRECTION('',(1.,0.,0.));
#11075=DIRECTION('center_axis',(-1.,0.,0.));
#11076=DIRECTION('ref_axis',(0.,0.,-1.));
#11077=DIRECTION('',(1.,0.,0.));
#11078=DIRECTION('',(1.,0.,0.));
#11079=DIRECTION('center_axis',(0.,0.,-1.));
#11080=DIRECTION('ref_axis',(1.22464679914735E-16,1.,0.));
#11081=DIRECTION('center_axis',(-0.602056836120766,0.798453233496022,0.));
#11082=DIRECTION('ref_axis',(-0.797776104274987,-0.601546261099765,0.0411750313262641));
#11083=DIRECTION('center_axis',(0.602056836120813,0.798453233495987,0.));
#11084=DIRECTION('ref_axis',(0.797776104274952,-0.60154626109981,-0.0411750313262736));
#11085=DIRECTION('center_axis',(-1.,0.,0.));
#11086=DIRECTION('ref_axis',(0.,0.,-1.));
#11087=DIRECTION('',(1.,0.,0.));
#11088=DIRECTION('center_axis',(-1.,0.,0.));
#11089=DIRECTION('ref_axis',(0.,0.,-1.));
#11090=DIRECTION('',(1.,0.,0.));
#11091=DIRECTION('center_axis',(-1.,0.,0.));
#11092=DIRECTION('ref_axis',(0.,0.,-1.));
#11093=DIRECTION('',(1.,0.,0.));
#11094=DIRECTION('center_axis',(-1.,0.,0.));
#11095=DIRECTION('ref_axis',(0.,0.,-1.));
#11096=DIRECTION('center_axis',(-1.,0.,0.));
#11097=DIRECTION('ref_axis',(0.,0.382683432365094,-0.923879532511285));
#11098=DIRECTION('',(1.,0.,0.));
#11099=DIRECTION('center_axis',(-1.,0.,0.));
#11100=DIRECTION('ref_axis',(0.,0.382683432365094,-0.923879532511285));
#11101=DIRECTION('',(1.,0.,0.));
#11102=DIRECTION('',(1.,0.,0.));
#11103=DIRECTION('center_axis',(0.,0.382683432365094,-0.923879532511285));
#11104=DIRECTION('ref_axis',(1.22464679914735E-16,0.923879532511285,0.382683432365094));
#11105=DIRECTION('center_axis',(-0.602056836120637,0.737674600094518,0.305554823977304));
#11106=DIRECTION('ref_axis',(-0.797776104275215,-0.571513280802905,-0.192161019234811));
#11107=DIRECTION('center_axis',(0.60205683612087,0.737674600094356,0.305554823977236));
#11108=DIRECTION('ref_axis',(0.797776104275151,-0.539999276176162,-0.268242556610214));
#11109=DIRECTION('center_axis',(-1.,0.,0.));
#11110=DIRECTION('ref_axis',(0.,0.382683432365094,-0.923879532511285));
#11111=DIRECTION('',(1.,0.,0.));
#11112=DIRECTION('center_axis',(-1.,0.,0.));
#11113=DIRECTION('ref_axis',(0.,0.382683432365094,-0.923879532511285));
#11114=DIRECTION('',(1.,0.,0.));
#11115=DIRECTION('center_axis',(-1.,0.,0.));
#11116=DIRECTION('ref_axis',(0.,0.382683432365094,-0.923879532511285));
#11117=DIRECTION('',(1.,0.,0.));
#11118=DIRECTION('center_axis',(-1.,0.,0.));
#11119=DIRECTION('ref_axis',(0.,0.382683432365094,-0.923879532511285));
#11120=DIRECTION('center_axis',(-1.,0.,0.));
#11121=DIRECTION('ref_axis',(0.,0.707106781186547,-0.707106781186547));
#11122=DIRECTION('',(1.,0.,0.));
#11123=DIRECTION('center_axis',(-1.,0.,0.));
#11124=DIRECTION('ref_axis',(0.,0.707106781186548,-0.707106781186548));
#11125=DIRECTION('',(1.,0.,0.));
#11126=DIRECTION('',(1.,0.,0.));
#11127=DIRECTION('center_axis',(0.,0.707106781186548,-0.707106781186548));
#11128=DIRECTION('ref_axis',(1.22464679914735E-16,0.707106781186548,0.707106781186548));
#11129=DIRECTION('center_axis',(-0.602056836120681,0.564591695865408,0.564591695865409));
#11130=DIRECTION('ref_axis',(-0.797776104275146,-0.454472584285347,-0.396242296556752));
#11131=DIRECTION('center_axis',(0.602056836120562,0.564591695865472,0.564591695865472));
#11132=DIRECTION('ref_axis',(0.797776104275237,-0.396242296556694,-0.454472584285238));
#11133=DIRECTION('center_axis',(-1.,0.,0.));
#11134=DIRECTION('ref_axis',(0.,0.707106781186548,-0.707106781186548));
#11135=DIRECTION('',(1.,0.,0.));
#11136=DIRECTION('center_axis',(-1.,0.,0.));
#11137=DIRECTION('ref_axis',(0.,0.707106781186548,-0.707106781186548));
#11138=DIRECTION('',(1.,0.,0.));
#11139=DIRECTION('center_axis',(-1.,0.,0.));
#11140=DIRECTION('ref_axis',(0.,0.707106781186548,-0.707106781186548));
#11141=DIRECTION('',(1.,0.,0.));
#11142=DIRECTION('center_axis',(-1.,0.,0.));
#11143=DIRECTION('ref_axis',(0.,0.707106781186547,-0.707106781186547));
#11144=DIRECTION('center_axis',(-1.,0.,0.));
#11145=DIRECTION('ref_axis',(0.,0.923879532511285,-0.382683432365094));
#11146=DIRECTION('',(1.,0.,0.));
#11147=DIRECTION('center_axis',(-1.,0.,0.));
#11148=DIRECTION('ref_axis',(0.,0.923879532511285,-0.382683432365094));
#11149=DIRECTION('',(1.,0.,0.));
#11150=DIRECTION('',(1.,0.,0.));
#11151=DIRECTION('center_axis',(0.,0.923879532511285,-0.382683432365094));
#11152=DIRECTION('ref_axis',(-7.6571373978539E-16,0.382683432365094,0.923879532511285));
#11153=DIRECTION('center_axis',(-0.602056836120741,0.305554823977272,0.737674600094446));
#11154=DIRECTION('ref_axis',(-0.797776104275203,-0.26824255661142,-0.539999276175487));
#11155=DIRECTION('center_axis',(0.602056836120943,0.305554823977215,0.737674600094305));
#11156=DIRECTION('ref_axis',(0.797776104274938,-0.192161019233689,-0.571513280803669));
#11157=DIRECTION('center_axis',(-1.,0.,0.));
#11158=DIRECTION('ref_axis',(0.,0.923879532511285,-0.382683432365094));
#11159=DIRECTION('',(1.,0.,0.));
#11160=DIRECTION('',(1.,0.,0.));
#11161=DIRECTION('',(1.,0.,0.));
#11162=DIRECTION('center_axis',(-1.,0.,0.));
#11163=DIRECTION('ref_axis',(0.,0.923879532511285,-0.382683432365094));
#11164=DIRECTION('center_axis',(-1.,0.,0.));
#11165=DIRECTION('ref_axis',(0.,0.923879532511285,-0.382683432365094));
#11166=DIRECTION('center_axis',(-1.,0.,0.));
#11167=DIRECTION('ref_axis',(0.,0.923879532511285,-0.382683432365094));
#11168=DIRECTION('axis',(0.,0.,1.));
#11169=DIRECTION('refdir',(1.,0.,0.));
#11170=DIRECTION('center_axis',(0.,0.,-1.));
#11171=DIRECTION('ref_axis',(0.,-1.,0.));
#11172=DIRECTION('center_axis',(0.,0.,1.));
#11173=DIRECTION('ref_axis',(0.,1.,0.));
#11174=DIRECTION('',(0.866025403784429,0.500000000000017,0.));
#11175=DIRECTION('',(0.,1.,0.));
#11176=DIRECTION('',(-0.866025403784429,0.500000000000017,0.));
#11177=DIRECTION('',(-0.866025403784429,-0.500000000000017,0.));
#11178=DIRECTION('',(0.,-1.,0.));
#11179=DIRECTION('',(0.866025403784429,-0.500000000000017,0.));
#11180=DIRECTION('center_axis',(0.,0.,-1.));
#11181=DIRECTION('ref_axis',(0.,-1.,0.));
#11182=DIRECTION('',(0.,0.,1.));
#11183=DIRECTION('center_axis',(0.,0.,-1.));
#11184=DIRECTION('ref_axis',(0.,-1.,0.));
#11185=DIRECTION('center_axis',(0.,0.,-1.));
#11186=DIRECTION('ref_axis',(0.,-1.,0.));
#11187=DIRECTION('center_axis',(0.,0.,-1.));
#11188=DIRECTION('ref_axis',(0.,-1.,0.));
#11189=DIRECTION('',(0.,0.,1.));
#11190=DIRECTION('center_axis',(0.,0.,-1.));
#11191=DIRECTION('ref_axis',(0.,-1.,0.));
#11192=DIRECTION('center_axis',(0.,0.,-1.));
#11193=DIRECTION('ref_axis',(0.,-1.,0.));
#11194=DIRECTION('center_axis',(-1.,1.22464679914735E-16,0.));
#11195=DIRECTION('ref_axis',(1.22464679914735E-16,1.,0.));
#11196=DIRECTION('center_axis',(0.,-6.12323399573677E-17,-1.));
#11197=DIRECTION('ref_axis',(0.,-1.,0.));
#11198=DIRECTION('center_axis',(1.,-1.22464679914735E-16,0.));
#11199=DIRECTION('ref_axis',(1.22464679914735E-16,1.,0.));
#11200=DIRECTION('center_axis',(1.,0.,0.));
#11201=DIRECTION('ref_axis',(0.,-1.,0.));
#11202=DIRECTION('',(1.,0.,0.));
#11203=DIRECTION('center_axis',(-0.500000000000017,0.866025403784429,0.));
#11204=DIRECTION('ref_axis',(0.866025403784429,0.500000000000017,0.));
#11205=DIRECTION('',(0.,0.,-1.));
#11206=DIRECTION('',(0.866025403784429,0.500000000000017,0.));
#11207=DIRECTION('',(0.,0.,-1.));
#11208=DIRECTION('center_axis',(-1.,0.,0.));
#11209=DIRECTION('ref_axis',(0.,1.,0.));
#11210=DIRECTION('',(0.,1.,0.));
#11211=DIRECTION('',(0.,0.,-1.));
#11212=DIRECTION('center_axis',(-0.500000000000017,-0.866025403784429,0.));
#11213=DIRECTION('ref_axis',(-0.866025403784429,0.500000000000017,0.));
#11214=DIRECTION('',(-0.866025403784429,0.500000000000017,0.));
#11215=DIRECTION('',(0.,0.,-1.));
#11216=DIRECTION('center_axis',(0.500000000000017,-0.866025403784429,0.));
#11217=DIRECTION('ref_axis',(-0.866025403784429,-0.500000000000017,0.));
#11218=DIRECTION('',(-0.866025403784429,-0.500000000000017,0.));
#11219=DIRECTION('',(0.,0.,-1.));
#11220=DIRECTION('center_axis',(1.,0.,0.));
#11221=DIRECTION('ref_axis',(0.,-1.,0.));
#11222=DIRECTION('',(0.,-1.,0.));
#11223=DIRECTION('',(0.,0.,-1.));
#11224=DIRECTION('center_axis',(0.500000000000017,0.866025403784429,0.));
#11225=DIRECTION('ref_axis',(0.866025403784429,-0.500000000000017,0.));
#11226=DIRECTION('',(0.866025403784429,-0.500000000000017,0.));
#11227=DIRECTION('center_axis',(0.,0.,-1.));
#11228=DIRECTION('ref_axis',(0.,-1.,0.));
#11229=DIRECTION('center_axis',(0.,0.,-1.));
#11230=DIRECTION('ref_axis',(0.,-1.,0.));
#11231=DIRECTION('',(0.,1.,0.));
#11232=DIRECTION('center_axis',(0.,0.,-1.));
#11233=DIRECTION('ref_axis',(0.,-1.,0.));
#11234=DIRECTION('',(0.,0.,-1.));
#11235=DIRECTION('',(-0.50903696045512,0.700629269222028,-0.50000000000002));
#11236=DIRECTION('',(0.50903696045512,-0.700629269222028,-0.50000000000002));
#11237=DIRECTION('',(0.,0.,-1.));
#11238=DIRECTION('',(0.,0.,-1.));
#11239=DIRECTION('',(0.,0.,-1.));
#11240=DIRECTION('',(0.,0.,-1.));
#11241=DIRECTION('center_axis',(-1.,0.,0.));
#11242=DIRECTION('ref_axis',(0.,1.,0.));
#11243=DIRECTION('',(0.,1.,0.));
#11244=DIRECTION('',(0.,0.,-1.));
#11245=DIRECTION('center_axis',(0.,0.,-1.));
#11246=DIRECTION('ref_axis',(0.,-1.,0.));
#11247=DIRECTION('center_axis',(0.,0.,-1.));
#11248=DIRECTION('ref_axis',(-0.916187957117145,-0.40074883310312,0.));
#11249=DIRECTION('',(-0.50903696045512,-0.700629269222028,-0.50000000000002));
#11250=DIRECTION('center_axis',(0.,0.,-1.));
#11251=DIRECTION('ref_axis',(0.548802039292154,0.835952344137375,0.));
#11252=DIRECTION('',(0.50903696045512,0.700629269222028,-0.50000000000002));
#11253=DIRECTION('',(-0.823639103546326,-0.267616567329808,-0.500000000000015));
#11254=DIRECTION('',(0.823639103546326,0.267616567329808,-0.500000000000015));
#11255=DIRECTION('',(-0.823639103546326,0.267616567329808,-0.500000000000015));
#11256=DIRECTION('',(0.823639103546326,-0.267616567329808,-0.500000000000015));
#11257=DIRECTION('center_axis',(-1.,0.,0.));
#11258=DIRECTION('ref_axis',(0.,1.,0.));
#11259=DIRECTION('axis',(0.,0.,1.));
#11260=DIRECTION('refdir',(1.,0.,0.));
#11261=DIRECTION('center_axis',(0.,1.,0.));
#11262=DIRECTION('ref_axis',(1.,0.,0.));
#11263=DIRECTION('center_axis',(0.,-1.,0.));
#11264=DIRECTION('ref_axis',(1.,0.,0.));
#11265=DIRECTION('center_axis',(0.,-1.,0.));
#11266=DIRECTION('ref_axis',(1.,0.,0.));
#11267=DIRECTION('center_axis',(0.,1.,0.));
#11268=DIRECTION('ref_axis',(1.,0.,0.));
#11269=DIRECTION('',(0.,1.,0.));
#11270=DIRECTION('center_axis',(0.,-1.,0.));
#11271=DIRECTION('ref_axis',(1.,0.,0.));
#11272=DIRECTION('center_axis',(0.,1.,0.));
#11273=DIRECTION('ref_axis',(1.,0.,0.));
#11274=DIRECTION('center_axis',(0.,1.,0.));
#11275=DIRECTION('ref_axis',(-1.,0.,0.));
#11276=DIRECTION('center_axis',(0.,1.,0.));
#11277=DIRECTION('ref_axis',(-0.999990518102908,0.,-0.00435473354849803));
#11278=DIRECTION('center_axis',(0.00435473354849791,0.,-0.999990518102908));
#11279=DIRECTION('ref_axis',(0.999990518102908,0.,0.00435473354849791));
#11280=DIRECTION('axis',(0.,0.,1.));
#11281=DIRECTION('refdir',(1.,0.,0.));
#11282=DIRECTION('center_axis',(0.,0.,1.));
#11283=DIRECTION('ref_axis',(0.,1.,0.));
#11284=DIRECTION('',(-4.18853873767699E-17,0.342020143325669,-0.939692620785908));
#11285=DIRECTION('center_axis',(0.,0.,1.));
#11286=DIRECTION('ref_axis',(-0.901991229138518,0.431754354416009,0.));
#11287=DIRECTION('center_axis',(0.,0.,1.));
#11288=DIRECTION('ref_axis',(0.,1.,0.));
#11289=DIRECTION('center_axis',(0.,0.,1.));
#11290=DIRECTION('ref_axis',(0.,1.,0.));
#11291=DIRECTION('center_axis',(0.,0.,1.));
#11292=DIRECTION('ref_axis',(-0.180387890266709,-0.983595551558223,0.));
#11293=DIRECTION('',(0.,0.,1.));
#11294=DIRECTION('center_axis',(0.,0.,1.));
#11295=DIRECTION('ref_axis',(0.,1.,0.));
#11296=DIRECTION('',(0.,0.,-1.));
#11297=DIRECTION('',(0.,-0.866025403784429,0.500000000000017));
#11298=DIRECTION('',(0.,-0.866025403784429,-0.500000000000017));
#11299=DIRECTION('center_axis',(0.,0.,-1.));
#11300=DIRECTION('ref_axis',(0.,-1.,0.));
#11301=DIRECTION('',(0.,0.866025403784429,-0.500000000000017));
#11302=DIRECTION('',(0.,-0.866025403784429,-0.500000000000017));
#11303=DIRECTION('',(0.,0.,-1.));
#11304=DIRECTION('',(0.,0.866025403784429,-0.500000000000017));
#11305=DIRECTION('',(0.,0.866025403784429,-0.500000000000017));
#11306=DIRECTION('',(0.,0.,-1.));
#11307=DIRECTION('',(0.,-0.866025403784429,-0.500000000000017));
#11308=DIRECTION('center_axis',(0.,0.,1.));
#11309=DIRECTION('ref_axis',(0.,1.,0.));
#11310=DIRECTION('center_axis',(1.,0.,0.));
#11311=DIRECTION('ref_axis',(0.,-0.939692620785897,0.342020143325699));
#11312=DIRECTION('center_axis',(0.,0.,1.));
#11313=DIRECTION('ref_axis',(-0.901991229138518,0.431754354416009,0.));
#11314=DIRECTION('center_axis',(-1.,-1.22464679914735E-16,0.));
#11315=DIRECTION('ref_axis',(1.22464679914735E-16,-1.,0.));
#11316=DIRECTION('center_axis',(0.,0.,1.));
#11317=DIRECTION('ref_axis',(0.,1.,0.));
#11318=DIRECTION('center_axis',(0.,0.,1.));
#11319=DIRECTION('ref_axis',(0.,1.,0.));
#11320=DIRECTION('',(0.,0.342020143325699,0.939692620785897));
#11321=DIRECTION('center_axis',(1.,0.,0.));
#11322=DIRECTION('ref_axis',(0.,-1.,0.));
#11323=DIRECTION('center_axis',(0.,0.,1.));
#11324=DIRECTION('ref_axis',(0.,1.,0.));
#11325=DIRECTION('center_axis',(0.,0.,1.));
#11326=DIRECTION('ref_axis',(0.,1.,0.));
#11327=DIRECTION('center_axis',(0.,0.,1.));
#11328=DIRECTION('ref_axis',(0.,1.,0.));
#11329=DIRECTION('',(0.,0.,-1.));
#11330=DIRECTION('center_axis',(0.,0.,1.));
#11331=DIRECTION('ref_axis',(0.,1.,0.));
#11332=DIRECTION('center_axis',(0.,0.,1.));
#11333=DIRECTION('ref_axis',(0.,1.,0.));
#11334=DIRECTION('center_axis',(0.,0.,-1.));
#11335=DIRECTION('ref_axis',(0.889042601598659,-0.457824477876279,0.));
#11336=DIRECTION('center_axis',(0.996194698083924,0.,0.0871557428370583));
#11337=DIRECTION('ref_axis',(-1.12154994191049E-8,-0.999999999999992,1.28193744829457E-7));
#11338=DIRECTION('center_axis',(0.996194698083924,0.,0.0871557428370583));
#11339=DIRECTION('ref_axis',(-1.12154994191049E-8,-0.999999999999992,1.28193744829457E-7));
#11340=DIRECTION('center_axis',(0.,0.,-1.));
#11341=DIRECTION('ref_axis',(0.457824477876279,0.889042601598659,0.));
#11342=DIRECTION('center_axis',(0.,0.,1.));
#11343=DIRECTION('ref_axis',(-0.457824477876279,0.889042601598659,0.));
#11344=DIRECTION('center_axis',(-0.996194698083924,0.,0.0871557428370583));
#11345=DIRECTION('ref_axis',(-1.12154878567642E-8,-0.999999999999992,-1.28193612671298E-7));
#11346=DIRECTION('center_axis',(0.,0.,1.));
#11347=DIRECTION('ref_axis',(-0.889042601598659,-0.457824477876279,0.));
#11348=DIRECTION('center_axis',(0.996194698091745,0.,0.087155742747664));
#11349=DIRECTION('ref_axis',(0.,-1.,0.));
#11350=DIRECTION('',(-0.0868265938642471,0.0868265938642471,0.992432509138967));
#11351=DIRECTION('',(0.,-1.,0.));
#11352=DIRECTION('',(-0.0868265938642471,-0.0868265938642471,0.992432509138967));
#11353=DIRECTION('center_axis',(-0.0868265938642471,0.0868265938642471,
0.992432509138967));
#11354=DIRECTION('ref_axis',(5.403663627668E-16,-0.996194698091746,0.0871557427476577));
#11355=DIRECTION('center_axis',(0.,0.,-1.));
#11356=DIRECTION('ref_axis',(0.707106781186546,-0.707106781186549,0.));
#11357=DIRECTION('',(-0.0868265938642471,0.0868265938642471,0.992432509138967));
#11358=DIRECTION('center_axis',(0.,0.,-1.));
#11359=DIRECTION('ref_axis',(0.,1.,0.));
#11360=DIRECTION('',(0.,1.,0.));
#11361=DIRECTION('center_axis',(0.,0.,-1.));
#11362=DIRECTION('ref_axis',(-0.707106781186546,0.707106781186549,0.));
#11363=DIRECTION('',(1.,0.,0.));
#11364=DIRECTION('center_axis',(0.,0.,-1.));
#11365=DIRECTION('ref_axis',(0.707106781186549,0.707106781186546,0.));
#11366=DIRECTION('',(0.,-1.,0.));
#11367=DIRECTION('center_axis',(0.,0.,1.));
#11368=DIRECTION('ref_axis',(-0.707106781186546,-0.707106781186549,0.));
#11369=DIRECTION('',(1.,0.,0.));
#11370=DIRECTION('center_axis',(0.,0.,-1.));
#11371=DIRECTION('ref_axis',(0.707106781186549,0.707106781186546,0.));
#11372=DIRECTION('',(-1.,0.,0.));
#11373=DIRECTION('center_axis',(0.,0.,1.));
#11374=DIRECTION('ref_axis',(-0.707106781186549,0.707106781186546,0.));
#11375=DIRECTION('',(0.,-1.,0.));
#11376=DIRECTION('center_axis',(0.,0.,-1.));
#11377=DIRECTION('ref_axis',(0.707106781186546,-0.707106781186549,0.));
#11378=DIRECTION('',(-1.,0.,0.));
#11379=DIRECTION('center_axis',(0.,0.,-1.));
#11380=DIRECTION('ref_axis',(-0.707106781186549,-0.707106781186546,0.));
#11381=DIRECTION('',(0.,1.,0.));
#11382=DIRECTION('center_axis',(0.,0.,1.));
#11383=DIRECTION('ref_axis',(0.707106781186546,0.707106781186549,0.));
#11384=DIRECTION('',(-1.,0.,0.));
#11385=DIRECTION('center_axis',(0.,0.,-1.));
#11386=DIRECTION('ref_axis',(-0.707106781186549,-0.707106781186546,0.));
#11387=DIRECTION('',(0.,1.,0.));
#11388=DIRECTION('center_axis',(0.,0.,-1.));
#11389=DIRECTION('ref_axis',(-0.707106781186546,0.707106781186549,0.));
#11390=DIRECTION('',(1.,0.,0.));
#11391=DIRECTION('center_axis',(0.,0.,1.));
#11392=DIRECTION('ref_axis',(0.707106781186549,-0.707106781186546,0.));
#11393=DIRECTION('center_axis',(-0.996194698091745,0.,0.087155742747664));
#11394=DIRECTION('ref_axis',(0.,1.,0.));
#11395=DIRECTION('',(0.,1.,0.));
#11396=DIRECTION('',(0.0868265938642471,-0.0868265938642471,0.992432509138967));
#11397=DIRECTION('',(-0.0868265938642471,0.0868265938642471,-0.992432509138967));
#11398=DIRECTION('center_axis',(0.,0.,1.));
#11399=DIRECTION('ref_axis',(0.,1.,0.));
#11400=DIRECTION('',(0.,-1.,0.));
#11401=DIRECTION('',(1.,0.,0.));
#11402=DIRECTION('center_axis',(0.,0.,-1.));
#11403=DIRECTION('ref_axis',(-0.707106781186546,-0.707106781186549,0.));
#11404=DIRECTION('center_axis',(0.,0.,1.));
#11405=DIRECTION('ref_axis',(0.,1.,0.));
#11406=DIRECTION('',(-1.,0.,0.));
#11407=DIRECTION('',(0.,-1.,0.));
#11408=DIRECTION('center_axis',(0.,0.,-1.));
#11409=DIRECTION('ref_axis',(-0.707106781186549,0.707106781186546,0.));
#11410=DIRECTION('center_axis',(0.,0.,1.));
#11411=DIRECTION('ref_axis',(0.,1.,0.));
#11412=DIRECTION('',(0.,1.,0.));
#11413=DIRECTION('',(-1.,0.,0.));
#11414=DIRECTION('center_axis',(0.,0.,-1.));
#11415=DIRECTION('ref_axis',(0.707106781186546,0.707106781186549,0.));
#11416=DIRECTION('center_axis',(0.,0.,1.));
#11417=DIRECTION('ref_axis',(0.,1.,0.));
#11418=DIRECTION('',(1.,0.,0.));
#11419=DIRECTION('center_axis',(0.,0.,-1.));
#11420=DIRECTION('ref_axis',(0.707106781186549,-0.707106781186546,0.));
#11421=DIRECTION('center_axis',(0.996194698091745,0.,0.087155742747664));
#11422=DIRECTION('ref_axis',(0.,-1.,0.));
#11423=DIRECTION('',(0.0868265938642471,0.0868265938642471,-0.992432509138967));
#11424=DIRECTION('',(-0.0868265938642471,-0.0868265938642471,0.992432509138967));
#11425=DIRECTION('center_axis',(-0.0868265938642471,-0.0868265938642471,
0.992432509138967));
#11426=DIRECTION('ref_axis',(0.996194698091746,5.403663627668E-16,0.0871557427476577));
#11427=DIRECTION('',(-0.0868265938642471,-0.0868265938642471,0.992432509138967));
#11428=DIRECTION('center_axis',(0.,0.996194698091745,0.087155742747664));
#11429=DIRECTION('ref_axis',(1.,0.,0.));
#11430=DIRECTION('',(0.0868265938642471,-0.0868265938642471,0.992432509138967));
#11431=DIRECTION('center_axis',(0.0868265938642471,-0.0868265938642471,
0.992432509138967));
#11432=DIRECTION('ref_axis',(-5.403663627668E-16,0.996194698091746,0.0871557427476577));
#11433=DIRECTION('center_axis',(-0.996194698091745,0.,0.087155742747664));
#11434=DIRECTION('ref_axis',(0.,1.,0.));
#11435=DIRECTION('',(0.0868265938642471,-0.0868265938642471,0.992432509138967));
#11436=DIRECTION('',(0.0868265938642471,0.0868265938642471,0.992432509138967));
#11437=DIRECTION('center_axis',(0.0868265938642471,-0.0868265938642471,
0.992432509138967));
#11438=DIRECTION('ref_axis',(-5.403663627668E-16,0.996194698091746,0.0871557427476577));
#11439=DIRECTION('',(0.0868265938642471,-0.0868265938642471,0.992432509138967));
#11440=DIRECTION('center_axis',(0.,0.996194698091745,0.087155742747664));
#11441=DIRECTION('ref_axis',(1.,0.,0.));
#11442=DIRECTION('',(-0.0868265938642471,0.0868265938642471,-0.992432509138967));
#11443=DIRECTION('center_axis',(-0.0868265938642471,0.0868265938642471,
-0.992432509138967));
#11444=DIRECTION('ref_axis',(0.996194698091746,-5.403663627668E-16,-0.0871557427476577));
#11445=DIRECTION('center_axis',(0.0868265938642471,0.0868265938642471,0.992432509138967));
#11446=DIRECTION('ref_axis',(-0.996194698091746,-5.403663627668E-16,0.0871557427476577));
#11447=DIRECTION('',(0.0868265938642471,0.0868265938642471,0.992432509138967));
#11448=DIRECTION('center_axis',(0.,-0.996194698091745,0.087155742747664));
#11449=DIRECTION('ref_axis',(-1.,0.,0.));
#11450=DIRECTION('',(-0.0868265938642471,-0.0868265938642471,-0.992432509138967));
#11451=DIRECTION('center_axis',(-0.0868265938642471,-0.0868265938642471,
-0.992432509138967));
#11452=DIRECTION('ref_axis',(5.403663627668E-16,0.996194698091746,-0.0871557427476577));
#11453=DIRECTION('',(-0.0868265938642471,-0.0868265938642471,-0.992432509138967));
#11454=DIRECTION('center_axis',(-0.996194698091745,0.,0.087155742747664));
#11455=DIRECTION('ref_axis',(0.,1.,0.));
#11456=DIRECTION('',(0.0868265938642471,0.0868265938642471,0.992432509138967));
#11457=DIRECTION('center_axis',(0.0868265938642471,0.0868265938642471,0.992432509138967));
#11458=DIRECTION('ref_axis',(-0.996194698091746,-5.403663627668E-16,0.0871557427476577));
#11459=DIRECTION('',(0.0868265938642372,0.0868265938642472,0.992432509138968));
#11460=DIRECTION('center_axis',(0.,-0.996194698091745,0.087155742747664));
#11461=DIRECTION('ref_axis',(-1.,0.,0.));
#11462=DIRECTION('',(-0.0868265938642471,0.0868265938642471,0.992432509138967));
#11463=DIRECTION('center_axis',(-0.0868265938642471,0.0868265938642471,
0.992432509138967));
#11464=DIRECTION('ref_axis',(5.403663627668E-16,-0.996194698091746,0.0871557427476577));
#11465=DIRECTION('',(-0.0868265938642471,0.0868265938642471,0.992432509138967));
#11466=DIRECTION('center_axis',(0.996194698091745,0.,0.087155742747664));
#11467=DIRECTION('ref_axis',(0.,-1.,0.));
#11468=DIRECTION('',(0.0868265938642471,-0.0868265938642471,-0.992432509138967));
#11469=DIRECTION('center_axis',(0.0868265938642471,-0.0868265938642471,
-0.992432509138967));
#11470=DIRECTION('ref_axis',(-0.996194698091746,5.403663627668E-16,-0.0871557427476577));
#11471=DIRECTION('',(0.0868265938642471,-0.0868265938642471,-0.992432509138967));
#11472=DIRECTION('center_axis',(0.,-0.996194698091745,0.087155742747664));
#11473=DIRECTION('ref_axis',(-1.,0.,0.));
#11474=DIRECTION('center_axis',(0.0868265938642471,0.0868265938642471,-0.992432509138967));
#11475=DIRECTION('ref_axis',(-5.403663627668E-16,-0.996194698091746,-0.0871557427476577));
#11476=DIRECTION('',(0.0868265938642471,0.0868265938642471,-0.992432509138967));
#11477=DIRECTION('center_axis',(0.,0.996194698091745,0.087155742747664));
#11478=DIRECTION('ref_axis',(1.,0.,0.));
#11479=DIRECTION('',(-0.0868265938642471,-0.0868265938642471,0.992432509138967));
#11480=DIRECTION('center_axis',(-0.0868265938642471,-0.0868265938642471,
0.992432509138967));
#11481=DIRECTION('ref_axis',(0.996194698091746,5.403663627668E-16,0.0871557427476577));
#11482=DIRECTION('axis',(0.,0.,1.));
#11483=DIRECTION('refdir',(1.,0.,0.));
#11484=DIRECTION('center_axis',(-0.866025403784429,0.,0.500000000000017));
#11485=DIRECTION('ref_axis',(0.500000000000017,0.,0.866025403784429));
#11486=DIRECTION('',(3.731805933989E-9,-1.,-1.76837731384E-9));
#11487=DIRECTION('',(4.187512236206E-13,-1.,7.252305024337E-13));
#11488=DIRECTION('',(-1.797493038896E-8,-1.,1.001821272828E-8));
#11489=DIRECTION('center_axis',(-0.866025403784529,2.50962908580945E-13,
0.499999999999843));
#11490=DIRECTION('ref_axis',(-0.0976799095104206,-0.980731635623266,-0.169186566150357));
#11491=DIRECTION('center_axis',(-0.866025403786267,-1.30314015865624E-12,
0.499999999996833));
#11492=DIRECTION('ref_axis',(0.127371879782138,-0.967008591980107,0.220614567237561));
#11493=DIRECTION('center_axis',(0.,-1.,0.));
#11494=DIRECTION('ref_axis',(-0.866025403784429,0.,0.500000000000017));
#11495=DIRECTION('',(-1.265825400597E-11,-1.,4.163515733621E-12));
#11496=DIRECTION('center_axis',(0.0220021483116849,-0.999116223542966,0.0358144848198564));
#11497=DIRECTION('ref_axis',(-0.999757922609801,-0.0219865712180024,0.000828773196178992));
#11498=DIRECTION('center_axis',(0.,-1.,0.));
#11499=DIRECTION('ref_axis',(-0.866025403784429,0.,0.500000000000017));
#11500=DIRECTION('center_axis',(-1.,0.,0.));
#11501=DIRECTION('ref_axis',(0.,0.,1.));
#11502=DIRECTION('',(1.257132338397E-11,-1.,-1.262436544441E-14));
#11503=DIRECTION('center_axis',(-1.,0.,0.));
#11504=DIRECTION('ref_axis',(0.,0.743887963014959,-0.668304345699963));
#11505=DIRECTION('center_axis',(-1.,0.,0.));
#11506=DIRECTION('ref_axis',(0.,0.998312190093586,-0.0580755637987892));
#11507=DIRECTION('center_axis',(-1.,0.,0.));
#11508=DIRECTION('ref_axis',(0.,0.,1.));
#11509=DIRECTION('',(2.02237243844E-8,-1.,-2.714238573232E-14));
#11510=DIRECTION('center_axis',(-1.,0.,0.));
#11511=DIRECTION('ref_axis',(0.,-0.997449181646666,-0.0713801795486376));
#11512=DIRECTION('center_axis',(-1.,0.,0.));
#11513=DIRECTION('ref_axis',(0.,-0.570342240088595,-0.821407164060993));
#11514=DIRECTION('center_axis',(-1.,0.,0.));
#11515=DIRECTION('ref_axis',(0.,0.,1.));
#11516=DIRECTION('center_axis',(-1.,0.,0.));
#11517=DIRECTION('ref_axis',(0.,-0.743887963015197,0.668304345699697));
#11518=DIRECTION('center_axis',(-1.,0.,0.));
#11519=DIRECTION('ref_axis',(0.,-0.998312190093589,0.0580755637987493));
#11520=DIRECTION('center_axis',(-1.,0.,0.));
#11521=DIRECTION('ref_axis',(0.,0.,1.));
#11522=DIRECTION('',(-2.111258706869E-8,-1.,-6.059695388083E-14));
#11523=DIRECTION('center_axis',(-1.,0.,0.));
#11524=DIRECTION('ref_axis',(0.,0.997449181646666,0.0713801795486376));
#11525=DIRECTION('center_axis',(-1.,0.,0.));
#11526=DIRECTION('ref_axis',(0.,0.57034223781309,0.821407165640985));
#11527=DIRECTION('center_axis',(0.,-1.,0.));
#11528=DIRECTION('ref_axis',(-1.,0.,0.));
#11529=DIRECTION('center_axis',(0.022000557232617,0.999116243244608,-0.035814912623604));
#11530=DIRECTION('ref_axis',(-0.999757957615157,0.0219849728771459,-0.000828946778124254));
#11531=DIRECTION('',(-3.509175205565E-9,-1.,-1.661152348979E-9));
#11532=DIRECTION('center_axis',(9.69425622428E-9,-1.,-1.679094432204E-8));
#11533=DIRECTION('ref_axis',(-1.,-9.69425622428E-9,-2.68179925674151E-24));
#11534=DIRECTION('center_axis',(-0.222676118655611,-0.895355451606744,0.385686351143719));
#11535=DIRECTION('ref_axis',(-0.959639358826226,0.131600370203915,-0.248543041652312));
#11536=DIRECTION('center_axis',(-1.,0.,0.));
#11537=DIRECTION('ref_axis',(0.,0.762967197668601,-0.646437201344201));
#11538=DIRECTION('center_axis',(0.,-0.883720930232564,-0.468014227848781));
#11539=DIRECTION('ref_axis',(0.95964016823036,-0.131620002936973,0.248529520068901));
#11540=DIRECTION('center_axis',(-1.,0.,0.));
#11541=DIRECTION('ref_axis',(0.,0.743887962015906,-0.668304346812006));
#11542=DIRECTION('center_axis',(0.,-0.668304347088608,-0.743887961767409));
#11543=DIRECTION('ref_axis',(1.,-1.2479157085834E-11,1.1211197595737E-11));
#11544=DIRECTION('center_axis',(-0.280818391263604,-0.447274630670207,-0.849168084590413));
#11545=DIRECTION('ref_axis',(0.826864856300596,-0.561948510408893,0.0225473072498959));
#11546=DIRECTION('center_axis',(-1.,0.,0.));
#11547=DIRECTION('ref_axis',(0.,0.751071345860703,0.660221048912402));
#11548=DIRECTION('center_axis',(0.,-0.0713801795485182,-0.997449181646675));
#11549=DIRECTION('ref_axis',(-1.,0.,0.));
#11550=DIRECTION('center_axis',(0.,-0.040042283539229,-0.999197986151375));
#11551=DIRECTION('ref_axis',(-0.826848298356623,0.561973937025615,-0.0225207817068473));
#11552=DIRECTION('center_axis',(-1.,0.,0.));
#11553=DIRECTION('ref_axis',(0.,0.99919819108701,-0.0400371693360804));
#11554=DIRECTION('center_axis',(0.49824937053172,-0.0836077691306534,-0.862993224600135));
#11555=DIRECTION('ref_axis',(-0.866025403784453,-4.30093460845859E-13,-0.499999999999976));
#11556=DIRECTION('center_axis',(0.0439783181580926,0.996474919904308,-0.0714397755713733));
#11557=DIRECTION('ref_axis',(-0.99903248020092,0.043873250862281,-0.00303996091638142));
#11558=DIRECTION('center_axis',(-0.868182440414283,0.000195291349290394,
-0.496245112840005));
#11559=DIRECTION('ref_axis',(0.496237261125393,0.00598072766512104,-0.868166350169922));
#11560=DIRECTION('center_axis',(0.493374800291908,-0.162251348583303,-0.854550060745314));
#11561=DIRECTION('ref_axis',(-0.866025364189605,-1.31083826571125E-8,-0.500000068580258));
#11562=DIRECTION('center_axis',(-0.866025403784429,0.,-0.500000000000017));
#11563=DIRECTION('ref_axis',(-0.500000000000017,0.,0.866025403784429));
#11564=DIRECTION('',(-5.201696206723E-13,-1.,9.013782446814E-13));
#11565=DIRECTION('',(1.873702888582E-8,-1.,1.048002362625E-8));
#11566=DIRECTION('center_axis',(-0.866023526388187,3.03179301675285E-7,
-0.500003251731503));
#11567=DIRECTION('ref_axis',(0.0780807385647998,0.987731781529046,-0.135238034674545));
#11568=DIRECTION('center_axis',(0.866025403784448,1.54730561598205E-14,
0.499999999999983));
#11569=DIRECTION('ref_axis',(0.105564362892848,-0.977458265681004,-0.18284283999903));
#11570=DIRECTION('center_axis',(0.190441801473105,-0.924622993985522,-0.329854876036308));
#11571=DIRECTION('ref_axis',(0.86602540378445,3.8663516832569E-14,0.499999999999981));
#11572=DIRECTION('center_axis',(-1.,0.,0.));
#11573=DIRECTION('ref_axis',(0.,0.,1.));
#11574=DIRECTION('center_axis',(-1.,0.,0.));
#11575=DIRECTION('ref_axis',(0.,-0.743887962015906,-0.668304346812006));
#11576=DIRECTION('center_axis',(-1.,0.,0.));
#11577=DIRECTION('ref_axis',(0.,0.,1.));
#11578=DIRECTION('center_axis',(-1.,0.,0.));
#11579=DIRECTION('ref_axis',(0.,0.743887962015906,0.668304346812006));
#11580=DIRECTION('center_axis',(-1.,0.,0.));
#11581=DIRECTION('ref_axis',(0.,-1.97666424549385E-6,-0.999999999998046));
#11582=DIRECTION('center_axis',(-1.,0.,0.));
#11583=DIRECTION('ref_axis',(0.,0.467970411627219,-0.883744133695636));
#11584=DIRECTION('center_axis',(-1.,0.,0.));
#11585=DIRECTION('ref_axis',(0.,0.,1.));
#11586=DIRECTION('center_axis',(-1.,0.,0.));
#11587=DIRECTION('ref_axis',(0.,-0.467970411624927,0.88374413369685));
#11588=DIRECTION('center_axis',(-1.,0.,0.));
#11589=DIRECTION('ref_axis',(0.,-0.467970411624927,0.88374413369685));
#11590=DIRECTION('center_axis',(0.280781834080107,-0.447280798160512,0.849176924584922));
#11591=DIRECTION('ref_axis',(0.826871614630506,0.561937308806419,0.0225786157622499));
#11592=DIRECTION('center_axis',(0.,-0.040042283539229,0.999197986151375));
#11593=DIRECTION('ref_axis',(-0.826851728368265,-0.561968898410276,-0.0225205797872409));
#11594=DIRECTION('center_axis',(-0.351932310973904,-0.0131675051143801,
0.935932831618611));
#11595=DIRECTION('ref_axis',(6.04805910778599E-8,-0.999901048641168,-0.0140674420663423));
#11596=DIRECTION('center_axis',(0.351932331559598,0.0131675058692799,0.935932823867294));
#11597=DIRECTION('ref_axis',(-5.5740687180029E-6,-0.999901018808378,0.014069561290144));
#11598=DIRECTION('center_axis',(0.,0.040042283539229,0.999197986151375));
#11599=DIRECTION('ref_axis',(-0.826848298356623,-0.561973937025615,0.0225207817068473));
#11600=DIRECTION('center_axis',(-0.280818391263604,0.447274630670207,0.849168084590413));
#11601=DIRECTION('ref_axis',(0.826864856300596,0.561948510408893,-0.0225473072498959));
#11602=DIRECTION('center_axis',(0.,0.668304347090714,0.743887961765516));
#11603=DIRECTION('ref_axis',(1.,1.15056772865253E-11,-1.0336629360903E-11));
#11604=DIRECTION('center_axis',(-1.,0.,0.));
#11605=DIRECTION('ref_axis',(0.,-0.751071345860703,-0.660221048912402));
#11606=DIRECTION('center_axis',(0.,0.0713801795485182,0.997449181646675));
#11607=DIRECTION('ref_axis',(-1.,-2.96023766778491E-14,2.11842668399344E-15));
#11608=DIRECTION('center_axis',(-1.,0.,0.));
#11609=DIRECTION('ref_axis',(0.,-0.99919819108701,0.0400371693360804));
#11610=DIRECTION('center_axis',(0.498249370522803,0.0836077693430705,0.862993224584705));
#11611=DIRECTION('ref_axis',(-0.866025403784456,4.10046996357472E-13,0.49999999999997));
#11612=DIRECTION('center_axis',(0.0439824930033502,-0.99647481566198,0.0714386594263497));
#11613=DIRECTION('ref_axis',(-0.999032296552403,-0.043877321995646,0.00304155547751212));
#11614=DIRECTION('center_axis',(-0.868182440268428,-0.000195293486889366,
0.496245113094338));
#11615=DIRECTION('ref_axis',(0.496235363589393,-0.00662239063405862,0.868162777286375));
#11616=DIRECTION('center_axis',(0.493374794684409,0.162251348872403,0.854550063927915));
#11617=DIRECTION('ref_axis',(-0.866025367369646,1.20499664413301E-8,0.500000063072265));
#11618=DIRECTION('center_axis',(0.999372239295449,0.0354277761876217,0.));
#11619=DIRECTION('ref_axis',(0.,0.,1.));
#11620=DIRECTION('center_axis',(0.,-1.,0.));
#11621=DIRECTION('ref_axis',(0.,0.,1.));
#11622=DIRECTION('',(1.38025161653E-12,-1.,0.));
#11623=DIRECTION('center_axis',(-0.999372239543964,0.0354277691772887,4.01641479363486E-8));
#11624=DIRECTION('ref_axis',(4.01406338457382E-8,-1.37498900862607E-9,0.999999999999999));
#11625=DIRECTION('center_axis',(-0.493374730482818,0.162251352179406,-0.854550100366831));
#11626=DIRECTION('ref_axis',(-0.866025403784436,2.20656826144257E-15,0.500000000000005));
#11627=DIRECTION('center_axis',(-0.498249373922926,0.0836076882921444,-0.862993230473945));
#11628=DIRECTION('ref_axis',(-0.866025403784452,3.85108611666864E-15,0.499999999999977));
#11629=DIRECTION('center_axis',(-0.868182476504346,0.000194770775834953,
0.496245049904909));
#11630=DIRECTION('ref_axis',(0.496242860058454,0.00333736388693019,0.868177335481232));
#11631=DIRECTION('center_axis',(0.,0.0713801892709608,-0.99744918095091));
#11632=DIRECTION('ref_axis',(-1.,1.59057546106842E-14,1.1382592680318E-15));
#11633=DIRECTION('center_axis',(0.0220023491734484,0.9991162207134,0.0358144403589185));
#11634=DIRECTION('ref_axis',(-0.865987807571244,0.00114527309927654,0.500063801416858));
#11635=DIRECTION('center_axis',(0.043979209247116,0.996474897810047,0.0714395351920356));
#11636=DIRECTION('ref_axis',(-0.868223079665157,0.00274755012920933,0.496166438712896));
#11637=DIRECTION('center_axis',(-1.,0.,0.));
#11638=DIRECTION('ref_axis',(0.,0.751071345860703,0.660221048912402));
#11639=DIRECTION('center_axis',(-1.,0.,0.));
#11640=DIRECTION('ref_axis',(0.,0.997449180243098,0.0713801991617598));
#11641=DIRECTION('center_axis',(0.,0.040042283539229,-0.999197986151375));
#11642=DIRECTION('ref_axis',(-0.826851728368265,0.561968898410276,0.0225205797872409));
#11643=DIRECTION('center_axis',(0.280781834080107,0.447280798160512,-0.849176924584922));
#11644=DIRECTION('ref_axis',(0.826871614630508,-0.561937308806416,-0.0225786157622471));
#11645=DIRECTION('center_axis',(7.29309508193181E-7,0.668304022744483,-0.743888253155681));
#11646=DIRECTION('ref_axis',(0.999999999999734,-4.87417910926425E-7,5.42509114576228E-7));
#11647=DIRECTION('center_axis',(-1.,0.,0.));
#11648=DIRECTION('ref_axis',(0.,-0.99999889596136,0.00148595964285994));
#11649=DIRECTION('center_axis',(-1.,0.,0.));
#11650=DIRECTION('ref_axis',(0.,0.468006113503988,0.883725227501678));
#11651=DIRECTION('center_axis',(0.,0.883720930238071,-0.468014227838384));
#11652=DIRECTION('ref_axis',(0.959631287113083,-0.131634185239414,-0.248556299598387));
#11653=DIRECTION('center_axis',(9.559147147985E-9,-1.,1.655692853734E-8));
#11654=DIRECTION('ref_axis',(-0.866025403784429,1.79498192924013E-21,0.500000000000017));
#11655=DIRECTION('center_axis',(-0.222723179217891,-0.895308629331963,-0.385767862428684));
#11656=DIRECTION('ref_axis',(-0.86602540376781,-1.65629454595974E-11,0.500000000028802));
#11657=DIRECTION('center_axis',(-0.190441695445105,0.924622974493123,-0.329854991891108));
#11658=DIRECTION('ref_axis',(0.866025432288796,-1.38474408523102E-7,-0.499999950628983));
#11659=DIRECTION('center_axis',(1.8985766484E-10,1.,3.288431217093E-10));
#11660=DIRECTION('ref_axis',(0.866025403784429,2.57201471715716E-23,-0.500000000000017));
#11661=DIRECTION('center_axis',(0.19044180147329,0.92462299398535,0.329854876036682));
#11662=DIRECTION('ref_axis',(0.866025403784455,-1.38777878078137E-14,-0.499999999999972));
#11663=DIRECTION('center_axis',(0.,0.883720930232564,0.468014227848781));
#11664=DIRECTION('ref_axis',(0.959640168230617,0.131620002936562,-0.248529520068125));
#11665=DIRECTION('center_axis',(0.222676472654806,-0.895355099446026,0.385686964288411));
#11666=DIRECTION('ref_axis',(-0.866025536407818,-1.31934723174299E-7,0.49999977028948));
#11667=DIRECTION('center_axis',(-1.,0.,0.));
#11668=DIRECTION('ref_axis',(0.,-0.762644877891583,0.646817431912385));
#11669=DIRECTION('center_axis',(-1.,0.,0.));
#11670=DIRECTION('ref_axis',(0.,-0.743887962015906,0.668304346812006));
#11671=DIRECTION('center_axis',(-1.,0.,0.));
#11672=DIRECTION('ref_axis',(0.,0.0098807139151359,-0.99995118455479));
#11673=DIRECTION('center_axis',(-1.,0.,0.));
#11674=DIRECTION('ref_axis',(0.,0.,-1.));
#11675=DIRECTION('center_axis',(0.,0.99995118455479,0.00988071391513576));
#11676=DIRECTION('ref_axis',(0.,-0.00988071391513575,0.99995118455479));
#11677=DIRECTION('center_axis',(-1.,0.,0.));
#11678=DIRECTION('ref_axis',(0.,-0.468018161851774,-0.883718846792851));
#11679=DIRECTION('center_axis',(-1.,0.,0.));
#11680=DIRECTION('ref_axis',(0.,0.99999889596136,-0.00148595964285994));
#11681=DIRECTION('center_axis',(7.29307587577525E-7,-0.668304022745323,
0.743888253154926));
#11682=DIRECTION('ref_axis',(0.999999999999734,4.87415776280581E-7,-5.42508450466735E-7));
#11683=DIRECTION('center_axis',(0.,-0.883720930238698,0.468014227837199));
#11684=DIRECTION('ref_axis',(0.959631287109364,0.131634185245019,0.248556299609778));
#11685=DIRECTION('center_axis',(0.222725367331005,-0.895306451997919,-0.385771652351708));
#11686=DIRECTION('ref_axis',(-0.959634003928859,-0.131634145854039,-0.248545831083011));
#11687=DIRECTION('center_axis',(0.,-1.,0.));
#11688=DIRECTION('ref_axis',(-1.,0.,0.));
#11689=DIRECTION('center_axis',(0.,-1.,0.));
#11690=DIRECTION('ref_axis',(-1.,0.,0.));
#11691=DIRECTION('center_axis',(0.0220020309913136,-0.999116224741113,-0.0358145234691645));
#11692=DIRECTION('ref_axis',(-0.865987846623121,-0.00114495897030132,-0.500063734507918));
#11693=DIRECTION('center_axis',(0.,-0.0713801877643918,0.997449181058724));
#11694=DIRECTION('ref_axis',(-1.,-2.91605501258917E-14,-2.08680861423913E-15));
#11695=DIRECTION('center_axis',(-0.498249373968018,-0.083607687218453,0.862993230551932));
#11696=DIRECTION('ref_axis',(-0.866025403784423,9.78384040450952E-16,-0.500000000000027));
#11697=DIRECTION('center_axis',(0.0439792054831152,-0.996474897881974,-0.071439536505943));
#11698=DIRECTION('ref_axis',(-0.868223086749888,-0.00274754739562432,-0.496166426330727));
#11699=DIRECTION('center_axis',(-1.,0.,0.));
#11700=DIRECTION('ref_axis',(0.,-0.751071345860703,-0.660221048912402));
#11701=DIRECTION('center_axis',(-1.,0.,0.));
#11702=DIRECTION('ref_axis',(0.,-0.997449180276294,-0.0713801986978796));
#11703=DIRECTION('center_axis',(-1.,0.,0.));
#11704=DIRECTION('ref_axis',(0.,0.,1.));
#11705=DIRECTION('center_axis',(-0.868182476775313,-0.000194768429474923,
-0.496245049431772));
#11706=DIRECTION('ref_axis',(0.496245087391322,-0.000373257433497943,-0.86818239668797));
#11707=DIRECTION('',(-0.999371785786445,-0.0354405142272462,6.10354031209678E-5));
#11708=DIRECTION('',(0.999371785786445,0.0354405142272462,6.10354031209678E-5));
#11709=DIRECTION('',(0.999372166129595,0.0354298400425457,0.));
#11710=DIRECTION('center_axis',(0.999372092799054,0.0354319084221984,-2.05236350338391E-8));
#11711=DIRECTION('ref_axis',(2.05104383127819E-8,7.35929113883462E-10,1.));
#11712=DIRECTION('center_axis',(0.,0.,1.));
#11713=DIRECTION('ref_axis',(1.,0.,0.));
#11714=DIRECTION('',(-0.999372166129596,0.0354298400425258,0.));
#11715=DIRECTION('',(7.743978635044E-13,-1.,0.));
#11716=DIRECTION('center_axis',(-0.999372092671549,0.0354319120185417,0.));
#11717=DIRECTION('ref_axis',(0.,0.,1.));
#11718=DIRECTION('',(-0.999371785786448,0.0354405142271533,-6.1035403120968E-5));
#11719=DIRECTION('center_axis',(-1.,0.,0.));
#11720=DIRECTION('ref_axis',(0.,0.,1.));
#11721=DIRECTION('',(0.999371785786448,-0.0354405142271533,-6.1035403120968E-5));
#11722=DIRECTION('center_axis',(0.999372239295449,-0.0354277761876217,0.));
#11723=DIRECTION('ref_axis',(0.,0.,-1.));
#11724=DIRECTION('center_axis',(0.,-1.,0.));
#11725=DIRECTION('ref_axis',(-0.866025403784429,0.,-0.500000000000017));
#11726=DIRECTION('',(-1.111343038653E-12,-1.,0.));
#11727=DIRECTION('center_axis',(-0.999372239506482,-0.0354277702346294,
-3.41063282467894E-8));
#11728=DIRECTION('ref_axis',(3.40863636314234E-8,1.16752162350377E-9,-0.999999999999999));
#11729=DIRECTION('center_axis',(-0.493374730482899,-0.1622513521788,0.854550100366899));
#11730=DIRECTION('ref_axis',(-0.866025403784418,3.73312492030221E-15,-0.500000000000036));
#11731=DIRECTION('',(-0.9993721661296,-0.0354298400424142,0.));
#11732=DIRECTION('center_axis',(-0.999372092671548,-0.0354319120185517,
0.));
#11733=DIRECTION('ref_axis',(0.,0.,-1.));
#11734=DIRECTION('center_axis',(0.,0.,-1.));
#11735=DIRECTION('ref_axis',(-1.,0.,0.));
#11736=DIRECTION('',(0.9993721661296,-0.0354298400424206,0.));
#11737=DIRECTION('',(-8.842919962527E-13,-1.,0.));
#11738=DIRECTION('center_axis',(0.999372092820432,-0.0354319078192211,2.39647906652608E-8));
#11739=DIRECTION('ref_axis',(2.39493900704611E-8,-8.59072814438014E-10,
-1.));
#11740=DIRECTION('center_axis',(0.737263762925204,0.0895414080136305,0.669645040397004));
#11741=DIRECTION('ref_axis',(0.672345785926011,2.4021409861242E-12,-0.740237221536133));
#11742=DIRECTION('center_axis',(0.,-1.,0.));
#11743=DIRECTION('ref_axis',(0.,0.,-1.));
#11744=DIRECTION('',(-4.095605011303E-13,-1.,-3.717912330146E-13));
#11745=DIRECTION('center_axis',(-0.737263807819715,0.0895413984213018,-0.669644992251814));
#11746=DIRECTION('ref_axis',(0.672345737398719,5.92140809302375E-9,-0.740237265612704));
#11747=DIRECTION('center_axis',(0.737263762924105,-0.0895414080137006,-0.669645040398205));
#11748=DIRECTION('ref_axis',(0.672345785927211,-2.55426235717958E-12,0.740237221535044));
#11749=DIRECTION('center_axis',(0.,1.,0.));
#11750=DIRECTION('ref_axis',(1.,0.,0.));
#11751=DIRECTION('',(4.642472539228E-13,-1.,-4.217568272926E-13));
#11752=DIRECTION('center_axis',(-1.,0.,0.));
#11753=DIRECTION('ref_axis',(0.,1.,0.));
#11754=DIRECTION('center_axis',(-1.,0.,0.));
#11755=DIRECTION('ref_axis',(0.,1.,0.));
#11756=DIRECTION('center_axis',(-1.,0.,0.));
#11757=DIRECTION('ref_axis',(0.,1.,0.));
#11758=DIRECTION('center_axis',(-1.,0.,0.));
#11759=DIRECTION('ref_axis',(0.,-1.,1.22464679914735E-16));
#11760=DIRECTION('center_axis',(1.,0.,0.));
#11761=DIRECTION('ref_axis',(0.,-0.554308231206715,0.832311471035023));
#11762=DIRECTION('center_axis',(1.,0.,0.));
#11763=DIRECTION('ref_axis',(0.,-1.,0.));
#11764=DIRECTION('center_axis',(-1.,0.,0.));
#11765=DIRECTION('ref_axis',(0.,1.,0.));
#11766=DIRECTION('',(0.707106781186547,0.707106781186547,8.65956056235493E-17));
#11767=DIRECTION('center_axis',(-1.,0.,0.));
#11768=DIRECTION('ref_axis',(0.,1.,0.));
#11769=DIRECTION('center_axis',(-1.,0.,0.));
#11770=DIRECTION('ref_axis',(0.,1.,0.));
#11771=DIRECTION('',(-1.,0.,0.));
#11772=DIRECTION('center_axis',(-1.,0.,0.));
#11773=DIRECTION('ref_axis',(0.,-1.,0.));
#11774=DIRECTION('center_axis',(-1.,0.,0.));
#11775=DIRECTION('ref_axis',(0.,0.,1.));
#11776=DIRECTION('center_axis',(-1.,0.,0.));
#11777=DIRECTION('ref_axis',(0.,0.,1.));
#11778=DIRECTION('center_axis',(-1.,0.,0.));
#11779=DIRECTION('ref_axis',(0.,0.,1.));
#11780=DIRECTION('',(-1.,0.,0.));
#11781=DIRECTION('center_axis',(-1.,0.,0.));
#11782=DIRECTION('ref_axis',(0.,0.,1.));
#11783=DIRECTION('center_axis',(-1.,0.,0.));
#11784=DIRECTION('ref_axis',(0.,0.,1.));
#11785=DIRECTION('center_axis',(-0.737263813887754,-0.0895413971243944,
0.669644985744458));
#11786=DIRECTION('ref_axis',(0.672345730839688,-6.72198713358419E-9,0.740237271570168));
#11787=DIRECTION('center_axis',(0.,-1.,0.));
#11788=DIRECTION('ref_axis',(0.672345785906318,0.,0.74023722155402));
#11789=DIRECTION('center_axis',(-0.351932310972217,0.0131675051143506,-0.935932831619245));
#11790=DIRECTION('ref_axis',(6.04805859916508E-8,0.999901048641168,0.0140674420663031));
#11791=DIRECTION('center_axis',(0.351932331559182,-0.0131675058692493,-0.935932823867451));
#11792=DIRECTION('ref_axis',(-5.57406870898581E-6,0.999901018808379,-0.0140695612901056));
#11793=DIRECTION('center_axis',(-0.190441695445105,-0.924622974493123,0.329854991891108));
#11794=DIRECTION('ref_axis',(0.866025432288782,1.38474419875132E-7,0.499999950629006));
#11795=DIRECTION('center_axis',(1.899754571623E-10,-1.,-3.290471439962E-10));
#11796=DIRECTION('ref_axis',(0.866025403784429,6.82424005356271E-24,0.500000000000017));
#11797=DIRECTION('center_axis',(0.,-1.,0.));
#11798=DIRECTION('ref_axis',(-0.866025403784429,0.,0.500000000000017));
#11799=DIRECTION('axis',(0.,0.,1.));
#11800=DIRECTION('refdir',(1.,0.,0.));
#11801=DIRECTION('center_axis',(0.,0.,-1.));
#11802=DIRECTION('ref_axis',(0.,-1.,0.));
#11803=DIRECTION('center_axis',(0.,0.,-1.));
#11804=DIRECTION('ref_axis',(0.,1.,0.));
#11805=DIRECTION('center_axis',(0.,0.,-1.));
#11806=DIRECTION('ref_axis',(0.707106781186549,0.707106781186546,0.));
#11807=DIRECTION('',(0.,-1.,0.));
#11808=DIRECTION('center_axis',(0.,0.,1.));
#11809=DIRECTION('ref_axis',(-0.707106781186546,-0.707106781186549,0.));
#11810=DIRECTION('',(1.,0.,0.));
#11811=DIRECTION('center_axis',(0.,0.,1.));
#11812=DIRECTION('ref_axis',(0.707106781186549,-0.707106781186546,0.));
#11813=DIRECTION('',(0.,1.,0.));
#11814=DIRECTION('center_axis',(0.,0.,-1.));
#11815=DIRECTION('ref_axis',(-0.707106781186546,0.707106781186549,0.));
#11816=DIRECTION('',(1.,0.,0.));
#11817=DIRECTION('center_axis',(0.,0.,1.));
#11818=DIRECTION('ref_axis',(0.707106781186549,-0.707106781186546,0.));
#11819=DIRECTION('',(0.,1.,0.));
#11820=DIRECTION('center_axis',(0.,0.,1.));
#11821=DIRECTION('ref_axis',(0.707106781186546,0.707106781186549,0.));
#11822=DIRECTION('',(-1.,0.,0.));
#11823=DIRECTION('center_axis',(0.,0.,-1.));
#11824=DIRECTION('ref_axis',(-0.707106781186549,-0.707106781186546,0.));
#11825=DIRECTION('',(0.,1.,0.));
#11826=DIRECTION('center_axis',(0.,0.,1.));
#11827=DIRECTION('ref_axis',(0.707106781186546,0.707106781186549,0.));
#11828=DIRECTION('',(-1.,0.,0.));
#11829=DIRECTION('center_axis',(0.,0.,1.));
#11830=DIRECTION('ref_axis',(-0.707106781186549,0.707106781186546,0.));
#11831=DIRECTION('',(0.,-1.,0.));
#11832=DIRECTION('center_axis',(0.,0.,-1.));
#11833=DIRECTION('ref_axis',(0.707106781186546,-0.707106781186549,0.));
#11834=DIRECTION('',(-1.,0.,0.));
#11835=DIRECTION('center_axis',(0.,0.,1.));
#11836=DIRECTION('ref_axis',(-0.707106781186549,0.707106781186546,0.));
#11837=DIRECTION('',(0.,-1.,0.));
#11838=DIRECTION('center_axis',(0.,0.,1.));
#11839=DIRECTION('ref_axis',(-0.707106781186546,-0.707106781186549,0.));
#11840=DIRECTION('',(1.,0.,0.));
#11841=DIRECTION('center_axis',(0.,0.,-1.));
#11842=DIRECTION('ref_axis',(0.,-1.,0.));
#11843=DIRECTION('',(0.,0.,1.));
#11844=DIRECTION('center_axis',(0.,0.,-1.));
#11845=DIRECTION('ref_axis',(0.,1.,0.));
#11846=DIRECTION('center_axis',(0.,0.,-1.));
#11847=DIRECTION('ref_axis',(0.,-1.,0.));
#11848=DIRECTION('',(-8.65956056235493E-17,-0.707106781186547,0.707106781186547));
#11849=DIRECTION('center_axis',(0.,0.,-1.));
#11850=DIRECTION('ref_axis',(0.,1.,0.));
#11851=DIRECTION('center_axis',(0.,0.,-1.));
#11852=DIRECTION('ref_axis',(0.,-1.,0.));
#11853=DIRECTION('center_axis',(-1.,1.22464679914735E-16,0.));
#11854=DIRECTION('ref_axis',(1.22464679914735E-16,1.,0.));
#11855=DIRECTION('center_axis',(0.,0.,-1.));
#11856=DIRECTION('ref_axis',(0.,1.,0.));
#11857=DIRECTION('center_axis',(0.,0.,-1.));
#11858=DIRECTION('ref_axis',(0.,1.,0.));
#11859=DIRECTION('center_axis',(0.,0.,1.));
#11860=DIRECTION('ref_axis',(0.,1.,0.));
#11861=DIRECTION('center_axis',(0.,0.,-1.));
#11862=DIRECTION('ref_axis',(0.,1.,0.));
#11863=DIRECTION('',(-8.65956056235493E-17,0.707106781186547,-0.707106781186547));
#11864=DIRECTION('center_axis',(0.,0.,-1.));
#11865=DIRECTION('ref_axis',(0.,1.,0.));
#11866=DIRECTION('center_axis',(0.,0.,-1.));
#11867=DIRECTION('ref_axis',(-0.951797481692839,0.306727165153609,0.));
#11868=DIRECTION('',(-2.319132540328E-14,-6.945061809599E-14,-1.));
#11869=DIRECTION('',(-0.749745402825771,0.433453378048483,-0.499999999999981));
#11870=DIRECTION('',(0.749745402825771,-0.433453378048483,-0.499999999999981));
#11871=DIRECTION('',(0.64330979105792,-0.579786609649618,-0.500000000000016));
#11872=DIRECTION('',(-0.64330979105792,0.579786609649618,-0.500000000000016));
#11873=DIRECTION('',(-0.508789886402224,0.700808712484933,-0.500000000000023));
#11874=DIRECTION('',(0.508789886402224,-0.700808712484933,-0.500000000000023));
#11875=DIRECTION('',(0.352058281587984,-0.791236353035765,-0.499999999999978));
#11876=DIRECTION('',(-0.352058281587984,0.791236353035765,-0.499999999999978));
#11877=DIRECTION('',(-0.1799572419677,0.847121827757601,-0.5));
#11878=DIRECTION('',(0.1799572419677,-0.847121827757601,-0.5));
#11879=DIRECTION('center_axis',(0.,0.,-1.));
#11880=DIRECTION('ref_axis',(0.,-1.,0.));
#11881=DIRECTION('',(0.,0.,-1.));
#11882=DIRECTION('',(0.,0.,-1.));
#11883=DIRECTION('',(0.,0.,-1.));
#11884=DIRECTION('',(0.,0.,-1.));
#11885=DIRECTION('',(0.,0.,-1.));
#11886=DIRECTION('center_axis',(-0.309687603986101,-0.950838360573104,0.));
#11887=DIRECTION('ref_axis',(-0.950838360573104,0.309687603986101,0.));
#11888=DIRECTION('center_axis',(0.0868265938642471,0.0868265938642471,0.992432509138967));
#11889=DIRECTION('ref_axis',(0.996194698091746,5.403663627668E-16,-0.0871557427476577));
#11890=DIRECTION('',(0.0868265938642471,0.0868265938642471,0.992432509138967));
#11891=DIRECTION('center_axis',(0.,0.,1.));
#11892=DIRECTION('ref_axis',(0.707106781186549,0.707106781186546,0.));
#11893=DIRECTION('',(0.0868265938642471,0.0868265938642471,0.992432509138967));
#11894=DIRECTION('center_axis',(0.,-0.996194698091745,0.087155742747664));
#11895=DIRECTION('ref_axis',(1.,0.,0.));
#11896=DIRECTION('',(-0.0868265938642471,-0.0868265938642471,-0.992432509138967));
#11897=DIRECTION('',(1.,0.,0.));
#11898=DIRECTION('center_axis',(0.,0.,-1.));
#11899=DIRECTION('ref_axis',(1.,0.,0.));
#11900=DIRECTION('',(0.,-1.,0.));
#11901=DIRECTION('center_axis',(0.,0.,-1.));
#11902=DIRECTION('ref_axis',(0.707106781186549,-0.707106781186546,0.));
#11903=DIRECTION('',(-1.,0.,-1.932295848749E-14));
#11904=DIRECTION('center_axis',(0.,0.,-1.));
#11905=DIRECTION('ref_axis',(-0.707106781186546,-0.707106781186549,0.));
#11906=DIRECTION('',(0.,-1.,0.));
#11907=DIRECTION('center_axis',(0.,0.,-1.));
#11908=DIRECTION('ref_axis',(-0.707106781186546,-0.707106781186549,0.));
#11909=DIRECTION('',(0.,-1.,0.));
#11910=DIRECTION('center_axis',(0.,0.,-1.));
#11911=DIRECTION('ref_axis',(-0.707106781186549,0.707106781186546,0.));
#11912=DIRECTION('',(1.,0.,0.));
#11913=DIRECTION('center_axis',(0.,0.,1.));
#11914=DIRECTION('ref_axis',(0.707106781186546,-0.707106781186549,0.));
#11915=DIRECTION('',(0.,-1.,0.));
#11916=DIRECTION('center_axis',(0.,0.,-1.));
#11917=DIRECTION('ref_axis',(-0.707106781186549,0.707106781186546,0.));
#11918=DIRECTION('',(1.,0.,-1.932295848749E-14));
#11919=DIRECTION('center_axis',(0.,0.,-1.));
#11920=DIRECTION('ref_axis',(0.707106781186546,0.707106781186549,0.));
#11921=DIRECTION('',(0.,-1.,0.));
#11922=DIRECTION('center_axis',(0.,0.,1.));
#11923=DIRECTION('ref_axis',(-0.707106781186549,-0.707106781186546,0.));
#11924=DIRECTION('',(1.,0.,0.));
#11925=DIRECTION('center_axis',(0.,0.,-1.));
#11926=DIRECTION('ref_axis',(0.707106781186546,0.707106781186549,0.));
#11927=DIRECTION('',(0.,1.,1.932295848749E-14));
#11928=DIRECTION('center_axis',(0.,0.,-1.));
#11929=DIRECTION('ref_axis',(0.707106781186549,-0.707106781186546,0.));
#11930=DIRECTION('',(-1.,0.,0.));
#11931=DIRECTION('center_axis',(0.,0.,1.));
#11932=DIRECTION('ref_axis',(-0.707106781186546,0.707106781186549,0.));
#11933=DIRECTION('center_axis',(0.996194698091745,0.,0.087155742747664));
#11934=DIRECTION('ref_axis',(0.,1.,0.));
#11935=DIRECTION('',(-0.0868265938642471,0.0868265938642471,0.992432509138967));
#11936=DIRECTION('',(0.0868265938642471,-0.0868265938642471,-0.992432509138967));
#11937=DIRECTION('center_axis',(-0.0868265938642471,0.0868265938642471,
0.992432509138967));
#11938=DIRECTION('ref_axis',(-5.403663627668E-16,0.996194698091746,-0.0871557427476577));
#11939=DIRECTION('',(-0.0868265938642471,0.0868265938642471,0.992432509138967));
#11940=DIRECTION('center_axis',(0.,-0.996194698091745,0.087155742747664));
#11941=DIRECTION('ref_axis',(1.,0.,0.));
#11942=DIRECTION('',(0.0868265938642471,-0.0868265938642471,-0.992432509138967));
#11943=DIRECTION('center_axis',(0.0868265938642471,-0.0868265938642471,
-0.992432509138967));
#11944=DIRECTION('ref_axis',(0.996194698091746,-5.403663627668E-16,0.0871557427476577));
#11945=DIRECTION('',(0.0868265938642471,-0.0868265938642471,-0.992432509138967));
#11946=DIRECTION('center_axis',(0.996194698091745,0.,0.087155742747664));
#11947=DIRECTION('ref_axis',(0.,1.,0.));
#11948=DIRECTION('',(0.0868265938642471,0.0868265938642471,-0.992432509138967));
#11949=DIRECTION('center_axis',(0.0868265938642471,0.0868265938642471,-0.992432509138967));
#11950=DIRECTION('ref_axis',(5.403663627668E-16,0.996194698091746,0.0871557427476577));
#11951=DIRECTION('',(0.0868265938642471,0.0868265938642471,-0.992432509138967));
#11952=DIRECTION('center_axis',(0.,0.996194698091745,0.087155742747664));
#11953=DIRECTION('ref_axis',(-1.,0.,0.));
#11954=DIRECTION('',(-0.0868265938642471,-0.0868265938642471,0.992432509138967));
#11955=DIRECTION('center_axis',(-0.0868265938642471,-0.0868265938642471,
0.992432509138967));
#11956=DIRECTION('ref_axis',(-0.996194698091746,-5.403663627668E-16,-0.0871557427476577));
#11957=DIRECTION('',(-0.0868265938642471,-0.0868265938642471,0.992432509138967));
#11958=DIRECTION('center_axis',(0.996194698091745,0.,0.087155742747664));
#11959=DIRECTION('ref_axis',(0.,1.,0.));
#11960=DIRECTION('',(0.0868265938642471,0.0868265938642471,-0.992432509138967));
#11961=DIRECTION('center_axis',(0.0868265938642471,0.0868265938642471,-0.992432509138967));
#11962=DIRECTION('ref_axis',(5.403663627668E-16,0.996194698091746,0.0871557427476577));
#11963=DIRECTION('',(0.0868265938642471,0.0868265938642471,-0.992432509138967));
#11964=DIRECTION('center_axis',(0.,0.996194698091745,0.087155742747664));
#11965=DIRECTION('ref_axis',(-1.,0.,0.));
#11966=DIRECTION('',(-0.0868265938642471,0.0868265938642471,-0.992432509138967));
#11967=DIRECTION('center_axis',(-0.0868265938642471,0.0868265938642471,
-0.992432509138967));
#11968=DIRECTION('ref_axis',(-0.996194698091746,5.403663627668E-16,0.0871557427476577));
#11969=DIRECTION('',(-0.0868265938642471,0.0868265938642471,-0.992432509138967));
#11970=DIRECTION('center_axis',(-0.996194698091745,0.,0.087155742747664));
#11971=DIRECTION('ref_axis',(0.,-1.,0.));
#11972=DIRECTION('',(0.0868265938642471,-0.0868265938642471,0.992432509138967));
#11973=DIRECTION('center_axis',(0.0868265938642471,-0.0868265938642471,
0.992432509138967));
#11974=DIRECTION('ref_axis',(5.403663627668E-16,-0.996194698091746,-0.0871557427476577));
#11975=DIRECTION('',(0.0868265938642471,-0.0868265938642471,0.992432509138967));
#11976=DIRECTION('center_axis',(0.,0.996194698091745,0.087155742747664));
#11977=DIRECTION('ref_axis',(-1.,0.,0.));
#11978=DIRECTION('',(-0.0868265938642471,0.0868265938642471,-0.992432509138967));
#11979=DIRECTION('center_axis',(-0.0868265938642471,0.0868265938642471,
-0.992432509138967));
#11980=DIRECTION('ref_axis',(-0.996194698091746,5.403663627668E-16,0.0871557427476577));
#11981=DIRECTION('',(-0.0868265938642471,0.0868265938642471,-0.992432509138967));
#11982=DIRECTION('center_axis',(-0.996194698091745,0.,0.087155742747664));
#11983=DIRECTION('ref_axis',(0.,-1.,0.));
#11984=DIRECTION('',(-0.0868265938642471,-0.0868265938642471,-0.992432509138967));
#11985=DIRECTION('center_axis',(-0.0868265938642471,-0.0868265938642471,
-0.992432509138967));
#11986=DIRECTION('ref_axis',(-5.403663627668E-16,-0.996194698091746,0.0871557427476577));
#11987=DIRECTION('center_axis',(0.0868265938642471,-0.0868265938642471,
-0.992432509138967));
#11988=DIRECTION('ref_axis',(0.996194698091746,-5.403663627668E-16,0.0871557427476577));
#11989=DIRECTION('',(0.0868265938642471,-0.0868265938642471,-0.992432509138967));
#11990=DIRECTION('center_axis',(0.,-0.996194698091745,0.087155742747664));
#11991=DIRECTION('ref_axis',(1.,0.,0.));
#11992=DIRECTION('',(-0.0868265938642471,-0.0868265938642471,-0.992432509138967));
#11993=DIRECTION('center_axis',(-0.0868265938642471,-0.0868265938642471,
-0.992432509138967));
#11994=DIRECTION('ref_axis',(-5.403663627668E-16,-0.996194698091746,0.0871557427476577));
#11995=DIRECTION('',(-0.0868265938642471,-0.0868265938642471,-0.992432509138967));
#11996=DIRECTION('center_axis',(-0.996194698091745,0.,0.087155742747664));
#11997=DIRECTION('ref_axis',(0.,-1.,0.));
#11998=DIRECTION('axis',(0.,0.,1.));
#11999=DIRECTION('refdir',(1.,0.,0.));
#12000=DIRECTION('center_axis',(1.,0.,0.));
#12001=DIRECTION('ref_axis',(0.,0.,1.));
#12002=DIRECTION('',(0.,-1.,0.));
#12003=DIRECTION('',(-1.134075269297E-9,-1.795971255033E-10,-1.));
#12004=DIRECTION('',(-4.42567343416081E-9,0.999999999992356,3.90988426483683E-6));
#12005=DIRECTION('',(-2.32692945446299E-8,0.999999999999997,-6.98070862355898E-8));
#12006=DIRECTION('center_axis',(1.,0.,0.));
#12007=DIRECTION('ref_axis',(0.,0.,1.));
#12008=DIRECTION('center_axis',(-1.,0.,0.));
#12009=DIRECTION('ref_axis',(0.,-1.,0.));
#12010=DIRECTION('center_axis',(-1.,0.,0.));
#12011=DIRECTION('ref_axis',(0.,-0.999934254603685,-0.0114667549975298));
#12012=DIRECTION('center_axis',(-1.,0.,0.));
#12013=DIRECTION('ref_axis',(0.,-1.,0.));
#12014=DIRECTION('center_axis',(-1.,0.,0.));
#12015=DIRECTION('ref_axis',(0.,-1.,0.));
#12016=DIRECTION('center_axis',(0.,-0.0114667549975297,0.999934254603685));
#12017=DIRECTION('ref_axis',(0.,0.999934254603685,0.0114667549975297));
#12018=DIRECTION('center_axis',(-1.,0.,0.));
#12019=DIRECTION('ref_axis',(0.,1.,0.));
#12020=DIRECTION('center_axis',(-1.,0.,0.));
#12021=DIRECTION('ref_axis',(0.,1.,0.));
#12022=DIRECTION('',(1.,0.,0.));
#12023=DIRECTION('center_axis',(-1.,0.,0.));
#12024=DIRECTION('ref_axis',(0.,1.,0.));
#12025=DIRECTION('center_axis',(1.,0.,0.));
#12026=DIRECTION('ref_axis',(0.,-1.,0.));
#12027=DIRECTION('center_axis',(-1.,0.,0.));
#12028=DIRECTION('ref_axis',(0.,0.,-1.));
#12029=DIRECTION('center_axis',(-1.,0.,0.));
#12030=DIRECTION('ref_axis',(0.,-0.866025403784429,0.500000000000017));
#12031=DIRECTION('center_axis',(-1.,0.,0.));
#12032=DIRECTION('ref_axis',(0.,-0.866025403784429,0.500000000000017));
#12033=DIRECTION('',(-1.,0.,0.));
#12034=DIRECTION('center_axis',(-1.,0.,0.));
#12035=DIRECTION('ref_axis',(0.,0.,-1.));
#12036=DIRECTION('center_axis',(-1.,0.,0.));
#12037=DIRECTION('ref_axis',(0.,-1.,0.));
#12038=DIRECTION('',(-1.,0.,0.));
#12039=DIRECTION('',(-1.,0.,0.));
#12040=DIRECTION('center_axis',(-1.,0.,0.));
#12041=DIRECTION('ref_axis',(0.,0.,-1.));
#12042=DIRECTION('',(0.500000000000004,-0.750000000000006,-0.433012701892204));
#12043=DIRECTION('',(0.500000000000004,0.750000000000006,0.433012701892204));
#12044=DIRECTION('',(1.,0.,0.));
#12045=DIRECTION('',(1.,0.,0.));
#12046=DIRECTION('',(0.500000000000004,0.750000000000006,-0.433012701892204));
#12047=DIRECTION('',(0.500000000000004,-0.750000000000006,0.433012701892204));
#12048=DIRECTION('',(0.500000000000017,0.,-0.866025403784429));
#12049=DIRECTION('',(0.500000000000017,1.24992574614904E-14,0.866025403784429));
#12050=DIRECTION('',(1.,0.,0.));
#12051=DIRECTION('center_axis',(0.,-0.500000000000017,0.866025403784429));
#12052=DIRECTION('ref_axis',(0.,-0.866025403784429,-0.500000000000017));
#12053=DIRECTION('center_axis',(1.,0.,0.));
#12054=DIRECTION('ref_axis',(0.,0.,1.));
#12055=DIRECTION('center_axis',(1.,0.,0.));
#12056=DIRECTION('ref_axis',(0.,0.,1.));
#12057=DIRECTION('center_axis',(1.,0.,0.));
#12058=DIRECTION('ref_axis',(0.,0.,1.));
#12059=DIRECTION('',(1.,0.,0.));
#12060=DIRECTION('center_axis',(1.,0.,0.));
#12061=DIRECTION('ref_axis',(0.,0.,1.));
#12062=DIRECTION('center_axis',(1.,0.,0.));
#12063=DIRECTION('ref_axis',(0.,0.,1.));
#12064=DIRECTION('center_axis',(1.,0.,0.));
#12065=DIRECTION('ref_axis',(0.,0.,1.));
#12066=DIRECTION('center_axis',(1.,0.,0.));
#12067=DIRECTION('ref_axis',(0.,0.,1.));
#12068=DIRECTION('',(1.,0.,0.));
#12069=DIRECTION('center_axis',(1.,0.,0.));
#12070=DIRECTION('ref_axis',(0.,0.,1.));
#12071=DIRECTION('center_axis',(1.,0.,0.));
#12072=DIRECTION('ref_axis',(0.,0.,1.));
#12073=DIRECTION('',(-1.419652628015E-8,-1.,0.));
#12074=DIRECTION('',(0.,-3.273726813475E-12,-1.));
#12075=DIRECTION('',(0.,1.,0.));
#12076=DIRECTION('center_axis',(-1.,0.,0.));
#12077=DIRECTION('ref_axis',(0.,-0.181670789891997,0.983359407388783));
#12078=DIRECTION('center_axis',(1.,0.,0.));
#12079=DIRECTION('ref_axis',(0.,-0.500000000000017,-0.866025403784429));
#12080=DIRECTION('',(0.,0.866025403790389,-0.499999999989694));
#12081=DIRECTION('center_axis',(-1.,0.,0.));
#12082=DIRECTION('ref_axis',(0.,-0.866025403784429,-0.500000000000017));
#12083=DIRECTION('',(0.,-0.499999999989307,0.866025403790612));
#12084=DIRECTION('center_axis',(1.,0.,0.));
#12085=DIRECTION('ref_axis',(0.,0.983359407388783,-0.181670789891997));
#12086=DIRECTION('center_axis',(-1.,0.,0.));
#12087=DIRECTION('ref_axis',(0.,0.,-1.));
#12088=DIRECTION('',(-2.63758496709599E-8,-0.999999999999996,7.91298651712797E-8));
#12089=DIRECTION('center_axis',(-1.,0.,0.));
#12090=DIRECTION('ref_axis',(0.,0.,-1.));
#12091=DIRECTION('center_axis',(1.,0.,0.));
#12092=DIRECTION('ref_axis',(0.,0.,-1.));
#12093=DIRECTION('center_axis',(-1.,0.,0.));
#12094=DIRECTION('ref_axis',(0.,0.,-1.));
#12095=DIRECTION('',(1.,0.,0.));
#12096=DIRECTION('center_axis',(1.,0.,0.));
#12097=DIRECTION('ref_axis',(0.,0.,-1.));
#12098=DIRECTION('',(5.13413878158674E-11,0.866025574454957,-0.499999704389875));
#12099=DIRECTION('center_axis',(1.,0.,0.));
#12100=DIRECTION('ref_axis',(0.,-0.399559341953183,0.91670733184476));
#12101=DIRECTION('',(6.42234657013179E-12,-0.499999694960384,0.866025579899072));
#12102=DIRECTION('center_axis',(-1.,0.,0.));
#12103=DIRECTION('ref_axis',(0.,-0.866025403784429,-0.500000000000017));
#12104=DIRECTION('center_axis',(0.,0.866025403784429,-0.500000000000017));
#12105=DIRECTION('ref_axis',(-1.,0.,0.));
#12106=DIRECTION('center_axis',(0.,0.866025403784429,-0.500000000000017));
#12107=DIRECTION('ref_axis',(-1.,0.,0.));
#12108=DIRECTION('',(0.,-0.866025403784429,0.500000000000017));
#12109=DIRECTION('center_axis',(0.,0.916707576755026,0.399558780056111));
#12110=DIRECTION('ref_axis',(1.,6.74402148298192E-13,-1.54728062548894E-12));
#12111=DIRECTION('center_axis',(1.,0.,0.));
#12112=DIRECTION('ref_axis',(0.,-0.500000000000017,-0.866025403784429));
#12113=DIRECTION('center_axis',(1.,0.,0.));
#12114=DIRECTION('ref_axis',(0.,0.999999564444476,0.000933333197827078));
#12115=DIRECTION('center_axis',(0.,0.399559341952196,0.91670733184519));
#12116=DIRECTION('ref_axis',(1.,0.,0.));
#12117=DIRECTION('center_axis',(1.,0.,0.));
#12118=DIRECTION('ref_axis',(0.,-0.399559341953183,0.91670733184476));
#12119=DIRECTION('center_axis',(-1.,0.,0.));
#12120=DIRECTION('ref_axis',(0.,0.866025403784429,0.500000000000017));
#12121=DIRECTION('center_axis',(1.,0.,0.));
#12122=DIRECTION('ref_axis',(0.,0.983359407388783,-0.181670789891997));
#12123=DIRECTION('center_axis',(1.,0.,0.));
#12124=DIRECTION('ref_axis',(0.,0.983359407388783,-0.181670789891997));
#12125=DIRECTION('',(-1.,9.103769590032E-11,-1.576833478604E-10));
#12126=DIRECTION('',(1.,-3.095953123496E-11,-1.675853530022E-10));
#12127=DIRECTION('center_axis',(1.,0.,0.));
#12128=DIRECTION('ref_axis',(0.,0.969024744073282,-0.246963651928195));
#12129=DIRECTION('center_axis',(0.,0.181670789891997,0.983359407388783));
#12130=DIRECTION('ref_axis',(0.,-0.983359407388783,0.181670789891997));
#12131=DIRECTION('center_axis',(0.,-0.500000000000017,0.866025403784429));
#12132=DIRECTION('ref_axis',(0.,-0.866025403784429,-0.500000000000017));
#12133=DIRECTION('center_axis',(0.,-0.500000000000017,0.866025403784429));
#12134=DIRECTION('ref_axis',(0.,-0.866025403784429,-0.500000000000017));
#12135=DIRECTION('',(0.,-0.500000000000017,0.866025403784429));
#12136=DIRECTION('center_axis',(0.,-0.500000000000017,0.866025403784429));
#12137=DIRECTION('ref_axis',(0.,-0.866025403784429,-0.500000000000017));
#12138=DIRECTION('center_axis',(0.,-0.866025403784429,-0.500000000000017));
#12139=DIRECTION('ref_axis',(0.,0.500000000000017,-0.866025403784429));
#12140=DIRECTION('',(-1.,2.030967986381E-12,-3.514818066227E-12));
#12141=DIRECTION('',(0.,0.500000000000017,-0.866025403784429));
#12142=DIRECTION('center_axis',(0.,-0.500000000000017,0.866025403784429));
#12143=DIRECTION('ref_axis',(-1.,0.,0.));
#12144=DIRECTION('center_axis',(0.,-0.500000000000017,0.866025403784429));
#12145=DIRECTION('ref_axis',(-1.,0.,0.));
#12146=DIRECTION('center_axis',(1.,0.,0.));
#12147=DIRECTION('ref_axis',(0.,-0.850531242834003,-0.525924524017702));
#12148=DIRECTION('center_axis',(-1.,0.,0.));
#12149=DIRECTION('ref_axis',(0.,-0.866025403784429,-0.500000000000017));
#12150=DIRECTION('center_axis',(1.,0.,0.));
#12151=DIRECTION('ref_axis',(0.,-0.707106781187104,0.707106781185991));
#12152=DIRECTION('center_axis',(-1.,0.,0.));
#12153=DIRECTION('ref_axis',(0.,-0.866025403784429,-0.500000000000017));
#12154=DIRECTION('',(-1.,-2.646771690706E-13,1.515824502955E-13));
#12155=DIRECTION('center_axis',(1.,0.,0.));
#12156=DIRECTION('ref_axis',(0.,-0.855623464285791,-0.517598770635694));
#12157=DIRECTION('center_axis',(0.,0.866025403784429,-0.500000000000017));
#12158=DIRECTION('ref_axis',(0.,0.500000000000017,0.866025403784429));
#12159=DIRECTION('center_axis',(0.,0.866025403784429,-0.500000000000017));
#12160=DIRECTION('ref_axis',(0.,0.500000000000017,0.866025403784429));
#12161=DIRECTION('',(0.,0.866025403784429,-0.500000000000017));
#12162=DIRECTION('center_axis',(0.,0.866025403784429,-0.500000000000017));
#12163=DIRECTION('ref_axis',(0.,0.500000000000017,0.866025403784429));
#12164=DIRECTION('center_axis',(0.,0.500000000000017,0.866025403784429));
#12165=DIRECTION('ref_axis',(0.,-0.866025403784429,0.500000000000017));
#12166=DIRECTION('',(1.,-1.516879954977E-10,8.757853701506E-11));
#12167=DIRECTION('center_axis',(-1.,0.,0.));
#12168=DIRECTION('ref_axis',(0.,0.181670789891997,-0.983359407388783));
#12169=DIRECTION('center_axis',(1.,0.,0.));
#12170=DIRECTION('ref_axis',(0.,-0.500000000000017,-0.866025403784429));
#12171=DIRECTION('',(-1.,-1.747034739097E-10,-3.227581165296E-11));
#12172=DIRECTION('center_axis',(-1.,0.,0.));
#12173=DIRECTION('ref_axis',(0.,-0.552140107391307,-0.833751342913411));
#12174=DIRECTION('center_axis',(0.,0.983359407388783,0.181670789891997));
#12175=DIRECTION('ref_axis',(0.,-0.181670789891997,0.983359407388783));
#12176=DIRECTION('center_axis',(1.,0.,0.));
#12177=DIRECTION('ref_axis',(0.,-0.0912156582260493,0.995831162243073));
#12178=DIRECTION('center_axis',(-1.,0.,0.));
#12179=DIRECTION('ref_axis',(0.,-0.181670789891997,0.983359407388783));
#12180=DIRECTION('center_axis',(0.,1.,0.));
#12181=DIRECTION('ref_axis',(0.,0.,1.));
#12182=DIRECTION('center_axis',(1.,0.,0.));
#12183=DIRECTION('ref_axis',(0.,0.,1.));
#12184=DIRECTION('center_axis',(-1.,0.,0.));
#12185=DIRECTION('ref_axis',(0.,0.,-1.));
#12186=DIRECTION('',(1.,0.,0.));
#12187=DIRECTION('center_axis',(1.,0.,0.));
#12188=DIRECTION('ref_axis',(0.,0.,1.));
#12189=DIRECTION('',(1.,0.,0.));
#12190=DIRECTION('center_axis',(1.,0.,0.));
#12191=DIRECTION('ref_axis',(0.,0.0076661909649299,-0.999970614326286));
#12192=DIRECTION('center_axis',(0.,-1.,0.));
#12193=DIRECTION('ref_axis',(0.,0.,-1.));
#12194=DIRECTION('center_axis',(0.,-1.,0.));
#12195=DIRECTION('ref_axis',(0.,0.,-1.));
#12196=DIRECTION('',(-8.96449889951894E-8,-0.999999999999993,7.91296186399094E-8));
#12197=DIRECTION('center_axis',(0.,-1.,0.));
#12198=DIRECTION('ref_axis',(2.7385805267949E-7,0.,-0.999999999999963));
#12199=DIRECTION('center_axis',(0.,0.,-1.));
#12200=DIRECTION('ref_axis',(0.,1.,0.));
#12201=DIRECTION('',(3.87257253216599E-8,0.999999999999997,-6.98071249166998E-8));
#12202=DIRECTION('',(1.,0.,0.));
#12203=DIRECTION('center_axis',(1.,1.57229173603E-10,0.));
#12204=DIRECTION('ref_axis',(-1.55747353131272E-10,0.990575410162307,0.136968451775501));
#12205=DIRECTION('center_axis',(-0.0400339593305145,0.0439586138816482,
0.998230896319046));
#12206=DIRECTION('ref_axis',(0.672168878015028,-0.73800672205553,0.0594565188088726));
#12207=DIRECTION('center_axis',(-0.00691483422088646,-0.977373823122084,
-0.211406232035434));
#12208=DIRECTION('ref_axis',(0.995574959726093,0.0130842956657209,-0.0930553640222855));
#12209=DIRECTION('center_axis',(0.,-1.,0.));
#12210=DIRECTION('ref_axis',(0.992164397268247,0.,-0.124939220396706));
#12211=DIRECTION('',(5.416713864812E-14,1.,4.290037380931E-13));
#12212=DIRECTION('center_axis',(0.,-1.,0.));
#12213=DIRECTION('ref_axis',(0.992164397268247,0.,-0.124939220396706));
#12214=DIRECTION('center_axis',(0.,-0.993031974610984,-0.117845226463398));
#12215=DIRECTION('ref_axis',(0.991993011196462,0.0148830010065676,-0.125412766568694));
#12216=DIRECTION('center_axis',(-0.124870949205596,-0.0330540747897288,
-0.991622243691764));
#12217=DIRECTION('ref_axis',(-4.15466272496426E-16,0.999444906979154,-0.0333148302326418));
#12218=DIRECTION('',(-0.124870949205706,-0.0330540747749215,-0.991622243692244));
#12219=DIRECTION('center_axis',(0.,0.,-1.));
#12220=DIRECTION('ref_axis',(0.96670522786149,0.255892560316366,0.));
#12221=DIRECTION('',(-0.124870949205497,-0.0330540747897292,-0.991622243691777));
#12222=DIRECTION('center_axis',(-0.519150775460989,0.833954178873382,-0.187090619427796));
#12223=DIRECTION('ref_axis',(-0.854630432587176,-0.504108685418202,0.1244236994378));
#12224=DIRECTION('center_axis',(0.,-0.979738498904873,-0.200280987024795));
#12225=DIRECTION('ref_axis',(0.559356823890107,0.166018314377717,-0.812131678275607));
#12226=DIRECTION('center_axis',(0.,-0.964005425963159,-0.265882565644289));
#12227=DIRECTION('ref_axis',(0.391203692848694,0.244692820224845,-0.887178163861102));
#12228=DIRECTION('center_axis',(-0.821166253638671,0.530754423774481,0.209727741438393));
#12229=DIRECTION('ref_axis',(-0.523347833413461,-0.846903765812651,0.0941331860386426));
#12230=DIRECTION('center_axis',(0.959966443903985,-7.32732351878489E-7,
0.280115023834496));
#12231=DIRECTION('ref_axis',(0.257680928625254,0.392129214826704,-0.883082792212723));
#12232=DIRECTION('center_axis',(0.,0.,1.));
#12233=DIRECTION('ref_axis',(0.707106785728413,0.707106776644682,0.));
#12234=DIRECTION('center_axis',(0.,0.,1.));
#12235=DIRECTION('ref_axis',(1.,0.,0.));
#12236=DIRECTION('',(-8.269906478952E-12,0.,-1.));
#12237=DIRECTION('center_axis',(0.,0.,1.));
#12238=DIRECTION('ref_axis',(1.,0.,0.));
#12239=DIRECTION('center_axis',(0.,1.,0.));
#12240=DIRECTION('ref_axis',(0.,0.,1.));
#12241=DIRECTION('center_axis',(-1.,0.,0.));
#12242=DIRECTION('ref_axis',(0.,0.,1.));
#12243=DIRECTION('center_axis',(0.,0.,1.));
#12244=DIRECTION('ref_axis',(0.,-1.,0.));
#12245=DIRECTION('',(0.,1.,0.));
#12246=DIRECTION('',(-1.,0.,0.));
#12247=DIRECTION('center_axis',(0.,0.,1.));
#12248=DIRECTION('ref_axis',(0.,1.,0.));
#12249=DIRECTION('',(0.,-1.,0.));
#12250=DIRECTION('center_axis',(0.,0.,1.));
#12251=DIRECTION('ref_axis',(0.,-1.,0.));
#12252=DIRECTION('center_axis',(0.,0.,1.));
#12253=DIRECTION('ref_axis',(0.,-1.,0.));
#12254=DIRECTION('center_axis',(0.,0.,1.));
#12255=DIRECTION('ref_axis',(0.,-1.,0.));
#12256=DIRECTION('',(0.,0.,1.));
#12257=DIRECTION('center_axis',(0.,0.,1.));
#12258=DIRECTION('ref_axis',(0.,-1.,0.));
#12259=DIRECTION('center_axis',(0.,0.,1.));
#12260=DIRECTION('ref_axis',(0.,1.,0.));
#12261=DIRECTION('center_axis',(0.,0.,1.));
#12262=DIRECTION('ref_axis',(0.,1.,0.));
#12263=DIRECTION('center_axis',(0.,0.,1.));
#12264=DIRECTION('ref_axis',(0.,-1.,0.));
#12265=DIRECTION('',(0.,0.,1.));
#12266=DIRECTION('',(0.,0.,1.));
#12267=DIRECTION('center_axis',(0.,0.,-1.));
#12268=DIRECTION('ref_axis',(0.,-1.,0.));
#12269=DIRECTION('center_axis',(0.,0.,1.));
#12270=DIRECTION('ref_axis',(0.673329668846713,-0.739342381478822,0.));
#12271=DIRECTION('',(-1.,0.,0.));
#12272=DIRECTION('center_axis',(0.,0.,-1.));
#12273=DIRECTION('ref_axis',(-0.313683251850025,-0.949527681275693,0.));
#12274=DIRECTION('',(0.,-1.,0.));
#12275=DIRECTION('center_axis',(0.,0.,1.));
#12276=DIRECTION('ref_axis',(-0.80779094785921,0.589469070059421,0.));
#12277=DIRECTION('',(-1.,0.,0.));
#12278=DIRECTION('',(0.,-1.,0.));
#12279=DIRECTION('center_axis',(0.123779845007298,-0.135915123929598,0.982957592705388));
#12280=DIRECTION('ref_axis',(9.61036805691157E-16,-0.990575410162308,-0.136968451775493));
#12281=DIRECTION('',(0.123779845007102,-0.135915123929602,0.982957592705412));
#12282=DIRECTION('',(0.123779534119897,-0.135915212762297,0.982957619571078));
#12283=DIRECTION('center_axis',(-0.992164397268247,0.,0.124939220396706));
#12284=DIRECTION('ref_axis',(0.124939220396706,0.,0.992164397268247));
#12285=DIRECTION('center_axis',(0.,0.990575410162307,0.136968451775501));
#12286=DIRECTION('ref_axis',(0.,0.136968451775501,-0.990575410162307));
#12287=DIRECTION('',(1.,0.,0.));
#12288=DIRECTION('',(0.0452022558840394,0.136828450245298,-0.989562899095587));
#12289=DIRECTION('center_axis',(1.,0.,0.));
#12290=DIRECTION('ref_axis',(0.,0.990575410162307,0.136968451775501));
#12291=DIRECTION('center_axis',(1.,0.,0.));
#12292=DIRECTION('ref_axis',(0.,0.990575410162307,0.136968451775501));
#12293=DIRECTION('center_axis',(0.0147910789458937,0.0447731623135355,0.998887675326942));
#12294=DIRECTION('ref_axis',(-0.313280857521534,-0.948489162952014,0.0471530706652296));
#12295=DIRECTION('center_axis',(0.,0.999999999999929,-3.77402948630611E-7));
#12296=DIRECTION('ref_axis',(1.16229440341503E-7,-3.77402948630608E-7,-0.999999999999922));
#12297=DIRECTION('center_axis',(0.0209905750013486,0.971496035276488,-0.236124647597782));
#12298=DIRECTION('ref_axis',(-0.0900783656611823,0.237053837004821,0.967311411284444));
#12299=DIRECTION('center_axis',(0.998958343750615,0.,0.0456314305170007));
#12300=DIRECTION('ref_axis',(0.0456314305170007,0.,-0.998958343750615));
#12301=DIRECTION('',(1.30063660726595E-7,0.999999999996163,-2.7670341656329E-6));
#12302=DIRECTION('',(-0.0456061512274497,0.0332801611178298,0.998404982883294));
#12303=DIRECTION('',(0.0452020303481621,0.136828427182506,-0.989562912586747));
#12304=DIRECTION('center_axis',(0.0452022558846083,0.136828450245295,-0.989562899095562));
#12305=DIRECTION('ref_axis',(4.63171168085811E-16,-0.990575410162305,-0.136968451775511));
#12306=DIRECTION('center_axis',(-0.045606153526751,0.0332801660870907,0.998404982612622));
#12307=DIRECTION('ref_axis',(1.51788304147964E-16,0.999444906979154,-0.0333148302326418));
#12308=DIRECTION('',(-0.0456061527666419,0.0332801651001014,0.998404982680243));
#12309=DIRECTION('center_axis',(-0.00599371100089924,0.993987697016237,
0.109327643388101));
#12310=DIRECTION('ref_axis',(-0.0158677933944027,-0.109410380526878,0.993870002447884));
#12311=DIRECTION('center_axis',(0.997994746578697,0.000832709485814794,
-0.0632913295502143));
#12312=DIRECTION('ref_axis',(0.059454730773529,-0.355397842285051,0.932822335006928));
#12313=DIRECTION('center_axis',(1.,0.,0.));
#12314=DIRECTION('ref_axis',(0.,0.999444906979154,-0.0333148302326385));
#12315=DIRECTION('',(0.999999999999499,3.543019115023E-8,1.000251741924E-6));
#12316=DIRECTION('',(0.999999999999606,-2.05591310759001E-9,-8.87615856965605E-7));
#12317=DIRECTION('center_axis',(0.999999999998528,0.,-1.71571223939805E-6));
#12318=DIRECTION('ref_axis',(-5.71586619530014E-8,0.999444906979749,-0.0333148302147516));
#12319=DIRECTION('center_axis',(0.,-0.999444906979154,0.0333148302326385));
#12320=DIRECTION('ref_axis',(0.,0.0333148302326385,0.999444906979154));
#12321=DIRECTION('center_axis',(-8.77617113914048E-11,-1.,1.28881744793477E-9));
#12322=DIRECTION('ref_axis',(0.994676936356327,4.5508643513665E-11,0.103042672135346));
#12323=DIRECTION('center_axis',(0.992288436659883,0.,0.123950225780698));
#12324=DIRECTION('ref_axis',(0.00423001996726221,0.999417512380893,-0.03386359221145));
#12325=DIRECTION('center_axis',(0.97803698136698,0.,0.208431434957796));
#12326=DIRECTION('ref_axis',(0.170039536409224,0.578326194595119,-0.797888067778222));
#12327=DIRECTION('center_axis',(0.,1.,0.));
#12328=DIRECTION('ref_axis',(0.,0.,1.));
#12329=DIRECTION('',(-1.,0.,0.));
#12330=DIRECTION('',(3.309808819951E-11,5.093238724031E-10,-1.));
#12331=DIRECTION('center_axis',(-1.,0.,0.));
#12332=DIRECTION('ref_axis',(0.,0.,1.));
#12333=DIRECTION('center_axis',(-1.,0.,0.));
#12334=DIRECTION('ref_axis',(0.,0.,1.));
#12335=DIRECTION('center_axis',(0.,0.,-1.));
#12336=DIRECTION('ref_axis',(0.0301983768555915,0.999543925015448,0.));
#12337=DIRECTION('center_axis',(0.,0.,1.));
#12338=DIRECTION('ref_axis',(0.,1.,0.));
#12339=DIRECTION('center_axis',(0.,-1.,0.));
#12340=DIRECTION('ref_axis',(0.,0.,1.));
#12341=DIRECTION('center_axis',(0.,-1.,0.));
#12342=DIRECTION('ref_axis',(0.,0.,1.));
#12343=DIRECTION('center_axis',(0.,-1.,0.));
#12344=DIRECTION('ref_axis',(0.,0.,1.));
#12345=DIRECTION('center_axis',(1.,0.,0.));
#12346=DIRECTION('ref_axis',(0.,-1.,1.24367530163205E-13));
#12347=DIRECTION('center_axis',(0.,1.,0.));
#12348=DIRECTION('ref_axis',(0.,0.,-1.));
#12349=DIRECTION('center_axis',(0.,1.,0.));
#12350=DIRECTION('ref_axis',(0.,0.,-1.));
#12351=DIRECTION('center_axis',(0.,0.,-1.));
#12352=DIRECTION('ref_axis',(-1.,0.,0.));
#12353=DIRECTION('center_axis',(0.,1.,0.));
#12354=DIRECTION('ref_axis',(-0.998958343750615,0.,-0.0456314305170007));
#12355=DIRECTION('center_axis',(0.,1.,0.));
#12356=DIRECTION('ref_axis',(0.,0.,1.));
#12357=DIRECTION('axis',(0.,0.,1.));
#12358=DIRECTION('refdir',(1.,0.,0.));
#12359=DIRECTION('center_axis',(0.,1.,0.));
#12360=DIRECTION('ref_axis',(1.,0.,0.));
#12361=DIRECTION('center_axis',(0.,-1.,0.));
#12362=DIRECTION('ref_axis',(1.,0.,0.));
#12363=DIRECTION('center_axis',(0.,-1.,0.));
#12364=DIRECTION('ref_axis',(1.,0.,0.));
#12365=DIRECTION('center_axis',(0.,1.,0.));
#12366=DIRECTION('ref_axis',(1.,0.,0.));
#12367=DIRECTION('',(0.,1.,0.));
#12368=DIRECTION('center_axis',(0.,-1.,0.));
#12369=DIRECTION('ref_axis',(1.,0.,0.));
#12370=DIRECTION('center_axis',(0.,1.,0.));
#12371=DIRECTION('ref_axis',(1.,0.,0.));
#12372=DIRECTION('center_axis',(0.,1.,0.));
#12373=DIRECTION('ref_axis',(-1.,0.,0.));
#12374=DIRECTION('center_axis',(0.,1.,0.));
#12375=DIRECTION('ref_axis',(-0.999990481172045,0.,-0.0043632058514502));
#12376=DIRECTION('center_axis',(0.00436320585145007,0.,-0.999990481172045));
#12377=DIRECTION('ref_axis',(0.999990481172045,0.,0.00436320585145007));
#12378=DIRECTION('axis',(0.,0.,1.));
#12379=DIRECTION('refdir',(1.,0.,0.));
#12380=DIRECTION('center_axis',(0.,0.,-1.));
#12381=DIRECTION('ref_axis',(0.,-1.,0.));
#12382=DIRECTION('center_axis',(0.,0.,1.));
#12383=DIRECTION('ref_axis',(0.,-1.,0.));
#12384=DIRECTION('center_axis',(0.,0.,1.));
#12385=DIRECTION('ref_axis',(0.,-1.,0.));
#12386=DIRECTION('center_axis',(0.,0.,1.));
#12387=DIRECTION('ref_axis',(0.,-1.,0.));
#12388=DIRECTION('',(0.,0.,1.));
#12389=DIRECTION('center_axis',(0.,0.,-1.));
#12390=DIRECTION('ref_axis',(0.,-1.,0.));
#12391=DIRECTION('center_axis',(0.,0.,-1.));
#12392=DIRECTION('ref_axis',(0.,1.,0.));
#12393=DIRECTION('center_axis',(0.,0.,1.));
#12394=DIRECTION('ref_axis',(0.500000000000017,0.866025403784429,0.));
#12395=DIRECTION('center_axis',(0.,0.,1.));
#12396=DIRECTION('ref_axis',(0.500000000000017,0.866025403784429,0.));
#12397=DIRECTION('',(0.,0.,1.));
#12398=DIRECTION('',(0.,0.,1.));
#12399=DIRECTION('center_axis',(0.,0.,-1.));
#12400=DIRECTION('ref_axis',(0.,-1.,0.));
#12401=DIRECTION('',(0.866025403784429,0.500000000000017,0.));
#12402=DIRECTION('center_axis',(0.,0.,1.));
#12403=DIRECTION('ref_axis',(-0.500000000000017,0.866025403784429,0.));
#12404=DIRECTION('',(0.,1.,0.));
#12405=DIRECTION('center_axis',(0.,0.,1.));
#12406=DIRECTION('ref_axis',(-1.,0.,0.));
#12407=DIRECTION('',(-0.866025403784429,0.500000000000017,0.));
#12408=DIRECTION('center_axis',(0.,0.,1.));
#12409=DIRECTION('ref_axis',(-0.500000000000017,-0.866025403784429,0.));
#12410=DIRECTION('',(-0.866025403784429,-0.500000000000017,0.));
#12411=DIRECTION('center_axis',(0.,0.,1.));
#12412=DIRECTION('ref_axis',(0.500000000000017,-0.866025403784429,0.));
#12413=DIRECTION('',(0.,-1.,0.));
#12414=DIRECTION('center_axis',(0.,0.,1.));
#12415=DIRECTION('ref_axis',(1.,0.,0.));
#12416=DIRECTION('',(0.866025403784429,-0.500000000000017,0.));
#12417=DIRECTION('center_axis',(0.,0.,-1.));
#12418=DIRECTION('ref_axis',(0.,-1.,0.));
#12419=DIRECTION('center_axis',(0.,0.,-1.));
#12420=DIRECTION('ref_axis',(0.,-1.,0.));
#12421=DIRECTION('',(0.,0.,1.));
#12422=DIRECTION('',(0.,0.,1.));
#12423=DIRECTION('center_axis',(-0.500000000000017,-0.866025403784429,0.));
#12424=DIRECTION('ref_axis',(-0.866025403784429,0.500000000000017,0.));
#12425=DIRECTION('',(0.296198132725996,0.813797681349388,-0.499999999999993));
#12426=DIRECTION('',(-0.852868531952436,0.150383733180406,-0.500000000000021));
#12427=DIRECTION('',(-0.296198132725996,-0.813797681349388,-0.499999999999993));
#12428=DIRECTION('',(0.852868531952436,-0.150383733180406,-0.500000000000021));
#12429=DIRECTION('',(0.,0.,-1.));
#12430=DIRECTION('',(0.,0.,-1.));
#12431=DIRECTION('center_axis',(0.500000000000017,0.866025403784429,0.));
#12432=DIRECTION('ref_axis',(0.866025403784429,-0.500000000000017,0.));
#12433=DIRECTION('',(0.,0.,1.));
#12434=DIRECTION('center_axis',(0.,0.,1.));
#12435=DIRECTION('ref_axis',(1.,0.,0.));
#12436=DIRECTION('',(0.,0.,1.));
#12437=DIRECTION('center_axis',(1.,0.,0.));
#12438=DIRECTION('ref_axis',(0.,-1.,0.));
#12439=DIRECTION('',(0.,0.,1.));
#12440=DIRECTION('center_axis',(0.,0.,1.));
#12441=DIRECTION('ref_axis',(0.500000000000017,-0.866025403784429,0.));
#12442=DIRECTION('',(0.,0.,1.));
#12443=DIRECTION('center_axis',(0.500000000000017,-0.866025403784429,0.));
#12444=DIRECTION('ref_axis',(-0.866025403784429,-0.500000000000017,0.));
#12445=DIRECTION('',(0.,0.,1.));
#12446=DIRECTION('center_axis',(0.,0.,1.));
#12447=DIRECTION('ref_axis',(-0.500000000000017,-0.866025403784429,0.));
#12448=DIRECTION('',(0.,0.,1.));
#12449=DIRECTION('center_axis',(-0.500000000000017,0.866025403784429,0.));
#12450=DIRECTION('ref_axis',(0.866025403784429,0.500000000000017,0.));
#12451=DIRECTION('',(0.,0.,1.));
#12452=DIRECTION('center_axis',(0.,0.,1.));
#12453=DIRECTION('ref_axis',(-0.500000000000017,0.866025403784429,0.));
#12454=DIRECTION('',(0.,0.,1.));
#12455=DIRECTION('center_axis',(-1.,0.,0.));
#12456=DIRECTION('ref_axis',(0.,1.,0.));
#12457=DIRECTION('',(0.,2.221133174104E-14,1.));
#12458=DIRECTION('center_axis',(0.,0.,1.));
#12459=DIRECTION('ref_axis',(-1.,0.,0.));
#12460=DIRECTION('',(0.,0.,1.));
#12461=DIRECTION('center_axis',(-0.500000000000017,-0.866025403784429,0.));
#12462=DIRECTION('ref_axis',(-0.866025403784429,0.500000000000017,0.));
#12463=DIRECTION('axis',(0.,0.,1.));
#12464=DIRECTION('refdir',(1.,0.,0.));
#12465=DIRECTION('center_axis',(0.,0.,-1.));
#12466=DIRECTION('ref_axis',(1.,0.,0.));
#12467=DIRECTION('center_axis',(1.22464679914735E-16,1.,0.));
#12468=DIRECTION('ref_axis',(-1.,1.22464679914735E-16,0.));
#12469=DIRECTION('center_axis',(0.,0.,1.));
#12470=DIRECTION('ref_axis',(1.,0.,0.));
#12471=DIRECTION('axis',(0.,0.,1.));
#12472=DIRECTION('refdir',(1.,0.,0.));
#12473=DIRECTION('center_axis',(0.,1.,0.));
#12474=DIRECTION('ref_axis',(1.,0.,0.));
#12475=DIRECTION('center_axis',(0.,1.,0.));
#12476=DIRECTION('ref_axis',(1.,0.,0.));
#12477=DIRECTION('center_axis',(0.,-1.,0.));
#12478=DIRECTION('ref_axis',(1.,0.,0.));
#12479=DIRECTION('center_axis',(0.,1.,0.));
#12480=DIRECTION('ref_axis',(1.,0.,0.));
#12481=DIRECTION('',(0.,1.,0.));
#12482=DIRECTION('center_axis',(0.,-1.,0.));
#12483=DIRECTION('ref_axis',(1.,0.,0.));
#12484=DIRECTION('center_axis',(0.,1.,0.));
#12485=DIRECTION('ref_axis',(1.,0.,0.));
#12486=DIRECTION('center_axis',(0.,1.,0.));
#12487=DIRECTION('ref_axis',(1.,0.,0.));
#12488=DIRECTION('center_axis',(0.,1.,0.));
#12489=DIRECTION('ref_axis',(1.,0.,0.));
#12490=DIRECTION('',(0.,-1.,0.));
#12491=DIRECTION('axis',(0.,0.,1.));
#12492=DIRECTION('refdir',(1.,0.,0.));
#12493=DIRECTION('center_axis',(0.,0.,1.));
#12494=DIRECTION('ref_axis',(0.,1.,0.));
#12495=DIRECTION('center_axis',(0.,0.,1.));
#12496=DIRECTION('ref_axis',(0.,-1.,0.));
#12497=DIRECTION('center_axis',(0.,0.,1.));
#12498=DIRECTION('ref_axis',(0.,-1.,0.));
#12499=DIRECTION('center_axis',(0.,0.,1.));
#12500=DIRECTION('ref_axis',(0.,1.,0.));
#12501=DIRECTION('',(0.,0.,-1.));
#12502=DIRECTION('center_axis',(0.,0.,1.));
#12503=DIRECTION('ref_axis',(0.,-1.,0.));
#12504=DIRECTION('center_axis',(0.,6.12323399573676E-17,1.));
#12505=DIRECTION('ref_axis',(0.,1.,0.));
#12506=DIRECTION('center_axis',(1.,1.22464679914735E-16,0.));
#12507=DIRECTION('ref_axis',(1.22464679914735E-16,-1.,0.));
#12508=DIRECTION('center_axis',(0.,0.,1.));
#12509=DIRECTION('ref_axis',(0.,-1.,0.));
#12510=DIRECTION('center_axis',(0.,0.,1.));
#12511=DIRECTION('ref_axis',(0.,-1.,0.));
#12512=DIRECTION('',(0.,0.,1.));
#12513=DIRECTION('center_axis',(0.,0.,1.));
#12514=DIRECTION('ref_axis',(0.,-1.,0.));
#12515=DIRECTION('center_axis',(0.,6.12323399573676E-17,1.));
#12516=DIRECTION('ref_axis',(0.,1.,0.));
#12517=DIRECTION('center_axis',(-1.,-1.22464679914735E-16,0.));
#12518=DIRECTION('ref_axis',(1.22464679914735E-16,-1.,0.));
#12519=DIRECTION('',(1.,0.,0.));
#12520=DIRECTION('',(0.,0.,-1.));
#12521=DIRECTION('',(0.,-0.097582899759153,0.995227399981831));
#12522=DIRECTION('',(1.,0.,0.));
#12523=DIRECTION('',(-1.,0.,0.));
#12524=DIRECTION('',(0.,-0.097582899759153,0.995227399981831));
#12525=DIRECTION('',(0.,0.,1.));
#12526=DIRECTION('',(0.,-1.,0.));
#12527=DIRECTION('',(-1.,0.,0.));
#12528=DIRECTION('',(0.,0.,1.));
#12529=DIRECTION('',(0.,-1.,0.));
#12530=DIRECTION('',(0.,0.,-1.));
#12531=DIRECTION('',(0.,0.,1.));
#12532=DIRECTION('',(-1.,0.,0.));
#12533=DIRECTION('',(0.,0.,1.));
#12534=DIRECTION('',(1.,0.,0.));
#12535=DIRECTION('',(0.,0.,1.));
#12536=DIRECTION('',(0.,1.,0.));
#12537=DIRECTION('',(1.,0.,0.));
#12538=DIRECTION('',(0.,1.,0.));
#12539=DIRECTION('',(0.,0.,1.));
#12540=DIRECTION('',(1.,0.,0.));
#12541=DIRECTION('',(0.,1.,0.));
#12542=DIRECTION('',(-1.,0.,0.));
#12543=DIRECTION('',(-1.,0.,0.));
#12544=DIRECTION('',(0.,-1.,0.));
#12545=CARTESIAN_POINT('',(0.,0.,0.));
#12546=CARTESIAN_POINT('',(0.,0.,0.));
#12547=CARTESIAN_POINT('Origin',(-1.62,0.,0.));
#12548=CARTESIAN_POINT('',(2.35200870842004,-6.73733496176535E-9,-2.25));
#12549=CARTESIAN_POINT('',(1.56784454507149,1.7551195425239E-10,-2.24999999965197));
#12550=CARTESIAN_POINT('',(-1.62,2.75545529808154E-16,-2.25));
#12551=CARTESIAN_POINT('',(0.392128505845514,-1.44267263157291E-10,-2.24999999971305));
#12552=CARTESIAN_POINT('Ctrl Pts',(2.35200870842004,-1.34746699562149E-8,
-2.25));
#12553=CARTESIAN_POINT('Ctrl Pts',(2.33277638732405,-0.138949662434125,
-2.24999999916787));
#12554=CARTESIAN_POINT('Ctrl Pts',(2.3136433948348,-0.277617289677986,-2.23712870695244));
#12555=CARTESIAN_POINT('Ctrl Pts',(2.25366806067718,-0.703379839167081,
-2.1573828637615));
#12556=CARTESIAN_POINT('Ctrl Pts',(2.2129900387638,-0.979129299035637,-2.04703573040602));
#12557=CARTESIAN_POINT('Ctrl Pts',(2.1519494185931,-1.34948810995398,-1.80641324461668));
#12558=CARTESIAN_POINT('Ctrl Pts',(2.13161296068056,-1.46494615839442,-1.71411097634091));
#12559=CARTESIAN_POINT('Ctrl Pts',(2.09075399170948,-1.67573316142329,-1.5086415298124));
#12560=CARTESIAN_POINT('Ctrl Pts',(2.07032661889744,-1.77063375674575,-1.39604313280329));
#12561=CARTESIAN_POINT('Ctrl Pts',(2.00943863336491,-2.01920756533226,-1.03461219332703));
#12562=CARTESIAN_POINT('Ctrl Pts',(1.96964374375012,-2.13620985812946,-0.764346996059495));
#12563=CARTESIAN_POINT('Ctrl Pts',(1.90863622394457,-2.22966512019371,-0.335697586507395));
#12564=CARTESIAN_POINT('Ctrl Pts',(1.88823238081986,-2.24682944376116,-0.189372254756062));
#12565=CARTESIAN_POINT('Ctrl Pts',(1.84758268312515,-2.25236953127332,0.104468846512095));
#12566=CARTESIAN_POINT('Ctrl Pts',(1.82735396185634,-2.2407466408021,0.251267624447377));
#12567=CARTESIAN_POINT('Ctrl Pts',(1.78658703445223,-2.18899287867358,0.540823217609736));
#12568=CARTESIAN_POINT('Ctrl Pts',(1.76614227354399,-2.14892212598486,0.682869172878815));
#12569=CARTESIAN_POINT('Ctrl Pts',(1.70455376263095,-1.98749481790983,1.09536189156463));
#12570=CARTESIAN_POINT('Ctrl Pts',(1.66426251715545,-1.82648095233547,1.34681950231116));
#12571=CARTESIAN_POINT('Ctrl Pts',(1.60278209700345,-1.51969407244708,1.66570454228107));
#12572=CARTESIAN_POINT('Ctrl Pts',(1.58236836207887,-1.40782894454456,1.76126713241198));
#12573=CARTESIAN_POINT('Ctrl Pts',(1.54176994137328,-1.16750131542141,1.92894618385223));
#12574=CARTESIAN_POINT('Ctrl Pts',(1.52164437281176,-1.03967309036386,2.00074327125064));
#12575=CARTESIAN_POINT('Ctrl Pts',(1.46063877929285,-0.636221828820066,
2.17817317037249));
#12576=CARTESIAN_POINT('Ctrl Pts',(1.41990733277731,-0.345990135231769,
2.24265729999344));
#12577=CARTESIAN_POINT('Ctrl Pts',(1.35883501404012,0.0957467405484846,
2.25278719152739));
#12578=CARTESIAN_POINT('Ctrl Pts',(1.33852020218053,0.24304733990133,2.24168299296819));
#12579=CARTESIAN_POINT('Ctrl Pts',(1.29767897011706,0.532963956491612,2.19090165010054));
#12580=CARTESIAN_POINT('Ctrl Pts',(1.27724738626119,0.674898225257669,2.15142088265007));
#12581=CARTESIAN_POINT('Ctrl Pts',(1.21614110621229,1.08525868713529,1.9926333773732));
#12582=CARTESIAN_POINT('Ctrl Pts',(1.17619137834493,1.33527754707148,1.83450427328792));
#12583=CARTESIAN_POINT('Ctrl Pts',(1.11502332698973,1.65455281674558,1.53183980918237));
#12584=CARTESIAN_POINT('Ctrl Pts',(1.09461843507782,1.75101288969669,1.42057620764718));
#12585=CARTESIAN_POINT('Ctrl Pts',(1.05398607569683,1.92079184507726,1.18093297112612));
#12586=CARTESIAN_POINT('Ctrl Pts',(1.03377939642206,1.99371911206047,1.05315109711181));
#12587=CARTESIAN_POINT('Ctrl Pts',(0.993032597292335,2.11385925129569,0.784728189120789));
#12588=CARTESIAN_POINT('Ctrl Pts',(0.972585546096863,2.16068641849123,0.644693860742182));
#12589=CARTESIAN_POINT('Ctrl Pts',(0.910938101623354,2.2594151089232,0.212521738300102));
#12590=CARTESIAN_POINT('Ctrl Pts',(0.870603876065813,2.26774929129372,-0.0862475998130358));
#12591=CARTESIAN_POINT('Ctrl Pts',(0.809095780672101,2.19334836312328,-0.522750349456467));
#12592=CARTESIAN_POINT('Ctrl Pts',(0.788678651829075,2.15458504182036,-0.664687866011266));
#12593=CARTESIAN_POINT('Ctrl Pts',(0.748076415375149,2.05019231544315,-0.938386614720418));
#12594=CARTESIAN_POINT('Ctrl Pts',(0.727967451926541,1.98492979001699,-1.06953883009641));
#12595=CARTESIAN_POINT('Ctrl Pts',(0.66695908632401,1.75109360472821,-1.44326800323482));
#12596=CARTESIAN_POINT('Ctrl Pts',(0.62618961791159,1.54720453400115,-1.65997389246564));
#12597=CARTESIAN_POINT('Ctrl Pts',(0.56940574368058,1.21284296473895,-1.89868238190458));
#12598=CARTESIAN_POINT('Ctrl Pts',(0.553392895611178,1.11326053025777,-1.95873245111983));
#12599=CARTESIAN_POINT('Ctrl Pts',(0.513121790218507,0.853450251020534,
-2.08916451042388));
#12600=CARTESIAN_POINT('Ctrl Pts',(0.488882293379238,0.688823957401331,
-2.14907018596128));
#12601=CARTESIAN_POINT('Ctrl Pts',(0.440333302359495,0.348906643869198,
-2.2296414081572));
#12602=CARTESIAN_POINT('Ctrl Pts',(0.416310037109522,0.174759273682914,
-2.25000000001581));
#12603=CARTESIAN_POINT('Ctrl Pts',(0.392128506274274,-2.03592837033639E-10,
-2.25));
#12604=CARTESIAN_POINT('',(-1.12,0.,-2.25));
#12605=CARTESIAN_POINT('',(-1.62,2.75545529808154E-16,-2.25));
#12606=CARTESIAN_POINT('Origin',(-1.12,0.,0.));
#12607=CARTESIAN_POINT('',(0.392,0.,-2.25));
#12608=CARTESIAN_POINT('Origin',(-1.62,0.,0.));
#12609=CARTESIAN_POINT('',(4.31209250605754,-4.71354290851659E-8,-2.25));
#12610=CARTESIAN_POINT('',(3.52798225106248,1.06028063402371E-8,-2.25));
#12611=CARTESIAN_POINT('',(-1.62,2.75545529808154E-16,-2.25));
#12612=CARTESIAN_POINT('Ctrl Pts',(4.31209251248913,-4.8029842897669E-8,
-2.25));
#12613=CARTESIAN_POINT('Ctrl Pts',(4.3096836921749,-0.0173186732513607,
-2.24999999963031));
#12614=CARTESIAN_POINT('Ctrl Pts',(4.30727412907853,-0.0346409650931408,
-2.24980004305779));
#12615=CARTESIAN_POINT('Ctrl Pts',(4.26390032233211,-0.346378474343082,
-2.24259857970738));
#12616=CARTESIAN_POINT('Ctrl Pts',(4.22372857992966,-0.636620042927198,
-2.17806075975736));
#12617=CARTESIAN_POINT('Ctrl Pts',(4.16255591602526,-1.0400654841798,-2.00053948582208));
#12618=CARTESIAN_POINT('Ctrl Pts',(4.14221936692873,-1.16788321487765,-1.92871521092846));
#12619=CARTESIAN_POINT('Ctrl Pts',(4.10153463416861,-1.40816256393229,-1.76099865177231));
#12620=CARTESIAN_POINT('Ctrl Pts',(4.08133681215282,-1.52000051536649,-1.66542465736685));
#12621=CARTESIAN_POINT('Ctrl Pts',(4.02014872279012,-1.82670962668572,-1.34650379086338));
#12622=CARTESIAN_POINT('Ctrl Pts',(3.97923702176023,-1.98766869768262,-1.09504016666849));
#12623=CARTESIAN_POINT('Ctrl Pts',(3.91797084687114,-2.1490285267146,-0.682536143298372));
#12624=CARTESIAN_POINT('Ctrl Pts',(3.89769729492075,-2.18907646066102,-0.540483248301418));
#12625=CARTESIAN_POINT('Ctrl Pts',(3.85692869629777,-2.24078837892765,-0.250906415087508));
#12626=CARTESIAN_POINT('Ctrl Pts',(3.83652802221641,-2.25238725782488,-0.104092586806907));
#12627=CARTESIAN_POINT('Ctrl Pts',(3.79566850402458,-2.2467980137086,0.189719065307968));
#12628=CARTESIAN_POINT('Ctrl Pts',(3.77539635985123,-2.22961601599269,0.336022905307451));
#12629=CARTESIAN_POINT('Ctrl Pts',(3.71475827653615,-2.13609374147413,0.76468053512841));
#12630=CARTESIAN_POINT('Ctrl Pts',(3.67444889417311,-2.01903786410996,1.03494295741834));
#12631=CARTESIAN_POINT('Ctrl Pts',(3.61365957837694,-1.77041013913102,1.39632589673724));
#12632=CARTESIAN_POINT('Ctrl Pts',(3.59344857673001,-1.6754969521165,1.50890339956332));
#12633=CARTESIAN_POINT('Ctrl Pts',(3.55270646116513,-1.46466091956622,1.71435719882085));
#12634=CARTESIAN_POINT('Ctrl Pts',(3.53226843656,-1.34917295652032,1.80664890853136));
#12635=CARTESIAN_POINT('Ctrl Pts',(3.47083314749689,-0.978766159167189,
2.0472098780982));
#12636=CARTESIAN_POINT('Ctrl Pts',(3.43067952500035,-0.702981415412188,
2.15751642705047));
#12637=CARTESIAN_POINT('Ctrl Pts',(3.36954546604559,-0.269851280770565,
2.23855388857242));
#12638=CARTESIAN_POINT('Ctrl Pts',(3.34919136760675,-0.123629571159131,
2.25136791167734));
#12639=CARTESIAN_POINT('Ctrl Pts',(3.30846337269836,0.169554513911013,2.24839775051071));
#12640=CARTESIAN_POINT('Ctrl Pts',(3.28825578849117,0.315822445267529,2.23255470585241));
#12641=CARTESIAN_POINT('Ctrl Pts',(3.22715306326724,0.748446928600913,2.14229924286184));
#12642=CARTESIAN_POINT('Ctrl Pts',(3.18632278838618,1.02271595912037,2.02575126538499));
#12643=CARTESIAN_POINT('Ctrl Pts',(3.12512300392732,1.38827462433469,1.77675178903506));
#12644=CARTESIAN_POINT('Ctrl Pts',(3.10486681051267,1.5014717162221,1.68218171628064));
#12645=CARTESIAN_POINT('Ctrl Pts',(3.06410287513668,1.70772615377232,1.47234662177451));
#12646=CARTESIAN_POINT('Ctrl Pts',(3.04368915577137,1.80029296917859,1.35759899910148));
#12647=CARTESIAN_POINT('Ctrl Pts',(3.00278457893002,1.96169182729548,1.11170665051441));
#12648=CARTESIAN_POINT('Ctrl Pts',(2.98247979590209,2.03014491871399,0.981143626178216));
#12649=CARTESIAN_POINT('Ctrl Pts',(2.92212349573607,2.19412631916938,0.576373576555818));
#12650=CARTESIAN_POINT('Ctrl Pts',(2.88214235426619,2.25002453221374,0.289429263379427));
#12651=CARTESIAN_POINT('Ctrl Pts',(2.80180325462564,2.24997545071142,-0.289821426149872));
#12652=CARTESIAN_POINT('Ctrl Pts',(2.76226046746642,2.1940276179487,-0.576737472505687));
#12653=CARTESIAN_POINT('Ctrl Pts',(2.70152461771704,2.02999121891702,-0.981461835728237));
#12654=CARTESIAN_POINT('Ctrl Pts',(2.68112151868365,1.96150972560333,-1.11203260815236));
#12655=CARTESIAN_POINT('Ctrl Pts',(2.64044620380749,1.80004928023798,-1.35792161134074));
#12656=CARTESIAN_POINT('Ctrl Pts',(2.6201897172147,1.70747036178314,-1.47264103442275));
#12657=CARTESIAN_POINT('Ctrl Pts',(2.57939813892615,1.50119327929904,-1.68243069966521));
#12658=CARTESIAN_POINT('Ctrl Pts',(2.55895696088971,1.38797891913171,-1.77698237260967));
#12659=CARTESIAN_POINT('Ctrl Pts',(2.49747399935976,1.02236832477551,-2.02592944165093));
#12660=CARTESIAN_POINT('Ctrl Pts',(2.45725819439494,0.748063370721404,-2.14243526276714));
#12661=CARTESIAN_POINT('Ctrl Pts',(2.39583737585762,0.315405218933968,-2.23261384171523));
#12662=CARTESIAN_POINT('Ctrl Pts',(2.37542727449016,0.169119063455048,-2.24843215995123));
#12663=CARTESIAN_POINT('Ctrl Pts',(2.3540695508737,0.0148876676420556,-2.24996306357395));
#12664=CARTESIAN_POINT('Ctrl Pts',(2.35303897077726,0.0074434246915941,
-2.25000000004458));
#12665=CARTESIAN_POINT('Ctrl Pts',(2.35200870842004,-1.34746697823107E-8,
-2.25));
#12666=CARTESIAN_POINT('Ctrl Pts',(1.56784454455142,2.47754351756502E-10,
-2.25));
#12667=CARTESIAN_POINT('Ctrl Pts',(1.59211895035072,0.17479682892967,-2.24999999998075));
#12668=CARTESIAN_POINT('Ctrl Pts',(1.61641651664107,0.348995564145036,-2.22963234048382));
#12669=CARTESIAN_POINT('Ctrl Pts',(1.66478847007177,0.689026197844474,-2.1490102399816));
#12670=CARTESIAN_POINT('Ctrl Pts',(1.68879344734741,0.853692883134347,-2.08906901944099));
#12671=CARTESIAN_POINT('Ctrl Pts',(1.72911468700117,1.11355858179884,-1.95856528032236));
#12672=CARTESIAN_POINT('Ctrl Pts',(1.74524575915888,1.21315915341977,-1.89848197821454));
#12673=CARTESIAN_POINT('Ctrl Pts',(1.80239810265935,1.54751075606308,-1.65969083865729));
#12674=CARTESIAN_POINT('Ctrl Pts',(1.8425875741646,1.75137701442023,-1.44293043674562));
#12675=CARTESIAN_POINT('Ctrl Pts',(1.9037906929622,1.98515120720636,-1.06912759367124));
#12676=CARTESIAN_POINT('Ctrl Pts',(1.92411338573857,2.0503869387489,-0.937961715305248));
#12677=CARTESIAN_POINT('Ctrl Pts',(1.96476482028555,2.15471718118683,-0.664255413906532));
#12678=CARTESIAN_POINT('Ctrl Pts',(1.98495972725598,2.19345036446728,-0.522321200366432));
#12679=CARTESIAN_POINT('Ctrl Pts',(2.04619880723112,2.26776069914933,-0.0858385456680671));
#12680=CARTESIAN_POINT('Ctrl Pts',(2.08715131373674,2.25937622499644,0.212900405402588));
#12681=CARTESIAN_POINT('Ctrl Pts',(2.14845223284548,2.16058263016293,0.645044248508482));
#12682=CARTESIAN_POINT('Ctrl Pts',(2.16874000501105,2.11373097647935,0.785072614123205));
#12683=CARTESIAN_POINT('Ctrl Pts',(2.20951134791998,1.99354329671921,1.0534861431364));
#12684=CARTESIAN_POINT('Ctrl Pts',(2.22990026726523,1.9205878078923,1.18126534091795));
#12685=CARTESIAN_POINT('Ctrl Pts',(2.27072327240798,1.75078233631504,1.42085711461194));
#12686=CARTESIAN_POINT('Ctrl Pts',(2.29097278202136,1.65431840297454,1.53209280458974));
#12687=CARTESIAN_POINT('Ctrl Pts',(2.35178136990745,1.33499069778918,1.83471469093413));
#12688=CARTESIAN_POINT('Ctrl Pts',(2.39228770211503,1.08494074352961,1.99280530690906));
#12689=CARTESIAN_POINT('Ctrl Pts',(2.45323161358009,0.674566773852937,2.15152456699413));
#12690=CARTESIAN_POINT('Ctrl Pts',(2.47345385186549,0.532632319946515,2.1909819434057));
#12691=CARTESIAN_POINT('Ctrl Pts',(2.51420325307758,0.242686200374217,2.24172393096506));
#12692=CARTESIAN_POINT('Ctrl Pts',(2.53463709303976,0.0953672317794488,
2.25280354062975));
#12693=CARTESIAN_POINT('Ctrl Pts',(2.59610004747896,-0.346381125090515,
2.24259817496518));
#12694=CARTESIAN_POINT('Ctrl Pts',(2.63627179232953,-0.636622652438412,
2.17806000181052));
#12695=CARTESIAN_POINT('Ctrl Pts',(2.69744446087517,-1.04006789323018,2.00053823197433));
#12696=CARTESIAN_POINT('Ctrl Pts',(2.71778100791431,-1.16788552105996,1.92871381304625));
#12697=CARTESIAN_POINT('Ctrl Pts',(2.75846573572112,-1.40816465574277,1.76099697910864));
#12698=CARTESIAN_POINT('Ctrl Pts',(2.77866355700581,-1.52000249393371,1.66542285158641));
#12699=CARTESIAN_POINT('Ctrl Pts',(2.83985165482856,-1.82671126135403,1.34650158425958));
#12700=CARTESIAN_POINT('Ctrl Pts',(2.88076336322876,-1.98767005323287,1.09503771980515));
#12701=CARTESIAN_POINT('Ctrl Pts',(2.94202954427547,-2.14902938680981,0.682533437385133));
#12702=CARTESIAN_POINT('Ctrl Pts',(2.96230309827855,-2.18907714428284,0.540480482169972));
#12703=CARTESIAN_POINT('Ctrl Pts',(3.00307169736765,-2.24078869377107,0.250903592223416));
#12704=CARTESIAN_POINT('Ctrl Pts',(3.0234723698216,-2.25238738686191,0.104089768228522));
#12705=CARTESIAN_POINT('Ctrl Pts',(3.06433188272785,-2.24679777808941,-0.189721846837428));
#12706=CARTESIAN_POINT('Ctrl Pts',(3.08460402337628,-2.22961560096571,-0.336025654074097));
#12707=CARTESIAN_POINT('Ctrl Pts',(3.14524213459954,-2.13609275790457,-0.764683362701376));
#12708=CARTESIAN_POINT('Ctrl Pts',(3.18555154937213,-2.0190364256806,-1.03494582298224));
#12709=CARTESIAN_POINT('Ctrl Pts',(3.24634089062226,-1.77040803178236,-1.39632856968566));
#12710=CARTESIAN_POINT('Ctrl Pts',(3.26655189380965,-1.67549466831335,-1.50890593643214));
#12711=CARTESIAN_POINT('Ctrl Pts',(3.30729401050766,-1.46465832691475,-1.71435941266956));
#12712=CARTESIAN_POINT('Ctrl Pts',(3.32773203467332,-1.34917023535203,-1.80665093953558));
#12713=CARTESIAN_POINT('Ctrl Pts',(3.3891673279893,-0.978763052959974,-2.04721136927531));
#12714=CARTESIAN_POINT('Ctrl Pts',(3.42932095269871,-0.702978100313755,
-2.1575175129611));
#12715=CARTESIAN_POINT('Ctrl Pts',(3.48940060268209,-0.277318270540816,
-2.2371566154978));
#12716=CARTESIAN_POINT('Ctrl Pts',(3.50869452424106,-0.13879770411982,-2.25000000066645));
#12717=CARTESIAN_POINT('Ctrl Pts',(3.52798224961699,1.08036556437097E-8,
-2.25));
#12718=CARTESIAN_POINT('Origin',(-1.62,0.,0.));
#12719=CARTESIAN_POINT('',(6.27207431538479,-3.77424972188349E-8,-2.25));
#12720=CARTESIAN_POINT('',(5.48792568467742,3.79675638141282E-8,-2.25));
#12721=CARTESIAN_POINT('',(-1.62,2.75545529808154E-16,-2.25));
#12722=CARTESIAN_POINT('',(5.29204615187795,3.82768812034955E-6,2.2500376859885));
#12723=CARTESIAN_POINT('Ctrl Pts',(6.27207432050307,-3.84499440619912E-8,
-2.25));
#12724=CARTESIAN_POINT('Ctrl Pts',(6.25408532734062,-0.130165591604654,
-2.24999999777562));
#12725=CARTESIAN_POINT('Ctrl Pts',(6.23611633433344,-0.260113717555053,
-2.2387046819596));
#12726=CARTESIAN_POINT('Ctrl Pts',(6.19765297673759,-0.533145965110677,
-2.19085732779874));
#12727=CARTESIAN_POINT('Ctrl Pts',(6.17722142712748,-0.675076412010008,
-2.15136493955894));
#12728=CARTESIAN_POINT('Ctrl Pts',(6.11611677525103,-1.08541438319642,-1.99254717511697));
#12729=CARTESIAN_POINT('Ctrl Pts',(6.07616819926228,-1.33541291644883,-1.83440421567511));
#12730=CARTESIAN_POINT('Ctrl Pts',(6.01500131723825,-1.6546604838004,-1.53172356103907));
#12731=CARTESIAN_POINT('Ctrl Pts',(5.99459643609767,-1.75111308725479,-1.42045275172777));
#12732=CARTESIAN_POINT('Ctrl Pts',(5.95396394316539,-1.92087604585497,-1.18079614519214));
#12733=CARTESIAN_POINT('Ctrl Pts',(5.93375707907688,-1.99379472607352,-1.05300809263716));
#12734=CARTESIAN_POINT('Ctrl Pts',(5.89301010919162,-2.11391569789108,-0.784576015091131));
#12735=CARTESIAN_POINT('Ctrl Pts',(5.87256307521049,-2.1607326268593,-0.644538848405556));
#12736=CARTESIAN_POINT('Ctrl Pts',(5.81091604648748,-2.25942987283393,-0.212362060682051));
#12737=CARTESIAN_POINT('Ctrl Pts',(5.77058213474394,-2.26774301450112,0.0864058887794901));
#12738=CARTESIAN_POINT('Ctrl Pts',(5.70907421085162,-2.19331233614171,0.522901439395613));
#12739=CARTESIAN_POINT('Ctrl Pts',(5.68865711036259,-2.15453928606102,0.664836132781844));
#12740=CARTESIAN_POINT('Ctrl Pts',(5.64805491001764,-2.05012742522628,0.938528535781674));
#12741=CARTESIAN_POINT('Ctrl Pts',(5.62794579809253,-1.9848553301936,1.06967714620222));
#12742=CARTESIAN_POINT('Ctrl Pts',(5.56693746455699,-1.75099350503924,1.44338901773155));
#12743=CARTESIAN_POINT('Ctrl Pts',(5.52616833815168,-1.54709100449272,1.66007933403282));
#12744=CARTESIAN_POINT('Ctrl Pts',(5.46938273005178,-1.21270280996112,1.89877282192696));
#12745=CARTESIAN_POINT('Ctrl Pts',(5.45336778929448,-1.11310280591162,1.95882297685515));
#12746=CARTESIAN_POINT('Ctrl Pts',(5.41309150365977,-0.853248456719158,
2.08924873488907));
#12747=CARTESIAN_POINT('Ctrl Pts',(5.38884891316524,-0.688595612688673,
2.14914511344005));
#12748=CARTESIAN_POINT('Ctrl Pts',(5.34030897001841,-0.348730902642399,
2.22966222455927));
#12749=CARTESIAN_POINT('Ctrl Pts',(5.31629606784201,-0.174658290764173,
2.2500011638322));
#12750=CARTESIAN_POINT('Ctrl Pts',(5.29212643182535,1.49921888440568E-5,
2.24999999995005));
#12751=CARTESIAN_POINT('Ctrl Pts',(5.29215286593614,1.86469866857858E-5,
2.24999999992273));
#12752=CARTESIAN_POINT('Ctrl Pts',(5.26788459471967,0.174771258645414,2.24999855165179));
#12753=CARTESIAN_POINT('Ctrl Pts',(5.24359172922835,0.348936080922872,2.22963821621658));
#12754=CARTESIAN_POINT('Ctrl Pts',(5.19522294699834,0.688947458703098,2.1490371277111));
#12755=CARTESIAN_POINT('Ctrl Pts',(5.17121524420815,0.85363528418937,2.08909424764715));
#12756=CARTESIAN_POINT('Ctrl Pts',(5.13088935441657,1.11353358772044,1.95858029077967));
#12757=CARTESIAN_POINT('Ctrl Pts',(5.11475641692752,1.21314635881947,1.89849097930423));
#12758=CARTESIAN_POINT('Ctrl Pts',(5.05760220103249,1.54750914204975,1.65969233824127));
#12759=CARTESIAN_POINT('Ctrl Pts',(5.01741273190551,1.75137559127931,1.44293215801028));
#12760=CARTESIAN_POINT('Ctrl Pts',(4.956209617063,1.98515014899732,1.06912956060157));
#12761=CARTESIAN_POINT('Ctrl Pts',(4.93588692261656,2.05038601671524,0.937963733178924));
#12762=CARTESIAN_POINT('Ctrl Pts',(4.89523548415118,2.15471653107058,0.664257522211146));
#12763=CARTESIAN_POINT('Ctrl Pts',(4.87504057714961,2.19344985264303,0.522323349061616));
#12764=CARTESIAN_POINT('Ctrl Pts',(4.81380150253075,2.26776061051127,0.0858407957701425));
#12765=CARTESIAN_POINT('Ctrl Pts',(4.77284899967315,2.25937643530655,-0.212898136213141));
#12766=CARTESIAN_POINT('Ctrl Pts',(4.71154808385884,2.16058328727759,-0.645042045642452));
#12767=CARTESIAN_POINT('Ctrl Pts',(4.69126031340649,2.11373177917323,-0.785070451457586));
#12768=CARTESIAN_POINT('Ctrl Pts',(4.65048897078392,1.99354437168984,-1.05348411115453));
#12769=CARTESIAN_POINT('Ctrl Pts',(4.63010004997872,1.92058900476889,-1.18126339690632));
#12770=CARTESIAN_POINT('Ctrl Pts',(4.58927704048005,1.75078376058498,-1.42085536040784));
#12771=CARTESIAN_POINT('Ctrl Pts',(4.56902752837063,1.65431993345513,-1.53209115275161));
#12772=CARTESIAN_POINT('Ctrl Pts',(4.5082189584666,1.33499262069522,-1.83471327046107));
#12773=CARTESIAN_POINT('Ctrl Pts',(4.46771264686281,1.08494295367164,-1.99280408393575));
#12774=CARTESIAN_POINT('Ctrl Pts',(4.4067687515742,0.674569302753384,-2.15152377353736));
#12775=CARTESIAN_POINT('Ctrl Pts',(4.38654651469855,0.532634903269586,-2.19098131485047));
#12776=CARTESIAN_POINT('Ctrl Pts',(4.34819606392266,0.259758194840745,-2.23873640467835));
#12777=CARTESIAN_POINT('Ctrl Pts',(4.33017143806453,0.129981476370136,-2.25000000277466));
#12778=CARTESIAN_POINT('Ctrl Pts',(4.31209251248913,-4.80298429847426E-8,
-2.25));
#12779=CARTESIAN_POINT('Ctrl Pts',(3.52798224961699,1.08036555900686E-8,
-2.25));
#12780=CARTESIAN_POINT('Ctrl Pts',(3.52903809419908,0.00759804595041996,
-2.24999999996352));
#12781=CARTESIAN_POINT('Ctrl Pts',(3.53009386946379,0.0151969186709084,
-2.24996151317907));
#12782=CARTESIAN_POINT('Ctrl Pts',(3.55153710138858,0.169557933752482,-2.24839749237712));
#12783=CARTESIAN_POINT('Ctrl Pts',(3.57174468363663,0.315825837333526,-2.2325542257493));
#12784=CARTESIAN_POINT('Ctrl Pts',(3.63284742363824,0.748450276953202,-2.14229808671015));
#12785=CARTESIAN_POINT('Ctrl Pts',(3.67367771353097,1.02271921695567,-2.02574963515858));
#12786=CARTESIAN_POINT('Ctrl Pts',(3.73487751004098,1.38827756485256,-1.77674949253261));
#12787=CARTESIAN_POINT('Ctrl Pts',(3.75513370599362,1.50147451002373,-1.68217922372651));
#12788=CARTESIAN_POINT('Ctrl Pts',(3.79589764216434,1.70772859083133,-1.47234379280653));
#12789=CARTESIAN_POINT('Ctrl Pts',(3.81631135973467,1.80029520233142,-1.35759603527156));
#12790=CARTESIAN_POINT('Ctrl Pts',(3.8572159299359,1.96169363605914,-1.11170345647742));
#12791=CARTESIAN_POINT('Ctrl Pts',(3.87752070776928,2.03014650713162,-0.981140336813649));
#12792=CARTESIAN_POINT('Ctrl Pts',(3.93787705708652,2.19412738785583,-0.576369694984279));
#12793=CARTESIAN_POINT('Ctrl Pts',(3.97785825589419,2.2500251408795,-0.289424903347084));
#12794=CARTESIAN_POINT('Ctrl Pts',(4.05819741292109,2.24997484101667,0.289826277868796));
#12795=CARTESIAN_POINT('Ctrl Pts',(4.09774022238688,2.19402635884467,0.576742322258415));
#12796=CARTESIAN_POINT('Ctrl Pts',(4.15847609373613,2.02998899065074,0.981466448251175));
#12797=CARTESIAN_POINT('Ctrl Pts',(4.17887919265677,1.96150718828485,1.11203708702209));
#12798=CARTESIAN_POINT('Ctrl Pts',(4.21955451327411,1.80004614748845,1.35792576754677));
#12799=CARTESIAN_POINT('Ctrl Pts',(4.23981100566145,1.70746694325715,1.4726450012244));
#12800=CARTESIAN_POINT('Ctrl Pts',(4.28060258902202,1.50118936105739,1.68243419423437));
#12801=CARTESIAN_POINT('Ctrl Pts',(4.30104376623934,1.38797479489467,1.77698559252924));
#12802=CARTESIAN_POINT('Ctrl Pts',(4.36252670165228,1.02236375565302,2.02593172692336));
#12803=CARTESIAN_POINT('Ctrl Pts',(4.40274248808703,0.748058676427634,2.14243688239479));
#12804=CARTESIAN_POINT('Ctrl Pts',(4.46416329089555,0.315400465914695,2.23261451352336));
#12805=CARTESIAN_POINT('Ctrl Pts',(4.48457339157346,0.169114271160377,2.24843252078476));
#12806=CARTESIAN_POINT('Ctrl Pts',(4.52517609820414,-0.124091736174342,
2.25134226315683));
#12807=CARTESIAN_POINT('Ctrl Pts',(4.54532642928959,-0.270304179716033,
2.23849878605978));
#12808=CARTESIAN_POINT('Ctrl Pts',(4.60633261296772,-0.703384484216852,
2.15738134133833));
#12809=CARTESIAN_POINT('Ctrl Pts',(4.64701062369311,-0.979133652254152,
2.04703363983638));
#12810=CARTESIAN_POINT('Ctrl Pts',(4.70805123769189,-1.34949192457293,1.80641039645255));
#12811=CARTESIAN_POINT('Ctrl Pts',(4.72838769996192,-1.46494979275193,1.71410787190213));
#12812=CARTESIAN_POINT('Ctrl Pts',(4.76924667246394,-1.6757363624887,1.50863797289603));
#12813=CARTESIAN_POINT('Ctrl Pts',(4.78967404439193,-1.77063671067734,1.39603938489405));
#12814=CARTESIAN_POINT('Ctrl Pts',(4.8505619800633,-2.0192095809236,1.03460817590125));
#12815=CARTESIAN_POINT('Ctrl Pts',(4.89035683420762,-2.136211235017,0.764343034593591));
#12816=CARTESIAN_POINT('Ctrl Pts',(4.95136431657638,-2.22966570058694,0.335693738657983));
#12817=CARTESIAN_POINT('Ctrl Pts',(4.97176815953602,-2.24682977301417,0.189368360942901));
#12818=CARTESIAN_POINT('Ctrl Pts',(5.01241786106949,-2.25236934995637,-0.104472792493422));
#12819=CARTESIAN_POINT('Ctrl Pts',(5.03264658685133,-2.24074619937062,-0.251271576130403));
#12820=CARTESIAN_POINT('Ctrl Pts',(5.0734135183212,-2.18899192118144,-0.540827089300053));
#12821=CARTESIAN_POINT('Ctrl Pts',(5.09385827870535,-2.14892092142864,-0.682872960558762));
#12822=CARTESIAN_POINT('Ctrl Pts',(5.15544677542526,-1.98749291968624,-1.09536531654571));
#12823=CARTESIAN_POINT('Ctrl Pts',(5.19573801061881,-1.82647866393059,-1.34682258994401));
#12824=CARTESIAN_POINT('Ctrl Pts',(5.25721842344305,-1.51969130410301,-1.66570706791729));
#12825=CARTESIAN_POINT('Ctrl Pts',(5.27763215772858,-1.40782601752243,-1.76126947206421));
#12826=CARTESIAN_POINT('Ctrl Pts',(5.31823057856148,-1.16749808807915,-1.92894813920351));
#12827=CARTESIAN_POINT('Ctrl Pts',(5.3383561510158,-1.03966971950341,-2.0007450247888));
#12828=CARTESIAN_POINT('Ctrl Pts',(5.39936174428246,-0.636218178201016,
-2.17817423002739));
#12829=CARTESIAN_POINT('Ctrl Pts',(5.44009318222189,-0.34598642648124,-2.24265786574736));
#12830=CARTESIAN_POINT('Ctrl Pts',(5.48317363486213,-0.0343849350021253,
-2.24980298931542));
#12831=CARTESIAN_POINT('Ctrl Pts',(5.48554992285105,-0.0171905666706365,
-2.25000000029552));
#12832=CARTESIAN_POINT('Ctrl Pts',(5.48792567952862,3.86792288330504E-8,
-2.25));
#12833=CARTESIAN_POINT('Origin',(-1.62,0.,0.));
#12834=CARTESIAN_POINT('',(8.23201774889606,-1.07519836100082E-8,-2.25));
#12835=CARTESIAN_POINT('',(7.44790749394411,4.71413583506493E-8,-2.25));
#12836=CARTESIAN_POINT('',(-1.62,2.75545529808154E-16,-2.25));
#12837=CARTESIAN_POINT('Ctrl Pts',(8.23201775036189,-1.09556604927598E-8,
-2.25));
#12838=CARTESIAN_POINT('Ctrl Pts',(8.23095406960136,-0.0076544365601514,
-2.24999999996273));
#12839=CARTESIAN_POINT('Ctrl Pts',(8.22989045929263,-0.0153097114686535,
-2.24996093978238));
#12840=CARTESIAN_POINT('Ctrl Pts',(8.20843948292972,-0.169726843614622,
-2.24838473640397));
#12841=CARTESIAN_POINT('Ctrl Pts',(8.18823199726517,-0.31599337566833,-2.23253050637012));
#12842=CARTESIAN_POINT('Ctrl Pts',(8.1271285281988,-0.748615648616462,-2.14224097734124));
#12843=CARTESIAN_POINT('Ctrl Pts',(8.08629749799337,-1.0228801106048,-2.02566911458184));
#12844=CARTESIAN_POINT('Ctrl Pts',(8.0250971071162,-1.38842278055941,-1.77663607139859));
#12845=CARTESIAN_POINT('Ctrl Pts',(8.00484078578692,-1.50161247962248,-1.68205612062705));
#12846=CARTESIAN_POINT('Ctrl Pts',(7.96407681040092,-1.70784894142048,-1.47220407654263));
#12847=CARTESIAN_POINT('Ctrl Pts',(7.94366318154694,-1.80040548235535,-1.3574496594755));
#12848=CARTESIAN_POINT('Ctrl Pts',(7.90275893934824,-1.96178295692203,-1.1115457126321));
#12849=CARTESIAN_POINT('Ctrl Pts',(7.88245441796761,-2.03022494603235,-0.980977885241562));
#12850=CARTESIAN_POINT('Ctrl Pts',(7.82209564580445,-2.19418014489188,-0.57617802840078));
#12851=CARTESIAN_POINT('Ctrl Pts',(7.7821116220244,-2.25005518612483,-0.289209643824882));
#12852=CARTESIAN_POINT('Ctrl Pts',(7.70176962959587,-2.24994473140811,0.290065825880358));
#12853=CARTESIAN_POINT('Ctrl Pts',(7.66222571526396,-2.1939641725135,0.576981779026868));
#12854=CARTESIAN_POINT('Ctrl Pts',(7.60148878147473,-2.02987896698876,0.981694164661813));
#12855=CARTESIAN_POINT('Ctrl Pts',(7.58108568810569,-1.96138190649418,1.11225820465269));
#12856=CARTESIAN_POINT('Ctrl Pts',(7.54041008390259,-1.79989146956541,1.35813095322165));
#12857=CARTESIAN_POINT('Ctrl Pts',(7.52015330548745,-1.70729815730867,1.47284083444354));
#12858=CARTESIAN_POINT('Ctrl Pts',(7.47936147180096,-1.50099590571904,1.68260671123367));
#12859=CARTESIAN_POINT('Ctrl Pts',(7.45892033505228,-1.38777117021646,1.77714454947763));
#12860=CARTESIAN_POINT('Ctrl Pts',(7.39743869110616,-1.0221381803978,2.02604453173824));
#12861=CARTESIAN_POINT('Ctrl Pts',(7.35722382091421,-0.747826936732087,
2.14251682117079));
#12862=CARTESIAN_POINT('Ctrl Pts',(7.29580379636594,-0.315165842380389,
2.23264766329073));
#12863=CARTESIAN_POINT('Ctrl Pts',(7.2753937296875,-0.168877708232943,2.24845032000289));
#12864=CARTESIAN_POINT('Ctrl Pts',(7.23479094383233,0.124330601794713,2.25132919560883));
#12865=CARTESIAN_POINT('Ctrl Pts',(7.21464034989432,0.270543380370812,2.23846999940466));
#12866=CARTESIAN_POINT('Ctrl Pts',(7.15363413279597,0.703613780870449,2.15730617596627));
#12867=CARTESIAN_POINT('Ctrl Pts',(7.11295667378843,0.979348546673183,2.04693042658809));
#12868=CARTESIAN_POINT('Ctrl Pts',(7.05191636363925,1.3496802322424,1.80626978190683));
#12869=CARTESIAN_POINT('Ctrl Pts',(7.03157968634747,1.46512920013272,1.71395460692825));
#12870=CARTESIAN_POINT('Ctrl Pts',(6.99072053963046,1.67589437825013,1.50846237224991));
#12871=CARTESIAN_POINT('Ctrl Pts',(6.97029321134451,1.77078252607677,1.39585435600291));
#12872=CARTESIAN_POINT('Ctrl Pts',(6.90940773937468,2.01930906556166,1.03440985658292));
#12873=CARTESIAN_POINT('Ctrl Pts',(6.86961463792993,2.13627918649898,0.764147494529221));
#12874=CARTESIAN_POINT('Ctrl Pts',(6.80860900574881,2.22969433797703,0.335503824874883));
#12875=CARTESIAN_POINT('Ctrl Pts',(6.78820517091419,2.24684601517249,0.189176178485125));
#12876=CARTESIAN_POINT('Ctrl Pts',(6.74755527979027,2.2523603923114,-0.104667548958869));
#12877=CARTESIAN_POINT('Ctrl Pts',(6.72732633127926,2.24072440354504,-0.251466613113482));
#12878=CARTESIAN_POINT('Ctrl Pts',(6.68655919917942,2.18894465508701,-0.541018176731977));
#12879=CARTESIAN_POINT('Ctrl Pts',(6.66611446468501,2.14886146155801,-0.683059901069027));
#12880=CARTESIAN_POINT('Ctrl Pts',(6.60452666954551,1.98739922685157,-1.09553434819301));
#12881=CARTESIAN_POINT('Ctrl Pts',(6.56423594252792,1.82636571910927,-1.34697496578364));
#12882=CARTESIAN_POINT('Ctrl Pts',(6.50275589222393,1.51955467963752,-1.66583170377288));
#12883=CARTESIAN_POINT('Ctrl Pts',(6.48234218945987,1.40768156186358,-1.76138492976101));
#12884=CARTESIAN_POINT('Ctrl Pts',(6.44174376210382,1.16733881115099,-1.92904463122872));
#12885=CARTESIAN_POINT('Ctrl Pts',(6.4216179974731,1.03950335999851,-2.00083155686855));
#12886=CARTESIAN_POINT('Ctrl Pts',(6.36061241652338,0.636038013123998,-2.17822651786486));
#12887=CARTESIAN_POINT('Ctrl Pts',(6.31988140189253,0.345803393089197,-2.24268577897185));
#12888=CARTESIAN_POINT('Ctrl Pts',(6.27680967342241,0.0342641567769058,
-2.24980437079299));
#12889=CARTESIAN_POINT('Ctrl Pts',(6.27444173288307,0.017130188862149,-2.25000000029274));
#12890=CARTESIAN_POINT('Ctrl Pts',(6.27207432050307,-3.84499440678469E-8,
-2.25));
#12891=CARTESIAN_POINT('',(6.46795384919627,-3.82950037302251E-6,2.25003768627347));
#12892=CARTESIAN_POINT('Ctrl Pts',(5.48792567952862,3.86792289516769E-8,
-2.25));
#12893=CARTESIAN_POINT('Ctrl Pts',(5.50590617826707,0.130104127504668,-2.24999999776341));
#12894=CARTESIAN_POINT('Ctrl Pts',(5.52386671666605,0.259991227284445,-2.23871534675092));
#12895=CARTESIAN_POINT('Ctrl Pts',(5.5623215461235,0.532967571307075,-2.19090076998503));
#12896=CARTESIAN_POINT('Ctrl Pts',(5.5827531292993,0.674901764174861,-2.15141977173756));
#12897=CARTESIAN_POINT('Ctrl Pts',(5.64385937703691,1.08526177954693,-1.99263166541714));
#12898=CARTESIAN_POINT('Ctrl Pts',(5.6838090820455,1.3352802359164,-1.83450228602105));
#12899=CARTESIAN_POINT('Ctrl Pts',(5.74497711019981,1.65455495546337,-1.53183750016682));
#12900=CARTESIAN_POINT('Ctrl Pts',(5.76538200189739,1.75101488004341,-1.42057375546334));
#12901=CARTESIAN_POINT('Ctrl Pts',(5.80601436392908,1.920793517681,-1.18093025336458));
#12902=CARTESIAN_POINT('Ctrl Pts',(5.82622104687486,1.99372061410875,-1.05314825661555));
#12903=CARTESIAN_POINT('Ctrl Pts',(5.86696784939671,2.11386037262269,-0.784725166469402));
#12904=CARTESIAN_POINT('Ctrl Pts',(5.8874149002506,2.16068733645426,-0.644690781704316));
#12905=CARTESIAN_POINT('Ctrl Pts',(5.94906233647854,2.25941540231167,-0.212518566495218));
#12906=CARTESIAN_POINT('Ctrl Pts',(5.98939655581076,2.26774916672706,0.0862507441290902));
#12907=CARTESIAN_POINT('Ctrl Pts',(6.05090464780758,2.19334764755515,0.52275335085135));
#12908=CARTESIAN_POINT('Ctrl Pts',(6.07132177608726,2.15458413299376,0.66469081131897));
#12909=CARTESIAN_POINT('Ctrl Pts',(6.11192401182039,2.05019102651987,0.938389433970038));
#12910=CARTESIAN_POINT('Ctrl Pts',(6.13203297821732,1.98492831099768,1.06954157773761));
#12911=CARTESIAN_POINT('Ctrl Pts',(6.19304134318137,1.75109161637569,1.44327040719888));
#12912=CARTESIAN_POINT('Ctrl Pts',(6.23381080480159,1.54720227886157,1.6599759870873));
#12913=CARTESIAN_POINT('Ctrl Pts',(6.29059691656243,1.21282720819533,1.89869343989598));
#12914=CARTESIAN_POINT('Ctrl Pts',(6.30661199780199,1.11323007755143,1.958750721318));
#12915=CARTESIAN_POINT('Ctrl Pts',(6.34688875432011,0.853380541848131,2.08919502043973));
#12916=CARTESIAN_POINT('Ctrl Pts',(6.37113166383439,0.688728795534948,2.14910266292007));
#12917=CARTESIAN_POINT('Ctrl Pts',(6.4196784236978,0.348821980273698,2.22965154308787));
#12918=CARTESIAN_POINT('Ctrl Pts',(6.44369758253354,0.174704179448234,2.25000115879057));
#12919=CARTESIAN_POINT('Ctrl Pts',(6.46787355864607,-1.49233260668402E-5,
2.24999999995051));
#12920=CARTESIAN_POINT('Ctrl Pts',(6.46784713536575,-1.86563614583413E-5,
2.24999999992265));
#12921=CARTESIAN_POINT('Ctrl Pts',(6.49211169406068,-0.174744534622054,
2.24999855114526));
#12922=CARTESIAN_POINT('Ctrl Pts',(6.51640089120071,-0.34888303436543,2.22964444352667));
#12923=CARTESIAN_POINT('Ctrl Pts',(6.56476837632269,-0.688887635955652,
2.14905765169502));
#12924=CARTESIAN_POINT('Ctrl Pts',(6.5887783135975,-0.853592650180886,2.08911305388841));
#12925=CARTESIAN_POINT('Ctrl Pts',(6.62910801303975,-1.11351736209021,1.9585901699099));
#12926=CARTESIAN_POINT('Ctrl Pts',(6.64524247698548,-1.21313997953028,1.89849573053106));
#12927=CARTESIAN_POINT('Ctrl Pts',(6.70239823256866,-1.54751144648411,1.65969019718443));
#12928=CARTESIAN_POINT('Ctrl Pts',(6.74258770509127,-1.7513776231923,1.44292970044513));
#12929=CARTESIAN_POINT('Ctrl Pts',(6.80379082558073,-1.98515165987259,1.06912675228319));
#12930=CARTESIAN_POINT('Ctrl Pts',(6.8241135176427,-2.05038733316381,0.937960852125335));
#12931=CARTESIAN_POINT('Ctrl Pts',(6.86476495051354,-2.15471745928448,0.664254512043225));
#12932=CARTESIAN_POINT('Ctrl Pts',(6.88495985747066,-2.19345058340818,0.522320281225319));
#12933=CARTESIAN_POINT('Ctrl Pts',(6.946198939737,-2.267760737065,0.0858375831489372));
#12934=CARTESIAN_POINT('Ctrl Pts',(6.98715144780304,-2.25937613503204,-0.212901376086072));
#12935=CARTESIAN_POINT('Ctrl Pts',(7.04845236832096,-2.16058234907065,-0.645045190820419));
#12936=CARTESIAN_POINT('Ctrl Pts',(7.06874014121938,-2.11373063311318,-0.785073539238702));
#12937=CARTESIAN_POINT('Ctrl Pts',(7.1095114842508,-1.99354283688225,-1.05348701234965));
#12938=CARTESIAN_POINT('Ctrl Pts',(7.12990040297153,-1.92058729590811,-1.18126617250044));
#12939=CARTESIAN_POINT('Ctrl Pts',(7.17072340625096,-1.75078172705965,-1.42085786500112));
#12940=CARTESIAN_POINT('Ctrl Pts',(7.19097291479663,-1.65431774828579,-1.53209351119021));
#12941=CARTESIAN_POINT('Ctrl Pts',(7.2517815103747,-1.33498987523482,-1.83471529856348));
#12942=CARTESIAN_POINT('Ctrl Pts',(7.29228785139571,-1.08493979810649,-1.99280583005406));
#12943=CARTESIAN_POINT('Ctrl Pts',(7.35323176978037,-0.674565692077119,
-2.1515249064064));
#12944=CARTESIAN_POINT('Ctrl Pts',(7.37345400866882,-0.532631214890633,
-2.19098221227881));
#12945=CARTESIAN_POINT('Ctrl Pts',(7.4118042875143,-0.259755662775317,-2.23873662484747));
#12946=CARTESIAN_POINT('Ctrl Pts',(7.42982873863646,-0.12998020594816,-2.25000000277498));
#12947=CARTESIAN_POINT('Ctrl Pts',(7.44790748751171,4.80358836735251E-8,
-2.25));
#12948=CARTESIAN_POINT('Origin',(-1.62,0.,0.));
#12949=CARTESIAN_POINT('',(10.1921554549285,-1.75510464272513E-10,-2.24999999965197));
#12950=CARTESIAN_POINT('',(9.40799129157889,6.73348500120871E-9,-2.25));
#12951=CARTESIAN_POINT('',(-1.62,2.75545529808154E-16,-2.25));
#12952=CARTESIAN_POINT('Ctrl Pts',(10.1921554554485,-2.47752686421965E-10,
-2.25));
#12953=CARTESIAN_POINT('Ctrl Pts',(10.1678791899995,-0.174810220022603,
-2.24999999998075));
#12954=CARTESIAN_POINT('Ctrl Pts',(10.1435797764755,-0.34902221205559,-2.22962921949452));
#12955=CARTESIAN_POINT('Ctrl Pts',(10.095204122033,-0.689077681658914,-2.14899483794996));
#12956=CARTESIAN_POINT('Ctrl Pts',(10.0711972764174,-0.853755667884177,
-2.08904449831867));
#12957=CARTESIAN_POINT('Ctrl Pts',(10.0308729101271,-1.1136365201982,-1.95852147570092));
#12958=CARTESIAN_POINT('Ctrl Pts',(10.0147406223479,-1.2132419895112,-1.89842956834442));
#12959=CARTESIAN_POINT('Ctrl Pts',(9.95758689262062,-1.54759049910711,-1.65961674556115));
#12960=CARTESIAN_POINT('Ctrl Pts',(9.91739730356014,-1.75144732661182,-1.44284539106328));
#12961=CARTESIAN_POINT('Ctrl Pts',(9.85619398933669,-1.98520348866504,-1.06903041048806));
#12962=CARTESIAN_POINT('Ctrl Pts',(9.8358713790699,-2.05043249207215,-0.937862015186465));
#12963=CARTESIAN_POINT('Ctrl Pts',(9.7952201380992,-2.15474929967526,-0.664151245701674));
#12964=CARTESIAN_POINT('Ctrl Pts',(9.77502523258085,-2.19347565022966,-0.522215036382986));
#12965=CARTESIAN_POINT('Ctrl Pts',(9.71378588818094,-2.26776507549231,-0.0857273735488627));
#12966=CARTESIAN_POINT('Ctrl Pts',(9.67283320177061,-2.25936583118408,0.213012518120693));
#12967=CARTESIAN_POINT('Ctrl Pts',(9.6115321201354,-2.16055016212059,0.645153081928275));
#12968=CARTESIAN_POINT('Ctrl Pts',(9.59124426332106,-2.11369131603536,0.785179461201588));
#12969=CARTESIAN_POINT('Ctrl Pts',(9.55047290627762,-1.99349018446163,1.05358653325004));
#12970=CARTESIAN_POINT('Ctrl Pts',(9.53008405908172,-1.92052867295727,1.1813613845873));
#12971=CARTESIAN_POINT('Ctrl Pts',(9.48926126915408,-1.75071196702641,1.42094378060002));
#12972=CARTESIAN_POINT('Ctrl Pts',(9.46901188280145,-1.65424278622536,1.53217441317964));
#12973=CARTESIAN_POINT('Ctrl Pts',(9.4082024071065,-1.33489569641816,1.83478486492308));
#12974=CARTESIAN_POINT('Ctrl Pts',(9.36769505770934,-1.08483155590647,1.99286572080852));
#12975=CARTESIAN_POINT('Ctrl Pts',(9.30675034762537,-0.674441843775681,
2.15156376045152));
#12976=CARTESIAN_POINT('Ctrl Pts',(9.28652803966901,-0.532504701513786,
2.19101299057692));
#12977=CARTESIAN_POINT('Ctrl Pts',(9.24577859847646,-0.242555833700009,
2.24173799978252));
#12978=CARTESIAN_POINT('Ctrl Pts',(9.22534478964992,-0.0952368412224312,
2.25280901643769));
#12979=CARTESIAN_POINT('Ctrl Pts',(9.16388168375656,0.346512072377135,2.24257817668726));
#12980=CARTESIAN_POINT('Ctrl Pts',(9.12370981787615,0.636751562346658,2.17802255503517));
#12981=CARTESIAN_POINT('Ctrl Pts',(9.06253692001376,1.04018689981432,2.00047628757521));
#12982=CARTESIAN_POINT('Ctrl Pts',(9.04220047461225,1.16799944579107,1.92864475338737));
#12983=CARTESIAN_POINT('Ctrl Pts',(9.00151599147505,1.40826799044789,1.76091434507733));
#12984=CARTESIAN_POINT('Ctrl Pts',(8.98131820618637,1.52010023448917,1.66533364131775));
#12985=CARTESIAN_POINT('Ctrl Pts',(8.92012969082443,1.82679201010891,1.34639257552805));
#12986=CARTESIAN_POINT('Ctrl Pts',(8.87921761889866,1.98773701141072,1.09491684581422));
#12987=CARTESIAN_POINT('Ctrl Pts',(8.81795113408565,2.14907186905657,0.682399770891608));
#12988=CARTESIAN_POINT('Ctrl Pts',(8.79767747867094,2.18911090908818,0.540343841329279));
#12989=CARTESIAN_POINT('Ctrl Pts',(8.7569088565767,2.24080424176858,0.250764149690147));
#12990=CARTESIAN_POINT('Ctrl Pts',(8.73650826454768,2.25239375654172,0.103950537859746));
#12991=CARTESIAN_POINT('Ctrl Pts',(8.6956490127593,2.24678613485836,-0.189859246691785));
#12992=CARTESIAN_POINT('Ctrl Pts',(8.67537704616007,2.22959509548118,-0.33616143559126));
#12993=CARTESIAN_POINT('Ctrl Pts',(8.61473755750295,2.13604416922574,-0.764823027594284));
#12994=CARTESIAN_POINT('Ctrl Pts',(8.57442654317558,2.01896537293113,-1.03508735577817));
#12995=CARTESIAN_POINT('Ctrl Pts',(8.51363594566775,1.77030394547916,-1.39646058182148));
#12996=CARTESIAN_POINT('Ctrl Pts',(8.49342486634409,1.67538186709516,-1.50903122743432));
#12997=CARTESIAN_POINT('Ctrl Pts',(8.45268269369654,1.46453027254645,-1.71446874901185));
#12998=CARTESIAN_POINT('Ctrl Pts',(8.43224469130559,1.34903583430484,-1.80675124475737));
#12999=CARTESIAN_POINT('Ctrl Pts',(8.37080918781604,0.978609634814664,-2.04728501279938));
#13000=CARTESIAN_POINT('Ctrl Pts',(8.33065545347321,0.70281436392203,-2.15757114052607));
#13001=CARTESIAN_POINT('Ctrl Pts',(8.27058336091969,0.277203037255173,-2.23716731953718));
#13002=CARTESIAN_POINT('Ctrl Pts',(8.25129743618393,0.13873984998652,-2.25000000067555));
#13003=CARTESIAN_POINT('Ctrl Pts',(8.23201775036189,-1.0955660406653E-8,
-2.25));
#13004=CARTESIAN_POINT('Ctrl Pts',(7.44790748751171,4.80358838146612E-8,
-2.25));
#13005=CARTESIAN_POINT('Ctrl Pts',(7.45031648143266,0.0173199214325949,
-2.24999999963023));
#13006=CARTESIAN_POINT('Ctrl Pts',(7.45272621823156,0.0346434618927655,
-2.24980001423445));
#13007=CARTESIAN_POINT('Ctrl Pts',(7.49610020567124,0.346382258987719,-2.24259800182962));
#13008=CARTESIAN_POINT('Ctrl Pts',(7.53627195156904,0.636623768696126,-2.17805967758632));
#13009=CARTESIAN_POINT('Ctrl Pts',(7.59744462210005,1.04006892373761,-2.00053769562103));
#13010=CARTESIAN_POINT('Ctrl Pts',(7.61778116825911,1.16788650756399,-1.92871321508005));
#13011=CARTESIAN_POINT('Ctrl Pts',(7.65846589394708,1.40816555054601,-1.7609962636005));
#13012=CARTESIAN_POINT('Ctrl Pts',(7.67866371491907,1.52000334029545,-1.6654220791355));
#13013=CARTESIAN_POINT('Ctrl Pts',(7.73985181636063,1.82671196060705,-1.34650064035097));
#13014=CARTESIAN_POINT('Ctrl Pts',(7.78076352791346,1.98767063308841,-1.09503667312279));
#13015=CARTESIAN_POINT('Ctrl Pts',(7.84202971159407,2.1490297547269,-0.682532279891398));
#13016=CARTESIAN_POINT('Ctrl Pts',(7.86230326647522,2.18907743671087,-0.540479298917099));
#13017=CARTESIAN_POINT('Ctrl Pts',(7.90307186576371,2.2407888284488,-0.250902384702513));
#13018=CARTESIAN_POINT('Ctrl Pts',(7.9234725375215,2.25238744205827,-0.104088562540999));
#13019=CARTESIAN_POINT('Ctrl Pts',(7.96433204816676,2.24679767729886,0.189723036676631));
#13020=CARTESIAN_POINT('Ctrl Pts',(7.98460418730738,2.2296154234309,0.336026829898549));
#13021=CARTESIAN_POINT('Ctrl Pts',(8.04524231046848,2.13609233716781,0.764684572234052));
#13022=CARTESIAN_POINT('Ctrl Pts',(8.08555173910438,2.01903581037218,1.03494704876394));
#13023=CARTESIAN_POINT('Ctrl Pts',(8.14634109124253,1.77040713033635,1.39632971307185));
#13024=CARTESIAN_POINT('Ctrl Pts',(8.1665520950889,1.67549369138675,1.50890702160853));
#13025=CARTESIAN_POINT('Ctrl Pts',(8.20729421227161,1.46465721787459,1.71436035966986));
#13026=CARTESIAN_POINT('Ctrl Pts',(8.22773223624926,1.34916907133738,1.80665180832173));
#13027=CARTESIAN_POINT('Ctrl Pts',(8.2891675313845,0.978761724240049,2.04721200714371));
#13028=CARTESIAN_POINT('Ctrl Pts',(8.32932115704057,0.702976682237688,2.1575179774717));
#13029=CARTESIAN_POINT('Ctrl Pts',(8.39045522386414,0.269846343520668,2.23855448139628));
#13030=CARTESIAN_POINT('Ctrl Pts',(8.41080931861443,0.123624641426579,2.25136818007742));
#13031=CARTESIAN_POINT('Ctrl Pts',(8.45153730418538,-0.169559396633769,
2.24839738195556));
#13032=CARTESIAN_POINT('Ctrl Pts',(8.47174488559542,-0.315827288333582,
2.2325540203774));
#13033=CARTESIAN_POINT('Ctrl Pts',(8.53284763191817,-0.748451709252293,
2.14229759214995));
#13034=CARTESIAN_POINT('Ctrl Pts',(8.57367792823207,-1.02272061053316,2.02574893780776));
#13035=CARTESIAN_POINT('Ctrl Pts',(8.6348777298969,-1.38827882269214,1.77674851017548));
#13036=CARTESIAN_POINT('Ctrl Pts',(8.65513392693521,-1.50147570510363,1.68217815750605));
#13037=CARTESIAN_POINT('Ctrl Pts',(8.69589786344588,-1.7077296333102,1.47234258268137));
#13038=CARTESIAN_POINT('Ctrl Pts',(8.71631158024835,-1.80029615758694,1.35759476745783));
#13039=CARTESIAN_POINT('Ctrl Pts',(8.75721614760918,-1.96169440977718,1.11170209019017));
#13040=CARTESIAN_POINT('Ctrl Pts',(8.77752092322055,-2.03014718659409,0.981138929748954));
#13041=CARTESIAN_POINT('Ctrl Pts',(8.83787729354608,-2.1941278449513,0.576368034708614));
#13042=CARTESIAN_POINT('Ctrl Pts',(8.87785851684834,-2.25002540127477,0.289423038532547));
#13043=CARTESIAN_POINT('Ctrl Pts',(8.95819769845474,-2.24997458026347,-0.28982835325914));
#13044=CARTESIAN_POINT('Ctrl Pts',(8.99774051748962,-2.19402582019354,-0.576744396851616));
#13045=CARTESIAN_POINT('Ctrl Pts',(9.05847639803951,-2.0299880375715,-0.981468421122089));
#13046=CARTESIAN_POINT('Ctrl Pts',(9.07887949691193,-1.96150610301751,-1.11203900272667));
#13047=CARTESIAN_POINT('Ctrl Pts',(9.11955481998493,-1.80004480754295,-1.35792754524089));
#13048=CARTESIAN_POINT('Ctrl Pts',(9.13981131485071,-1.7074654810793,-1.47264669790595));
#13049=CARTESIAN_POINT('Ctrl Pts',(9.18060290038066,-1.50118768514118,-1.68243568893175));
#13050=CARTESIAN_POINT('Ctrl Pts',(9.20104407724762,-1.38797303087011,-1.77698696975314));
#13051=CARTESIAN_POINT('Ctrl Pts',(9.26252700148927,-1.022361801345,-2.02593270437716));
#13052=CARTESIAN_POINT('Ctrl Pts',(9.30274277999797,-0.748056668585006,
-2.14243757513772));
#13053=CARTESIAN_POINT('Ctrl Pts',(9.36416357607854,-0.315398432957757,
-2.23261480086537));
#13054=CARTESIAN_POINT('Ctrl Pts',(9.38457367646151,-0.169112221404442,
-2.24843267511704));
#13055=CARTESIAN_POINT('Ctrl Pts',(9.40593108173522,-0.0148830980846057,
-2.2499630862436));
#13056=CARTESIAN_POINT('Ctrl Pts',(9.4069613454312,-0.00744114014909166,
-2.25000000004454));
#13057=CARTESIAN_POINT('Ctrl Pts',(9.40799129157889,1.34669676642552E-8,
-2.25));
#13058=CARTESIAN_POINT('Origin',(0.,0.,-1.75));
#13059=CARTESIAN_POINT('',(0.734986525864679,1.12279801474381E-10,-3.12449703104719));
#13060=CARTESIAN_POINT('Ctrl Pts',(0.734986525570974,8.83388398624539E-17,
-3.12449703116234));
#13061=CARTESIAN_POINT('Ctrl Pts',(0.677869456040291,-1.78307850476143E-14,
-2.97881367266937));
#13062=CARTESIAN_POINT('Ctrl Pts',(0.620752386509192,-4.29751012965632E-12,
-2.83313031417656));
#13063=CARTESIAN_POINT('Ctrl Pts',(0.5064663800335,-4.29751012965632E-12,
-2.54163130365447));
#13064=CARTESIAN_POINT('Ctrl Pts',(0.449297443089002,-3.51393138104219E-15,
-2.39581565162515));
#13065=CARTESIAN_POINT('Ctrl Pts',(0.392128506144054,-1.42854491361204E-16,
-2.24999999959601));
#13066=CARTESIAN_POINT('',(0.98,1.07231970108979E-7,-3.12449703081926));
#13067=CARTESIAN_POINT('Ctrl Pts',(0.98,1.38777878078145E-16,-3.12449703075067));
#13068=CARTESIAN_POINT('Ctrl Pts',(0.939166666666667,1.38777878078145E-16,
-3.12449703075067));
#13069=CARTESIAN_POINT('Ctrl Pts',(0.898333333333334,1.38777878078145E-16,
-3.12449703075067));
#13070=CARTESIAN_POINT('Ctrl Pts',(0.816662175288226,1.38777878078145E-16,
-3.12449703075067));
#13071=CARTESIAN_POINT('Ctrl Pts',(0.775824350576453,1.38777878078145E-16,
-3.12449703075067));
#13072=CARTESIAN_POINT('Ctrl Pts',(0.734986525864679,1.38777878078145E-16,
-3.12449703075067));
#13073=CARTESIAN_POINT('',(1.22498652499198,-1.0227729590452E-10,-3.1244970310227));
#13074=CARTESIAN_POINT('Ctrl Pts',(1.22498652499198,-1.38762734240172E-16,
-3.12449703075067));
#13075=CARTESIAN_POINT('Ctrl Pts',(1.18415768332799,-1.36412213158615E-16,
-3.12449703075067));
#13076=CARTESIAN_POINT('Ctrl Pts',(1.14332884166399,1.38777878078145E-16,
-3.12449703075067));
#13077=CARTESIAN_POINT('Ctrl Pts',(1.06166666666667,1.38777878078145E-16,
-3.12449703075067));
#13078=CARTESIAN_POINT('Ctrl Pts',(1.02083333333333,1.38777878078145E-16,
-3.12449703075067));
#13079=CARTESIAN_POINT('Ctrl Pts',(0.98,1.38777878078145E-16,-3.12449703075067));
#13080=CARTESIAN_POINT('Ctrl Pts',(1.56784454470915,-9.35700253971563E-17,
-2.24999999950992));
#13081=CARTESIAN_POINT('Ctrl Pts',(1.51067680443466,5.09067919699466E-15,
-2.39581259929919));
#13082=CARTESIAN_POINT('Ctrl Pts',(1.45350906416085,5.51601214575205E-12,
-2.54162519908873));
#13083=CARTESIAN_POINT('Ctrl Pts',(1.33922305767831,5.51601214575205E-12,
-2.83312420962822));
#13084=CARTESIAN_POINT('Ctrl Pts',(1.2821047914697,2.2886891001175E-14,
-2.97881062037821));
#13085=CARTESIAN_POINT('Ctrl Pts',(1.22498652526162,1.11438500184582E-16,
-3.12449703112841));
#13086=CARTESIAN_POINT('Origin',(-1.62,0.,0.));
#13087=CARTESIAN_POINT('',(11.3678714941529,1.44267579994225E-10,-2.24999999971305));
#13088=CARTESIAN_POINT('Ctrl Pts',(9.40799129157889,1.34669670553977E-8,
-2.25));
#13089=CARTESIAN_POINT('Ctrl Pts',(9.42722393706556,0.138952006083732,-2.24999999916833));
#13090=CARTESIAN_POINT('Ctrl Pts',(9.44635724963363,0.277621957227089,-2.23712827275445));
#13091=CARTESIAN_POINT('Ctrl Pts',(9.50633290109874,0.703386470993788,-2.15738069016551));
#13092=CARTESIAN_POINT('Ctrl Pts',(9.54701090703894,0.979135514210064,-2.04703274565594));
#13093=CARTESIAN_POINT('Ctrl Pts',(9.60805151839805,1.34949355615953,-1.80640917823359));
#13094=CARTESIAN_POINT('Ctrl Pts',(9.62838798253185,1.46495134723679,-1.71410654406964));
#13095=CARTESIAN_POINT('Ctrl Pts',(9.66924695654409,1.67573773164555,-1.50863645153028));
#13096=CARTESIAN_POINT('Ctrl Pts',(9.68967432809396,1.7706379741301,-1.39603778183696));
#13097=CARTESIAN_POINT('Ctrl Pts',(9.75056224243817,2.0192104430276,-1.03460645757018));
#13098=CARTESIAN_POINT('Ctrl Pts',(9.79035708141066,2.13621182393407,-0.764341340201784));
#13099=CARTESIAN_POINT('Ctrl Pts',(9.85136454776663,2.22966594882906,-0.335692092866465));
#13100=CARTESIAN_POINT('Ctrl Pts',(9.87176839065577,2.2468299138393,-0.189366695491866));
#13101=CARTESIAN_POINT('Ctrl Pts',(9.91241809383145,2.25236927240188,0.104474480257507));
#13102=CARTESIAN_POINT('Ctrl Pts',(9.93264682154377,2.24074601056064,0.251273266333001));
#13103=CARTESIAN_POINT('Ctrl Pts',(9.97341375475298,2.1889915116435,0.540828745288069));
#13104=CARTESIAN_POINT('Ctrl Pts',(9.99385851491314,2.14892040621718,0.682874580613988));
#13105=CARTESIAN_POINT('Ctrl Pts',(10.0554470055626,1.98749210778212,1.09536678146656));
#13106=CARTESIAN_POINT('Ctrl Pts',(10.0957382363584,1.82647768514058,1.34682391057384));
#13107=CARTESIAN_POINT('Ctrl Pts',(10.1572186460484,1.51969012003666,1.66570814817095));
#13108=CARTESIAN_POINT('Ctrl Pts',(10.1776323800607,1.40782476558684,1.7612704727696));
#13109=CARTESIAN_POINT('Ctrl Pts',(10.2182308009482,1.16749670769175,1.92894897553718));
#13110=CARTESIAN_POINT('Ctrl Pts',(10.2383563750675,1.03966827773101,2.00074577480369));
#13111=CARTESIAN_POINT('Ctrl Pts',(10.2993619682263,0.636216616771537,2.17817468325712));
#13112=CARTESIAN_POINT('Ctrl Pts',(10.3400934024976,0.34598484018812,2.24265810772764));
#13113=CARTESIAN_POINT('Ctrl Pts',(10.4011657134897,-0.0957520143723365,
2.25278696900762));
#13114=CARTESIAN_POINT('Ctrl Pts',(10.4214805305554,-0.243052612565244,
2.24168242290984));
#13115=CARTESIAN_POINT('Ctrl Pts',(10.4623217669302,-0.532969117421723,
2.19090039354356));
#13116=CARTESIAN_POINT('Ctrl Pts',(10.4827533498151,-0.674903277826521,
2.15141929658051));
#13117=CARTESIAN_POINT('Ctrl Pts',(10.5438595837323,-1.08526310221882,1.99263093318505));
#13118=CARTESIAN_POINT('Ctrl Pts',(10.5838092789636,-1.33528138597463,1.83450143603576));
#13119=CARTESIAN_POINT('Ctrl Pts',(10.6449772971943,-1.65455587022264,1.53183651256687));
#13120=CARTESIAN_POINT('Ctrl Pts',(10.6653821888002,-1.75101573134227,1.42057270662821));
#13121=CARTESIAN_POINT('Ctrl Pts',(10.7060145519656,-1.92079423307653,1.18092909093811));
#13122=CARTESIAN_POINT('Ctrl Pts',(10.7262212364816,-1.99372125655518,1.05314704169378));
#13123=CARTESIAN_POINT('Ctrl Pts',(10.7669680404543,-2.11386085222904,0.784723873637474));
#13124=CARTESIAN_POINT('Ctrl Pts',(10.7874150911621,-2.16068772907889,0.644689464755181));
#13125=CARTESIAN_POINT('Ctrl Pts',(10.8490625238631,-2.25941552779656,0.212517209869512));
#13126=CARTESIAN_POINT('Ctrl Pts',(10.8893967405326,-2.26774911344673,-0.0862520889962616));
#13127=CARTESIAN_POINT('Ctrl Pts',(10.9509048310764,-2.19334734149575,-0.522754634588145));
#13128=CARTESIAN_POINT('Ctrl Pts',(10.9713219591151,-2.1545837442751,-0.664692071066582));
#13129=CARTESIAN_POINT('Ctrl Pts',(11.01192419454,-2.05019047522867,-0.938390639800923));
#13130=CARTESIAN_POINT('Ctrl Pts',(11.032033162198,-1.98492767839981,-1.06954275294056));
#13131=CARTESIAN_POINT('Ctrl Pts',(11.093041526889,-1.75109076592916,-1.44327143540629));
#13132=CARTESIAN_POINT('Ctrl Pts',(11.1338109856041,-1.54720131430671,-1.65997688298466));
#13133=CARTESIAN_POINT('Ctrl Pts',(11.190594802108,-1.21283961938079,-1.89868449761896));
#13134=CARTESIAN_POINT('Ctrl Pts',(11.2066076031856,-1.11325738277325,-1.95873421942164));
#13135=CARTESIAN_POINT('Ctrl Pts',(11.2468785862839,-0.853447715989413,
-2.08916550010555));
#13136=CARTESIAN_POINT('Ctrl Pts',(11.2711180082559,-0.688821878776564,
-2.14907080760077));
#13137=CARTESIAN_POINT('Ctrl Pts',(11.3196668465811,-0.348905567752826,
-2.22964153417314));
#13138=CARTESIAN_POINT('Ctrl Pts',(11.3436900377268,-0.174758732835044,
-2.25000000001581));
#13139=CARTESIAN_POINT('Ctrl Pts',(11.3678714937241,2.03596479952939E-10,
-2.25));
#13140=CARTESIAN_POINT('',(32.48,0.,-2.25));
#13141=CARTESIAN_POINT('',(-1.62,2.75545529808154E-16,-2.25));
#13142=CARTESIAN_POINT('Origin',(32.48,0.,0.));
#13143=CARTESIAN_POINT('',(10.192,0.,-2.25));
#13144=CARTESIAN_POINT('Ctrl Pts',(1.486050567538,-0.6826354359695,-2.100935843176));
#13145=CARTESIAN_POINT('Ctrl Pts',(1.539133900872,-0.3251200195628,-2.217099643673));
#13146=CARTESIAN_POINT('Ctrl Pts',(1.645300567538,0.4500302339061,-2.2627584625));
#13147=CARTESIAN_POINT('Ctrl Pts',(1.804550567538,1.498365337642,-1.754345766741));
#13148=CARTESIAN_POINT('Ctrl Pts',(1.963800567538,2.164505898152,-0.7985285881669));
#13149=CARTESIAN_POINT('Ctrl Pts',(2.123050567538,2.278706807749,0.3609111019353));
#13150=CARTESIAN_POINT('Ctrl Pts',(2.282300567538,1.811812146172,1.428317898065));
#13151=CARTESIAN_POINT('Ctrl Pts',(2.441550567538,0.8828928310149,2.13149160242));
#13152=CARTESIAN_POINT('Ctrl Pts',(2.600800567538,-0.271171719174,2.291118092888));
#13153=CARTESIAN_POINT('Ctrl Pts',(2.760050567538,-1.35608517812,1.866491128517));
#13154=CARTESIAN_POINT('Ctrl Pts',(2.919300567538,-2.09518612394,0.9658940328033));
#13155=CARTESIAN_POINT('Ctrl Pts',(3.078550567538,-2.299997866445,-0.1810137579678));
#13156=CARTESIAN_POINT('Ctrl Pts',(3.237800567538,-1.918291788201,-1.281761594049));
#13157=CARTESIAN_POINT('Ctrl Pts',(3.397050567538,-1.047405984058,-2.055649987917));
#13158=CARTESIAN_POINT('Ctrl Pts',(3.556300567538,0.09057671026141,-2.305331218682));
#13159=CARTESIAN_POINT('Ctrl Pts',(3.715550567538,1.205461620183,-1.967134578661));
#13160=CARTESIAN_POINT('Ctrl Pts',(3.874800567538,2.012944190303,-1.127302911826));
#13161=CARTESIAN_POINT('Ctrl Pts',(4.034050567538,2.30710991682,0.));
#13162=CARTESIAN_POINT('Ctrl Pts',(4.193300567538,2.012944190303,1.127302911826));
#13163=CARTESIAN_POINT('Ctrl Pts',(4.352550567538,1.205461620183,1.967134578661));
#13164=CARTESIAN_POINT('Ctrl Pts',(4.511800567538,0.09057671026142,2.305331218682));
#13165=CARTESIAN_POINT('Ctrl Pts',(4.671050567538,-1.047405984058,2.055649987917));
#13166=CARTESIAN_POINT('Ctrl Pts',(4.830300567538,-1.918291788201,1.281761594049));
#13167=CARTESIAN_POINT('Ctrl Pts',(4.989550567538,-2.299997866445,0.1810137579678));
#13168=CARTESIAN_POINT('Ctrl Pts',(5.148800567538,-2.09518612394,-0.9658940328033));
#13169=CARTESIAN_POINT('Ctrl Pts',(5.308050567538,-1.35608517812,-1.866491128517));
#13170=CARTESIAN_POINT('Ctrl Pts',(5.467300567538,-0.271171719174,-2.291118092888));
#13171=CARTESIAN_POINT('Ctrl Pts',(5.626550567538,0.8828928310149,-2.13149160242));
#13172=CARTESIAN_POINT('Ctrl Pts',(5.785800567538,1.811812146172,-1.428317898065));
#13173=CARTESIAN_POINT('Ctrl Pts',(5.945050567538,2.278706807749,-0.3609111019352));
#13174=CARTESIAN_POINT('Ctrl Pts',(6.104300567538,2.164505898152,0.7985285881669));
#13175=CARTESIAN_POINT('Ctrl Pts',(6.263550567538,1.498365337642,1.754345766741));
#13176=CARTESIAN_POINT('Ctrl Pts',(6.422800567538,0.4500302339061,2.2627584625));
#13177=CARTESIAN_POINT('Ctrl Pts',(6.528967234205,-0.3251200195628,2.217099643673));
#13178=CARTESIAN_POINT('Ctrl Pts',(6.582050567538,-0.6826354359695,2.100935843176));
#13179=CARTESIAN_POINT('Ctrl Pts',(1.361016855846,-0.7812005935783,-2.404288206087));
#13180=CARTESIAN_POINT('Ctrl Pts',(1.414100189179,-0.3720638262881,-2.537224800233));
#13181=CARTESIAN_POINT('Ctrl Pts',(1.520266855846,0.5150097216332,-2.589476257585));
#13182=CARTESIAN_POINT('Ctrl Pts',(1.679516855846,1.714713051046,-2.007654279437));
#13183=CARTESIAN_POINT('Ctrl Pts',(1.838766855846,2.477037087943,-0.9138274607431));
#13184=CARTESIAN_POINT('Ctrl Pts',(1.998016855846,2.607727371018,0.413022753002));
#13185=CARTESIAN_POINT('Ctrl Pts',(2.157266855846,2.073418181158,1.634551520464));
#13186=CARTESIAN_POINT('Ctrl Pts',(2.316516855846,1.010372985802,2.439255885761));
#13187=CARTESIAN_POINT('Ctrl Pts',(2.475766855846,-0.3103259760893,2.6219307112));
#13188=CARTESIAN_POINT('Ctrl Pts',(2.635016855846,-1.551889178717,2.135992215868));
#13189=CARTESIAN_POINT('Ctrl Pts',(2.794266855846,-2.397708289717,1.105358661447));
#13190=CARTESIAN_POINT('Ctrl Pts',(2.953516855846,-2.632092627808,-0.2071501825414));
#13191=CARTESIAN_POINT('Ctrl Pts',(3.112766855846,-2.195272329322,-1.466834074728));
#13192=CARTESIAN_POINT('Ctrl Pts',(3.272016855846,-1.198640054924,-2.3524635642));
#13193=CARTESIAN_POINT('Ctrl Pts',(3.431266855846,0.1036550054277,-2.638196058298));
#13194=CARTESIAN_POINT('Ctrl Pts',(3.590516855846,1.37951721168,-2.251167489299));
#13195=CARTESIAN_POINT('Ctrl Pts',(3.749766855846,2.303591512314,-1.290073233029));
#13196=CARTESIAN_POINT('Ctrl Pts',(3.909016855846,2.640231581167,0.));
#13197=CARTESIAN_POINT('Ctrl Pts',(4.068266855846,2.303591512314,1.290073233029));
#13198=CARTESIAN_POINT('Ctrl Pts',(4.227516855846,1.37951721168,2.251167489299));
#13199=CARTESIAN_POINT('Ctrl Pts',(4.386766855846,0.1036550054277,2.638196058298));
#13200=CARTESIAN_POINT('Ctrl Pts',(4.546016855846,-1.198640054924,2.3524635642));
#13201=CARTESIAN_POINT('Ctrl Pts',(4.705266855846,-2.195272329322,1.466834074728));
#13202=CARTESIAN_POINT('Ctrl Pts',(4.864516855846,-2.632092627808,0.2071501825414));
#13203=CARTESIAN_POINT('Ctrl Pts',(5.023766855846,-2.397708289717,-1.105358661447));
#13204=CARTESIAN_POINT('Ctrl Pts',(5.183016855846,-1.551889178717,-2.135992215868));
#13205=CARTESIAN_POINT('Ctrl Pts',(5.342266855846,-0.3103259760893,-2.6219307112));
#13206=CARTESIAN_POINT('Ctrl Pts',(5.501516855846,1.010372985802,-2.439255885761));
#13207=CARTESIAN_POINT('Ctrl Pts',(5.660766855846,2.073418181158,-1.634551520464));
#13208=CARTESIAN_POINT('Ctrl Pts',(5.820016855846,2.607727371018,-0.4130227530019));
#13209=CARTESIAN_POINT('Ctrl Pts',(5.979266855846,2.477037087943,0.913827460743));
#13210=CARTESIAN_POINT('Ctrl Pts',(6.138516855846,1.714713051046,2.007654279437));
#13211=CARTESIAN_POINT('Ctrl Pts',(6.297766855846,0.5150097216332,2.589476257585));
#13212=CARTESIAN_POINT('Ctrl Pts',(6.403933522513,-0.3720638262881,2.537224800233));
#13213=CARTESIAN_POINT('Ctrl Pts',(6.457016855846,-0.7812005935783,2.404288206087));
#13214=CARTESIAN_POINT('Ctrl Pts',(1.235983144154,-0.8797657511871,-2.707640568999));
#13215=CARTESIAN_POINT('Ctrl Pts',(1.289066477487,-0.4190076330134,-2.857349956793));
#13216=CARTESIAN_POINT('Ctrl Pts',(1.395233144154,0.5799892093603,-2.91619405267));
#13217=CARTESIAN_POINT('Ctrl Pts',(1.554483144154,1.931060764449,-2.260962792133));
#13218=CARTESIAN_POINT('Ctrl Pts',(1.713733144154,2.789568277733,-1.029126333319));
#13219=CARTESIAN_POINT('Ctrl Pts',(1.872983144154,2.936747934286,0.4651344040687));
#13220=CARTESIAN_POINT('Ctrl Pts',(2.032233144154,2.335024216144,1.840785142863));
#13221=CARTESIAN_POINT('Ctrl Pts',(2.191483144154,1.137853140589,2.747020169102));
#13222=CARTESIAN_POINT('Ctrl Pts',(2.350733144154,-0.3494802330045,2.952743329512));
#13223=CARTESIAN_POINT('Ctrl Pts',(2.509983144154,-1.747693179314,2.405493303218));
#13224=CARTESIAN_POINT('Ctrl Pts',(2.669233144154,-2.700230455495,1.244823290091));
#13225=CARTESIAN_POINT('Ctrl Pts',(2.828483144154,-2.964187389171,-0.2332866071149));
#13226=CARTESIAN_POINT('Ctrl Pts',(2.987733144154,-2.472252870444,-1.651906555408));
#13227=CARTESIAN_POINT('Ctrl Pts',(3.146983144154,-1.34987412579,-2.649277140482));
#13228=CARTESIAN_POINT('Ctrl Pts',(3.306233144154,0.1167333005941,-2.971060897913));
#13229=CARTESIAN_POINT('Ctrl Pts',(3.465483144154,1.553572803177,-2.535200399938));
#13230=CARTESIAN_POINT('Ctrl Pts',(3.624733144154,2.594238834326,-1.452843554231));
#13231=CARTESIAN_POINT('Ctrl Pts',(3.783983144154,2.973353245513,0.));
#13232=CARTESIAN_POINT('Ctrl Pts',(3.943233144154,2.594238834326,1.452843554231));
#13233=CARTESIAN_POINT('Ctrl Pts',(4.102483144154,1.553572803177,2.535200399938));
#13234=CARTESIAN_POINT('Ctrl Pts',(4.261733144154,0.1167333005941,2.971060897913));
#13235=CARTESIAN_POINT('Ctrl Pts',(4.420983144154,-1.34987412579,2.649277140482));
#13236=CARTESIAN_POINT('Ctrl Pts',(4.580233144154,-2.472252870444,1.651906555408));
#13237=CARTESIAN_POINT('Ctrl Pts',(4.739483144154,-2.964187389171,0.2332866071149));
#13238=CARTESIAN_POINT('Ctrl Pts',(4.898733144154,-2.700230455495,-1.244823290091));
#13239=CARTESIAN_POINT('Ctrl Pts',(5.057983144154,-1.747693179314,-2.405493303218));
#13240=CARTESIAN_POINT('Ctrl Pts',(5.217233144154,-0.3494802330045,-2.952743329512));
#13241=CARTESIAN_POINT('Ctrl Pts',(5.376483144154,1.137853140589,-2.747020169102));
#13242=CARTESIAN_POINT('Ctrl Pts',(5.535733144154,2.335024216144,-1.840785142863));
#13243=CARTESIAN_POINT('Ctrl Pts',(5.694983144154,2.936747934286,-0.4651344040687));
#13244=CARTESIAN_POINT('Ctrl Pts',(5.854233144154,2.789568277733,1.029126333319));
#13245=CARTESIAN_POINT('Ctrl Pts',(6.013483144154,1.931060764449,2.260962792133));
#13246=CARTESIAN_POINT('Ctrl Pts',(6.172733144154,0.5799892093604,2.91619405267));
#13247=CARTESIAN_POINT('Ctrl Pts',(6.278899810821,-0.4190076330134,2.857349956793));
#13248=CARTESIAN_POINT('Ctrl Pts',(6.331983144154,-0.8797657511871,2.707640568999));
#13249=CARTESIAN_POINT('Ctrl Pts',(1.110949432462,-0.9783309087958,-3.010992931911));
#13250=CARTESIAN_POINT('Ctrl Pts',(1.164032765795,-0.4659514397387,-3.177475113353));
#13251=CARTESIAN_POINT('Ctrl Pts',(1.270199432462,0.6449686970875,-3.242911847755));
#13252=CARTESIAN_POINT('Ctrl Pts',(1.429449432462,2.147408477853,-2.51427130483));
#13253=CARTESIAN_POINT('Ctrl Pts',(1.588699432462,3.102099467523,-1.144425205895));
#13254=CARTESIAN_POINT('Ctrl Pts',(1.747949432462,3.265768497555,0.5172460551354));
#13255=CARTESIAN_POINT('Ctrl Pts',(1.907199432462,2.59663025113,2.047018765263));
#13256=CARTESIAN_POINT('Ctrl Pts',(2.066449432462,1.265333295377,3.054784452443));
#13257=CARTESIAN_POINT('Ctrl Pts',(2.225699432462,-0.3886344899198,3.283555947824));
#13258=CARTESIAN_POINT('Ctrl Pts',(2.384949432462,-1.943497179912,2.674994390568));
#13259=CARTESIAN_POINT('Ctrl Pts',(2.544199432462,-3.002752621272,1.384287918735));
#13260=CARTESIAN_POINT('Ctrl Pts',(2.703449432462,-3.296282150534,-0.2594230316885));
#13261=CARTESIAN_POINT('Ctrl Pts',(2.862699432462,-2.749233411565,-1.836979036087));
#13262=CARTESIAN_POINT('Ctrl Pts',(3.021949432462,-1.501108196656,-2.946090716765));
#13263=CARTESIAN_POINT('Ctrl Pts',(3.181199432462,0.1298115957604,-3.303925737529));
#13264=CARTESIAN_POINT('Ctrl Pts',(3.340449432462,1.727628394674,-2.819233310576));
#13265=CARTESIAN_POINT('Ctrl Pts',(3.499699432462,2.884886156338,-1.615613875434));
#13266=CARTESIAN_POINT('Ctrl Pts',(3.658949432462,3.30647490986,0.));
#13267=CARTESIAN_POINT('Ctrl Pts',(3.818199432462,2.884886156338,1.615613875434));
#13268=CARTESIAN_POINT('Ctrl Pts',(3.977449432462,1.727628394674,2.819233310576));
#13269=CARTESIAN_POINT('Ctrl Pts',(4.136699432462,0.1298115957604,3.303925737529));
#13270=CARTESIAN_POINT('Ctrl Pts',(4.295949432462,-1.501108196656,2.946090716765));
#13271=CARTESIAN_POINT('Ctrl Pts',(4.455199432462,-2.749233411565,1.836979036087));
#13272=CARTESIAN_POINT('Ctrl Pts',(4.614449432462,-3.296282150534,0.2594230316885));
#13273=CARTESIAN_POINT('Ctrl Pts',(4.773699432462,-3.002752621272,-1.384287918735));
#13274=CARTESIAN_POINT('Ctrl Pts',(4.932949432462,-1.943497179912,-2.674994390568));
#13275=CARTESIAN_POINT('Ctrl Pts',(5.092199432462,-0.3886344899198,-3.283555947824));
#13276=CARTESIAN_POINT('Ctrl Pts',(5.251449432462,1.265333295377,-3.054784452443));
#13277=CARTESIAN_POINT('Ctrl Pts',(5.410699432462,2.59663025113,-2.047018765263));
#13278=CARTESIAN_POINT('Ctrl Pts',(5.569949432462,3.265768497555,-0.5172460551354));
#13279=CARTESIAN_POINT('Ctrl Pts',(5.729199432462,3.102099467523,1.144425205895));
#13280=CARTESIAN_POINT('Ctrl Pts',(5.888449432462,2.147408477853,2.51427130483));
#13281=CARTESIAN_POINT('Ctrl Pts',(6.047699432462,0.6449686970875,3.242911847755));
#13282=CARTESIAN_POINT('Ctrl Pts',(6.153866099128,-0.4659514397387,3.177475113353));
#13283=CARTESIAN_POINT('Ctrl Pts',(6.206949432462,-0.9783309087958,3.010992931911));
#13284=CARTESIAN_POINT('',(6.12500744527969,7.41993572688973E-7,3.12499989450239));
#13285=CARTESIAN_POINT('Ctrl Pts',(1.2249865253955,-1.42385617185603E-10,
-3.12449703075058));
#13286=CARTESIAN_POINT('Ctrl Pts',(1.2469582081062,0.220105501026209,-3.12463783133622));
#13287=CARTESIAN_POINT('Ctrl Pts',(1.26897679573541,0.440651235200038,-3.10173887397659));
#13288=CARTESIAN_POINT('Ctrl Pts',(1.31310572384028,0.872618743152088,-3.00870835952898));
#13289=CARTESIAN_POINT('Ctrl Pts',(1.33514657553483,1.08338871438441,-2.93893910181466));
#13290=CARTESIAN_POINT('Ctrl Pts',(1.38629053209713,1.55043320018979,-2.72810358228178));
#13291=CARTESIAN_POINT('Ctrl Pts',(1.42779283828223,1.92091911867349,-2.51858797774255));
#13292=CARTESIAN_POINT('Ctrl Pts',(1.5192164507904,2.54824617086084,-1.85148038354481));
#13293=CARTESIAN_POINT('Ctrl Pts',(1.55919669615488,2.76667000678541,-1.50682910689434));
#13294=CARTESIAN_POINT('Ctrl Pts',(1.64240102883077,3.06923750138773,-0.730496208269496));
#13295=CARTESIAN_POINT('Ctrl Pts',(1.68319131879263,3.13182588768285,-0.318472133625833));
#13296=CARTESIAN_POINT('Ctrl Pts',(1.77384690094005,3.11321199907849,0.589454969171755));
#13297=CARTESIAN_POINT('Ctrl Pts',(1.81566769599401,2.97612381593503,0.996047824886873));
#13298=CARTESIAN_POINT('Ctrl Pts',(1.87566680271497,2.73245626285589,1.54560310783317));
#13299=CARTESIAN_POINT('Ctrl Pts',(1.91705708412132,2.5223074836412,1.91404302998658));
#13300=CARTESIAN_POINT('Ctrl Pts',(2.00557929492136,1.87904024871205,2.52442476815786));
#13301=CARTESIAN_POINT('Ctrl Pts',(2.04549804777898,1.54078105288759,2.75166775493569));
#13302=CARTESIAN_POINT('Ctrl Pts',(2.1284307618169,0.768144592726455,3.05621103088524));
#13303=CARTESIAN_POINT('Ctrl Pts',(2.16908686746197,0.359581070464753,3.13013165576389));
#13304=CARTESIAN_POINT('Ctrl Pts',(2.26176471540898,-0.568604604223949,
3.11705696110185));
#13305=CARTESIAN_POINT('Ctrl Pts',(2.30373757339158,-0.977563840795589,
2.9820103808569));
#13306=CARTESIAN_POINT('Ctrl Pts',(2.37430055630902,-1.62585920990471,2.69999321328487));
#13307=CARTESIAN_POINT('Ctrl Pts',(2.41487067374851,-1.96613181358351,2.46385086322353));
#13308=CARTESIAN_POINT('Ctrl Pts',(2.48543046710326,-2.45553051679632,1.95376212132771));
#13309=CARTESIAN_POINT('Ctrl Pts',(2.52677217877916,-2.71875343764017,1.62181272348733));
#13310=CARTESIAN_POINT('Ctrl Pts',(2.61751008605416,-3.05336233804938,0.776946962299032));
#13311=CARTESIAN_POINT('Ctrl Pts',(2.65791907247006,-3.1286208842104,0.371271841828455));
#13312=CARTESIAN_POINT('Ctrl Pts',(2.75122878779405,-3.1195612174274,-0.563189413652714));
#13313=CARTESIAN_POINT('Ctrl Pts',(2.79352621934935,-2.9814101539477,-0.975053271184112));
#13314=CARTESIAN_POINT('Ctrl Pts',(2.86288521992931,-2.70782042248997,-1.61380337445919));
#13315=CARTESIAN_POINT('Ctrl Pts',(2.90352769034976,-2.47211612449971,-1.955325207837));
#13316=CARTESIAN_POINT('Ctrl Pts',(2.97355979919688,-1.96811675189464,-2.44349049201393));
#13317=CARTESIAN_POINT('Ctrl Pts',(3.01507806923606,-1.63734153359,-2.71166246485518));
#13318=CARTESIAN_POINT('Ctrl Pts',(3.10669238599482,-0.78471093229284,-3.05077446246927));
#13319=CARTESIAN_POINT('Ctrl Pts',(3.14681070224775,-0.382385740435305,
-3.12715191531059));
#13320=CARTESIAN_POINT('Ctrl Pts',(3.23204749336205,0.471183768083653,-3.12237996970145));
#13321=CARTESIAN_POINT('Ctrl Pts',(3.27300860642011,0.877409231626752,-3.02091407068733));
#13322=CARTESIAN_POINT('Ctrl Pts',(3.35984142912634,1.67903873524075,-2.68319768942736));
#13323=CARTESIAN_POINT('Ctrl Pts',(3.40138319477005,2.00874122018005,-2.41423377541334));
#13324=CARTESIAN_POINT('Ctrl Pts',(3.4616942874132,2.43162777346986,-1.98258700351926));
#13325=CARTESIAN_POINT('Ctrl Pts',(3.50323523064722,2.70311754303438,-1.65387788875614));
#13326=CARTESIAN_POINT('Ctrl Pts',(3.59538249933782,3.04697916736015,-0.79728039457302));
#13327=CARTESIAN_POINT('Ctrl Pts',(3.63518829630558,3.125,-0.398671791438241));
#13328=CARTESIAN_POINT('Ctrl Pts',(3.71481170369442,3.125,0.39867179143824));
#13329=CARTESIAN_POINT('Ctrl Pts',(3.75461750066256,3.04697916736015,0.797280394573017));
#13330=CARTESIAN_POINT('Ctrl Pts',(3.84676476935332,2.70311754303439,1.65387788875614));
#13331=CARTESIAN_POINT('Ctrl Pts',(3.88830571258727,2.43162777346986,1.98258700351927));
#13332=CARTESIAN_POINT('Ctrl Pts',(3.94861680523022,2.00874122018,2.4142337754134));
#13333=CARTESIAN_POINT('Ctrl Pts',(3.9901585708736,1.6790387352407,2.68319768942738));
#13334=CARTESIAN_POINT('Ctrl Pts',(4.07699139357983,0.877409231626905,3.02091407068727));
#13335=CARTESIAN_POINT('Ctrl Pts',(4.11795250663809,0.471183768083811,3.12237996970145));
#13336=CARTESIAN_POINT('Ctrl Pts',(4.20318929775232,-0.382385740435277,
3.12715191531059));
#13337=CARTESIAN_POINT('Ctrl Pts',(4.24330761400502,-0.78471093229281,3.05077446246928));
#13338=CARTESIAN_POINT('Ctrl Pts',(4.33492193076373,-1.63734153358998,2.71166246485519));
#13339=CARTESIAN_POINT('Ctrl Pts',(4.37644020080298,-1.96811675189461,2.44349049201395));
#13340=CARTESIAN_POINT('Ctrl Pts',(4.44647230965025,-2.4721161244997,1.95532520783702));
#13341=CARTESIAN_POINT('Ctrl Pts',(4.48711478007087,-2.70782042248996,1.6138033744592));
#13342=CARTESIAN_POINT('Ctrl Pts',(4.55647378065097,-2.98141015394769,0.97505327118414));
#13343=CARTESIAN_POINT('Ctrl Pts',(4.5987712122064,-3.1195612174274,0.563189413652733));
#13344=CARTESIAN_POINT('Ctrl Pts',(4.69208092753042,-3.1286208842104,-0.371271841828482));
#13345=CARTESIAN_POINT('Ctrl Pts',(4.73248991394627,-3.05336233804938,-0.776946962299062));
#13346=CARTESIAN_POINT('Ctrl Pts',(4.82322782122118,-2.71875343764019,-1.62181272348726));
#13347=CARTESIAN_POINT('Ctrl Pts',(4.864569532897,-2.45553051679639,-1.95376212132765));
#13348=CARTESIAN_POINT('Ctrl Pts',(4.93512932625151,-1.96613181358349,-2.46385086322354));
#13349=CARTESIAN_POINT('Ctrl Pts',(4.9756994436907,-1.62585920990471,-2.69999321328486));
#13350=CARTESIAN_POINT('Ctrl Pts',(5.04626242660797,-0.977563840795617,
-2.98201038085689));
#13351=CARTESIAN_POINT('Ctrl Pts',(5.08823528459042,-0.568604604223984,
-3.11705696110184));
#13352=CARTESIAN_POINT('Ctrl Pts',(5.18091313253766,0.359581070464712,-3.13013165576389));
#13353=CARTESIAN_POINT('Ctrl Pts',(5.22156923818307,0.76814459272642,-3.05621103088525));
#13354=CARTESIAN_POINT('Ctrl Pts',(5.30450195222119,1.54078105288758,-2.7516677549357));
#13355=CARTESIAN_POINT('Ctrl Pts',(5.34442070507877,1.87904024871205,-2.52442476815786));
#13356=CARTESIAN_POINT('Ctrl Pts',(5.43294291587883,2.52230748364104,-1.91404302998674));
#13357=CARTESIAN_POINT('Ctrl Pts',(5.47433319728519,2.73245626285581,-1.54560310783341));
#13358=CARTESIAN_POINT('Ctrl Pts',(5.5343323040062,2.97612381593512,-0.9960478248867));
#13359=CARTESIAN_POINT('Ctrl Pts',(5.57615309906016,3.1132119990785,-0.589454969171629));
#13360=CARTESIAN_POINT('Ctrl Pts',(5.66680868120744,3.13182588768285,0.31847213362576));
#13361=CARTESIAN_POINT('Ctrl Pts',(5.70759897116911,3.06923750138774,0.730496208269452));
#13362=CARTESIAN_POINT('Ctrl Pts',(5.79080330384514,2.7666700067854,1.50682910689435));
#13363=CARTESIAN_POINT('Ctrl Pts',(5.83078354921002,2.54824617086083,1.85148038354482));
#13364=CARTESIAN_POINT('Ctrl Pts',(5.92220716171829,1.92091911867347,2.51858797774256));
#13365=CARTESIAN_POINT('Ctrl Pts',(5.9637094679032,1.55043320018976,2.7281035822818));
#13366=CARTESIAN_POINT('Ctrl Pts',(6.01485344133236,1.08338856035466,2.93893917134752));
#13367=CARTESIAN_POINT('Ctrl Pts',(6.0368943099015,0.872618420486184,3.00870846633562));
#13368=CARTESIAN_POINT('Ctrl Pts',(6.08102337747936,0.440649532003025,3.10173920341104));
#13369=CARTESIAN_POINT('Ctrl Pts',(6.10304208760836,0.220102539161381,3.12463812164867));
#13370=CARTESIAN_POINT('Ctrl Pts',(6.12501389259301,-4.18742151370166E-6,
3.12449702806922));
#13371=CARTESIAN_POINT('',(6.468,0.,2.25));
#13372=CARTESIAN_POINT('Ctrl Pts',(6.386050567538,0.6826354359695,2.100935843176));
#13373=CARTESIAN_POINT('Ctrl Pts',(6.439133900872,0.3251200195628,2.217099643673));
#13374=CARTESIAN_POINT('Ctrl Pts',(6.545300567538,-0.4500302339061,2.2627584625));
#13375=CARTESIAN_POINT('Ctrl Pts',(6.704550567538,-1.498365337642,1.754345766741));
#13376=CARTESIAN_POINT('Ctrl Pts',(6.863800567538,-2.164505898152,0.7985285881669));
#13377=CARTESIAN_POINT('Ctrl Pts',(7.023050567538,-2.278706807749,-0.3609111019352));
#13378=CARTESIAN_POINT('Ctrl Pts',(7.182300567538,-1.811812146172,-1.428317898065));
#13379=CARTESIAN_POINT('Ctrl Pts',(7.341550567538,-0.8828928310149,-2.13149160242));
#13380=CARTESIAN_POINT('Ctrl Pts',(7.500800567538,0.271171719174,-2.291118092888));
#13381=CARTESIAN_POINT('Ctrl Pts',(7.660050567538,1.35608517812,-1.866491128517));
#13382=CARTESIAN_POINT('Ctrl Pts',(7.819300567538,2.09518612394,-0.9658940328033));
#13383=CARTESIAN_POINT('Ctrl Pts',(7.978550567538,2.299997866445,0.1810137579678));
#13384=CARTESIAN_POINT('Ctrl Pts',(8.137800567538,1.918291788201,1.281761594049));
#13385=CARTESIAN_POINT('Ctrl Pts',(8.297050567538,1.047405984058,2.055649987917));
#13386=CARTESIAN_POINT('Ctrl Pts',(8.456300567538,-0.0905767102614,2.305331218682));
#13387=CARTESIAN_POINT('Ctrl Pts',(8.615550567538,-1.205461620183,1.967134578661));
#13388=CARTESIAN_POINT('Ctrl Pts',(8.774800567538,-2.012944190303,1.127302911826));
#13389=CARTESIAN_POINT('Ctrl Pts',(8.934050567538,-2.30710991682,0.));
#13390=CARTESIAN_POINT('Ctrl Pts',(9.093300567538,-2.012944190303,-1.127302911826));
#13391=CARTESIAN_POINT('Ctrl Pts',(9.252550567538,-1.205461620183,-1.967134578661));
#13392=CARTESIAN_POINT('Ctrl Pts',(9.411800567538,-0.09057671026141,-2.305331218682));
#13393=CARTESIAN_POINT('Ctrl Pts',(9.571050567538,1.047405984058,-2.055649987917));
#13394=CARTESIAN_POINT('Ctrl Pts',(9.730300567538,1.918291788201,-1.281761594049));
#13395=CARTESIAN_POINT('Ctrl Pts',(9.889550567538,2.299997866445,-0.1810137579678));
#13396=CARTESIAN_POINT('Ctrl Pts',(10.04880056754,2.09518612394,0.9658940328033));
#13397=CARTESIAN_POINT('Ctrl Pts',(10.20805056754,1.35608517812,1.866491128517));
#13398=CARTESIAN_POINT('Ctrl Pts',(10.36730056754,0.271171719174,2.291118092888));
#13399=CARTESIAN_POINT('Ctrl Pts',(10.52655056754,-0.8828928310149,2.13149160242));
#13400=CARTESIAN_POINT('Ctrl Pts',(10.68580056754,-1.811812146172,1.428317898065));
#13401=CARTESIAN_POINT('Ctrl Pts',(10.84505056754,-2.278706807749,0.3609111019352));
#13402=CARTESIAN_POINT('Ctrl Pts',(11.00430056754,-2.164505898152,-0.7985285881669));
#13403=CARTESIAN_POINT('Ctrl Pts',(11.16355056754,-1.498365337642,-1.754345766741));
#13404=CARTESIAN_POINT('Ctrl Pts',(11.32280056754,-0.4500302339061,-2.2627584625));
#13405=CARTESIAN_POINT('Ctrl Pts',(11.4289672342,0.3251200195628,-2.217099643673));
#13406=CARTESIAN_POINT('Ctrl Pts',(11.48205056754,0.6826354359695,-2.100935843176));
#13407=CARTESIAN_POINT('Ctrl Pts',(6.261016855846,0.7812005935783,2.404288206087));
#13408=CARTESIAN_POINT('Ctrl Pts',(6.314100189179,0.3720638262881,2.537224800233));
#13409=CARTESIAN_POINT('Ctrl Pts',(6.420266855846,-0.5150097216332,2.589476257585));
#13410=CARTESIAN_POINT('Ctrl Pts',(6.579516855846,-1.714713051046,2.007654279437));
#13411=CARTESIAN_POINT('Ctrl Pts',(6.738766855846,-2.477037087943,0.9138274607431));
#13412=CARTESIAN_POINT('Ctrl Pts',(6.898016855846,-2.607727371018,-0.4130227530019));
#13413=CARTESIAN_POINT('Ctrl Pts',(7.057266855846,-2.073418181158,-1.634551520464));
#13414=CARTESIAN_POINT('Ctrl Pts',(7.216516855846,-1.010372985802,-2.439255885761));
#13415=CARTESIAN_POINT('Ctrl Pts',(7.375766855846,0.3103259760892,-2.6219307112));
#13416=CARTESIAN_POINT('Ctrl Pts',(7.535016855846,1.551889178717,-2.135992215868));
#13417=CARTESIAN_POINT('Ctrl Pts',(7.694266855846,2.397708289717,-1.105358661447));
#13418=CARTESIAN_POINT('Ctrl Pts',(7.853516855846,2.632092627808,0.2071501825414));
#13419=CARTESIAN_POINT('Ctrl Pts',(8.012766855846,2.195272329322,1.466834074728));
#13420=CARTESIAN_POINT('Ctrl Pts',(8.172016855846,1.198640054924,2.3524635642));
#13421=CARTESIAN_POINT('Ctrl Pts',(8.331266855846,-0.1036550054277,2.638196058298));
#13422=CARTESIAN_POINT('Ctrl Pts',(8.490516855846,-1.37951721168,2.251167489299));
#13423=CARTESIAN_POINT('Ctrl Pts',(8.649766855846,-2.303591512314,1.290073233029));
#13424=CARTESIAN_POINT('Ctrl Pts',(8.809016855846,-2.640231581167,1.108429745068E-14));
#13425=CARTESIAN_POINT('Ctrl Pts',(8.968266855846,-2.303591512314,-1.290073233029));
#13426=CARTESIAN_POINT('Ctrl Pts',(9.127516855846,-1.37951721168,-2.251167489299));
#13427=CARTESIAN_POINT('Ctrl Pts',(9.286766855846,-0.1036550054277,-2.638196058298));
#13428=CARTESIAN_POINT('Ctrl Pts',(9.446016855846,1.198640054924,-2.3524635642));
#13429=CARTESIAN_POINT('Ctrl Pts',(9.605266855846,2.195272329322,-1.466834074728));
#13430=CARTESIAN_POINT('Ctrl Pts',(9.764516855846,2.632092627808,-0.2071501825414));
#13431=CARTESIAN_POINT('Ctrl Pts',(9.923766855846,2.397708289717,1.105358661447));
#13432=CARTESIAN_POINT('Ctrl Pts',(10.08301685585,1.551889178717,2.135992215868));
#13433=CARTESIAN_POINT('Ctrl Pts',(10.24226685585,0.3103259760892,2.6219307112));
#13434=CARTESIAN_POINT('Ctrl Pts',(10.40151685585,-1.010372985802,2.439255885761));
#13435=CARTESIAN_POINT('Ctrl Pts',(10.56076685585,-2.073418181158,1.634551520464));
#13436=CARTESIAN_POINT('Ctrl Pts',(10.72001685585,-2.607727371018,0.4130227530019));
#13437=CARTESIAN_POINT('Ctrl Pts',(10.87926685585,-2.477037087943,-0.913827460743));
#13438=CARTESIAN_POINT('Ctrl Pts',(11.03851685585,-1.714713051046,-2.007654279437));
#13439=CARTESIAN_POINT('Ctrl Pts',(11.19776685585,-0.5150097216332,-2.589476257585));
#13440=CARTESIAN_POINT('Ctrl Pts',(11.30393352251,0.3720638262881,-2.537224800233));
#13441=CARTESIAN_POINT('Ctrl Pts',(11.35701685585,0.7812005935783,-2.404288206087));
#13442=CARTESIAN_POINT('Ctrl Pts',(6.135983144154,0.8797657511871,2.707640568999));
#13443=CARTESIAN_POINT('Ctrl Pts',(6.189066477487,0.4190076330134,2.857349956793));
#13444=CARTESIAN_POINT('Ctrl Pts',(6.295233144154,-0.5799892093603,2.91619405267));
#13445=CARTESIAN_POINT('Ctrl Pts',(6.454483144154,-1.931060764449,2.260962792133));
#13446=CARTESIAN_POINT('Ctrl Pts',(6.613733144154,-2.789568277733,1.029126333319));
#13447=CARTESIAN_POINT('Ctrl Pts',(6.772983144154,-2.936747934286,-0.4651344040686));
#13448=CARTESIAN_POINT('Ctrl Pts',(6.932233144154,-2.335024216144,-1.840785142863));
#13449=CARTESIAN_POINT('Ctrl Pts',(7.091483144154,-1.137853140589,-2.747020169102));
#13450=CARTESIAN_POINT('Ctrl Pts',(7.250733144154,0.3494802330045,-2.952743329512));
#13451=CARTESIAN_POINT('Ctrl Pts',(7.409983144154,1.747693179314,-2.405493303218));
#13452=CARTESIAN_POINT('Ctrl Pts',(7.569233144154,2.700230455495,-1.244823290091));
#13453=CARTESIAN_POINT('Ctrl Pts',(7.728483144154,2.964187389171,0.2332866071149));
#13454=CARTESIAN_POINT('Ctrl Pts',(7.887733144154,2.472252870444,1.651906555408));
#13455=CARTESIAN_POINT('Ctrl Pts',(8.046983144154,1.34987412579,2.649277140482));
#13456=CARTESIAN_POINT('Ctrl Pts',(8.206233144154,-0.116733300594,2.971060897913));
#13457=CARTESIAN_POINT('Ctrl Pts',(8.365483144154,-1.553572803177,2.535200399938));
#13458=CARTESIAN_POINT('Ctrl Pts',(8.524733144154,-2.594238834326,1.452843554231));
#13459=CARTESIAN_POINT('Ctrl Pts',(8.683983144154,-2.973353245513,1.647272319884E-14));
#13460=CARTESIAN_POINT('Ctrl Pts',(8.843233144154,-2.594238834326,-1.452843554231));
#13461=CARTESIAN_POINT('Ctrl Pts',(9.002483144154,-1.553572803177,-2.535200399938));
#13462=CARTESIAN_POINT('Ctrl Pts',(9.161733144154,-0.1167333005941,-2.971060897913));
#13463=CARTESIAN_POINT('Ctrl Pts',(9.320983144154,1.34987412579,-2.649277140482));
#13464=CARTESIAN_POINT('Ctrl Pts',(9.480233144154,2.472252870444,-1.651906555408));
#13465=CARTESIAN_POINT('Ctrl Pts',(9.639483144154,2.964187389171,-0.2332866071149));
#13466=CARTESIAN_POINT('Ctrl Pts',(9.798733144154,2.700230455495,1.244823290091));
#13467=CARTESIAN_POINT('Ctrl Pts',(9.957983144154,1.747693179314,2.405493303218));
#13468=CARTESIAN_POINT('Ctrl Pts',(10.11723314415,0.3494802330045,2.952743329512));
#13469=CARTESIAN_POINT('Ctrl Pts',(10.27648314415,-1.137853140589,2.747020169102));
#13470=CARTESIAN_POINT('Ctrl Pts',(10.43573314415,-2.335024216144,1.840785142863));
#13471=CARTESIAN_POINT('Ctrl Pts',(10.59498314415,-2.936747934286,0.4651344040687));
#13472=CARTESIAN_POINT('Ctrl Pts',(10.75423314415,-2.789568277733,-1.029126333319));
#13473=CARTESIAN_POINT('Ctrl Pts',(10.91348314415,-1.931060764449,-2.260962792133));
#13474=CARTESIAN_POINT('Ctrl Pts',(11.07273314415,-0.5799892093604,-2.91619405267));
#13475=CARTESIAN_POINT('Ctrl Pts',(11.17889981082,0.4190076330134,-2.857349956793));
#13476=CARTESIAN_POINT('Ctrl Pts',(11.23198314415,0.8797657511871,-2.707640568999));
#13477=CARTESIAN_POINT('Ctrl Pts',(6.010949432462,0.9783309087958,3.010992931911));
#13478=CARTESIAN_POINT('Ctrl Pts',(6.064032765795,0.4659514397387,3.177475113353));
#13479=CARTESIAN_POINT('Ctrl Pts',(6.170199432462,-0.6449686970874,3.242911847755));
#13480=CARTESIAN_POINT('Ctrl Pts',(6.329449432462,-2.147408477853,2.51427130483));
#13481=CARTESIAN_POINT('Ctrl Pts',(6.488699432462,-3.102099467523,1.144425205895));
#13482=CARTESIAN_POINT('Ctrl Pts',(6.647949432462,-3.265768497555,-0.5172460551353));
#13483=CARTESIAN_POINT('Ctrl Pts',(6.807199432462,-2.59663025113,-2.047018765263));
#13484=CARTESIAN_POINT('Ctrl Pts',(6.966449432462,-1.265333295377,-3.054784452443));
#13485=CARTESIAN_POINT('Ctrl Pts',(7.125699432462,0.3886344899198,-3.283555947824));
#13486=CARTESIAN_POINT('Ctrl Pts',(7.284949432462,1.943497179912,-2.674994390568));
#13487=CARTESIAN_POINT('Ctrl Pts',(7.444199432462,3.002752621272,-1.384287918735));
#13488=CARTESIAN_POINT('Ctrl Pts',(7.603449432462,3.296282150534,0.2594230316885));
#13489=CARTESIAN_POINT('Ctrl Pts',(7.762699432462,2.749233411565,1.836979036087));
#13490=CARTESIAN_POINT('Ctrl Pts',(7.921949432462,1.501108196656,2.946090716765));
#13491=CARTESIAN_POINT('Ctrl Pts',(8.081199432462,-0.1298115957604,3.303925737529));
#13492=CARTESIAN_POINT('Ctrl Pts',(8.240449432462,-1.727628394674,2.819233310576));
#13493=CARTESIAN_POINT('Ctrl Pts',(8.399699432462,-2.884886156338,1.615613875434));
#13494=CARTESIAN_POINT('Ctrl Pts',(8.558949432462,-3.30647490986,1.754152378908E-14));
#13495=CARTESIAN_POINT('Ctrl Pts',(8.718199432462,-2.884886156338,-1.615613875434));
#13496=CARTESIAN_POINT('Ctrl Pts',(8.877449432462,-1.727628394674,-2.819233310576));
#13497=CARTESIAN_POINT('Ctrl Pts',(9.036699432462,-0.1298115957604,-3.303925737529));
#13498=CARTESIAN_POINT('Ctrl Pts',(9.195949432462,1.501108196656,-2.946090716765));
#13499=CARTESIAN_POINT('Ctrl Pts',(9.355199432462,2.749233411565,-1.836979036087));
#13500=CARTESIAN_POINT('Ctrl Pts',(9.514449432462,3.296282150534,-0.2594230316885));
#13501=CARTESIAN_POINT('Ctrl Pts',(9.673699432462,3.002752621272,1.384287918735));
#13502=CARTESIAN_POINT('Ctrl Pts',(9.832949432462,1.943497179912,2.674994390568));
#13503=CARTESIAN_POINT('Ctrl Pts',(9.992199432462,0.3886344899198,3.283555947824));
#13504=CARTESIAN_POINT('Ctrl Pts',(10.15144943246,-1.265333295377,3.054784452443));
#13505=CARTESIAN_POINT('Ctrl Pts',(10.31069943246,-2.59663025113,2.047018765263));
#13506=CARTESIAN_POINT('Ctrl Pts',(10.46994943246,-3.265768497555,0.5172460551354));
#13507=CARTESIAN_POINT('Ctrl Pts',(10.62919943246,-3.102099467523,-1.144425205895));
#13508=CARTESIAN_POINT('Ctrl Pts',(10.78844943246,-2.147408477853,-2.51427130483));
#13509=CARTESIAN_POINT('Ctrl Pts',(10.94769943246,-0.6449686970875,-3.242911847755));
#13510=CARTESIAN_POINT('Ctrl Pts',(11.05386609913,0.4659514397387,-3.177475113353));
#13511=CARTESIAN_POINT('Ctrl Pts',(11.10694943246,0.9783309087959,-3.010992931911));
#13512=CARTESIAN_POINT('',(11.0250134741351,-1.1227774403895E-10,-3.12449703104719));
#13513=CARTESIAN_POINT('Ctrl Pts',(6.12498723189613,-7.07736163719358E-6,
3.12449703527009));
#13514=CARTESIAN_POINT('Ctrl Pts',(6.14695866368768,-0.220110064033207,
3.12463734035084));
#13515=CARTESIAN_POINT('Ctrl Pts',(6.16897699922435,-0.440653219467678,
3.1017384092623));
#13516=CARTESIAN_POINT('Ctrl Pts',(6.21310569009841,-0.87261842048626,3.0087084663356));
#13517=CARTESIAN_POINT('Ctrl Pts',(6.23514655866772,-1.08338856035471,2.9389391713475));
#13518=CARTESIAN_POINT('Ctrl Pts',(6.28629053209712,-1.55043320018978,2.72810358228179));
#13519=CARTESIAN_POINT('Ctrl Pts',(6.32779283828223,-1.92091911867348,2.51858797774255));
#13520=CARTESIAN_POINT('Ctrl Pts',(6.4192164507904,-2.54824617086084,1.85148038354481));
#13521=CARTESIAN_POINT('Ctrl Pts',(6.45919669615489,-2.76667000678541,1.50682910689433));
#13522=CARTESIAN_POINT('Ctrl Pts',(6.54240102883078,-3.06923750138774,0.730496208269489));
#13523=CARTESIAN_POINT('Ctrl Pts',(6.58319131879264,-3.13182588768285,0.318472133625827));
#13524=CARTESIAN_POINT('Ctrl Pts',(6.67384690094006,-3.11321199907849,-0.589454969171753));
#13525=CARTESIAN_POINT('Ctrl Pts',(6.715667695994,-2.97612381593503,-0.996047824886871));
#13526=CARTESIAN_POINT('Ctrl Pts',(6.77566680271496,-2.73245626285591,-1.54560310783311));
#13527=CARTESIAN_POINT('Ctrl Pts',(6.81705708412131,-2.52230748364124,-1.91404302998654));
#13528=CARTESIAN_POINT('Ctrl Pts',(6.90557929492136,-1.87904024871203,-2.52442476815788));
#13529=CARTESIAN_POINT('Ctrl Pts',(6.94549804777898,-1.54078105288757,-2.7516677549357));
#13530=CARTESIAN_POINT('Ctrl Pts',(7.0284307618169,-0.768144592726452,-3.05621103088524));
#13531=CARTESIAN_POINT('Ctrl Pts',(7.06908686746197,-0.359581070464751,
-3.13013165576389));
#13532=CARTESIAN_POINT('Ctrl Pts',(7.16176471540898,0.56860460422395,-3.11705696110185));
#13533=CARTESIAN_POINT('Ctrl Pts',(7.20373757339158,0.97756384079559,-2.9820103808569));
#13534=CARTESIAN_POINT('Ctrl Pts',(7.27430055630902,1.62585920990471,-2.69999321328487));
#13535=CARTESIAN_POINT('Ctrl Pts',(7.31487067374851,1.96613181358351,-2.46385086322353));
#13536=CARTESIAN_POINT('Ctrl Pts',(7.38543046710326,2.45553051679631,-1.95376212132773));
#13537=CARTESIAN_POINT('Ctrl Pts',(7.42677217877916,2.71875343764016,-1.62181272348735));
#13538=CARTESIAN_POINT('Ctrl Pts',(7.51751008605417,3.05336233804939,-0.776946962299028));
#13539=CARTESIAN_POINT('Ctrl Pts',(7.55791907247006,3.1286208842104,-0.371271841828451));
#13540=CARTESIAN_POINT('Ctrl Pts',(7.65122878779405,3.1195612174274,0.563189413652742));
#13541=CARTESIAN_POINT('Ctrl Pts',(7.69352621934936,2.98141015394768,0.975053271184142));
#13542=CARTESIAN_POINT('Ctrl Pts',(7.76288521992931,2.70782042248997,1.61380337445919));
#13543=CARTESIAN_POINT('Ctrl Pts',(7.80352769034976,2.47211612449971,1.955325207837));
#13544=CARTESIAN_POINT('Ctrl Pts',(7.87355979919688,1.96811675189463,2.44349049201393));
#13545=CARTESIAN_POINT('Ctrl Pts',(7.91507806923605,1.63734153359,2.71166246485518));
#13546=CARTESIAN_POINT('Ctrl Pts',(8.00669238599482,0.78471093229284,3.05077446246927));
#13547=CARTESIAN_POINT('Ctrl Pts',(8.04681070224775,0.382385740435304,3.12715191531059));
#13548=CARTESIAN_POINT('Ctrl Pts',(8.13204749336205,-0.471183768083647,
3.12237996970145));
#13549=CARTESIAN_POINT('Ctrl Pts',(8.17300860642011,-0.877409231626746,
3.02091407068734));
#13550=CARTESIAN_POINT('Ctrl Pts',(8.25984142912633,-1.67903873524074,2.68319768942737));
#13551=CARTESIAN_POINT('Ctrl Pts',(8.30138319477005,-2.00874122018004,2.41423377541336));
#13552=CARTESIAN_POINT('Ctrl Pts',(8.3616942874132,-2.43162777346988,1.98258700351925));
#13553=CARTESIAN_POINT('Ctrl Pts',(8.40323523064723,-2.70311754303439,1.65387788875613));
#13554=CARTESIAN_POINT('Ctrl Pts',(8.49538249933782,-3.04697916736015,0.79728039457302));
#13555=CARTESIAN_POINT('Ctrl Pts',(8.53518829630558,-3.125,0.398671791438241));
#13556=CARTESIAN_POINT('Ctrl Pts',(8.61481170369442,-3.125,-0.398671791438241));
#13557=CARTESIAN_POINT('Ctrl Pts',(8.65461750066257,-3.04697916736015,-0.797280394573019));
#13558=CARTESIAN_POINT('Ctrl Pts',(8.74676476935333,-2.70311754303436,-1.65387788875621));
#13559=CARTESIAN_POINT('Ctrl Pts',(8.78830571258729,-2.4316277734698,-1.98258700351933));
#13560=CARTESIAN_POINT('Ctrl Pts',(8.84861680523022,-2.00874122018003,-2.41423377541336));
#13561=CARTESIAN_POINT('Ctrl Pts',(8.89015857087361,-1.67903873524074,-2.68319768942736));
#13562=CARTESIAN_POINT('Ctrl Pts',(8.97699139357984,-0.877409231626881,
-3.02091407068728));
#13563=CARTESIAN_POINT('Ctrl Pts',(9.0179525066381,-0.471183768083787,-3.12237996970145));
#13564=CARTESIAN_POINT('Ctrl Pts',(9.10318929775232,0.382385740435283,-3.12715191531059));
#13565=CARTESIAN_POINT('Ctrl Pts',(9.14330761400503,0.784710932292816,-3.05077446246928));
#13566=CARTESIAN_POINT('Ctrl Pts',(9.23492193076374,1.63734153358998,-2.71166246485519));
#13567=CARTESIAN_POINT('Ctrl Pts',(9.27644020080298,1.96811675189461,-2.44349049201395));
#13568=CARTESIAN_POINT('Ctrl Pts',(9.34647230965026,2.4721161244997,-1.95532520783702));
#13569=CARTESIAN_POINT('Ctrl Pts',(9.38711478007088,2.70782042248997,-1.61380337445919));
#13570=CARTESIAN_POINT('Ctrl Pts',(9.45647378065097,2.98141015394769,-0.97505327118413));
#13571=CARTESIAN_POINT('Ctrl Pts',(9.4987712122064,3.1195612174274,-0.563189413652723));
#13572=CARTESIAN_POINT('Ctrl Pts',(9.59208092753043,3.1286208842104,0.371271841828488));
#13573=CARTESIAN_POINT('Ctrl Pts',(9.63248991394628,3.05336233804938,0.776946962299067));
#13574=CARTESIAN_POINT('Ctrl Pts',(9.72322782122119,2.71875343764021,1.62181272348721));
#13575=CARTESIAN_POINT('Ctrl Pts',(9.76456953289697,2.45553051679643,1.95376212132761));
#13576=CARTESIAN_POINT('Ctrl Pts',(9.83512932625145,1.96613181358349,2.46385086322354));
#13577=CARTESIAN_POINT('Ctrl Pts',(9.87569944369059,1.62585920990472,2.69999321328486));
#13578=CARTESIAN_POINT('Ctrl Pts',(9.94626242660763,0.977563840795634,2.98201038085688));
#13579=CARTESIAN_POINT('Ctrl Pts',(9.98823528459023,0.568604604224015,3.11705696110183));
#13580=CARTESIAN_POINT('Ctrl Pts',(10.0809131325367,-0.359581070464643,
3.1301316557639));
#13581=CARTESIAN_POINT('Ctrl Pts',(10.1215692381812,-0.768144592726318,
3.05621103088527));
#13582=CARTESIAN_POINT('Ctrl Pts',(10.2045019522189,-1.54078105288753,2.75166775493574));
#13583=CARTESIAN_POINT('Ctrl Pts',(10.2444207050765,-1.87904024871197,2.5244247681579));
#13584=CARTESIAN_POINT('Ctrl Pts',(10.3329429158766,-2.52230748364106,1.91404302998675));
#13585=CARTESIAN_POINT('Ctrl Pts',(10.3743331972831,-2.73245626285578,1.54560310783337));
#13586=CARTESIAN_POINT('Ctrl Pts',(10.4343323040041,-2.97612381593498,0.996047824887012));
#13587=CARTESIAN_POINT('Ctrl Pts',(10.476153099058,-3.11321199907846,0.589454969171896));
#13588=CARTESIAN_POINT('Ctrl Pts',(10.5668086812053,-3.13182588768287,-0.31847213362573));
#13589=CARTESIAN_POINT('Ctrl Pts',(10.607598971167,-3.06923750138775,-0.730496208269382));
#13590=CARTESIAN_POINT('Ctrl Pts',(10.690803303843,-2.76667000678551,-1.50682910689415));
#13591=CARTESIAN_POINT('Ctrl Pts',(10.7307835492079,-2.54824617086096,-1.85148038354464));
#13592=CARTESIAN_POINT('Ctrl Pts',(10.8222071617162,-1.9209191186736,-2.51858797774247));
#13593=CARTESIAN_POINT('Ctrl Pts',(10.8637094679009,-1.55043320018988,-2.72810358228172));
#13594=CARTESIAN_POINT('Ctrl Pts',(10.9148534207039,-1.08338874871494,-2.93893908631701));
#13595=CARTESIAN_POINT('Ctrl Pts',(10.9368942686374,-0.872618815068493,
-3.00870833572371));
#13596=CARTESIAN_POINT('Ctrl Pts',(10.9810231968561,-0.440651309409201,
-3.10173886632448));
#13597=CARTESIAN_POINT('Ctrl Pts',(11.0030417882076,-0.220105537948483,
-3.12463783133899));
#13598=CARTESIAN_POINT('Ctrl Pts',(11.0250134745746,-1.56339628742952E-10,
-3.12449703075077));
#13599=CARTESIAN_POINT('Ctrl Pts',(11.3678714938544,6.18854804392756E-16,
-2.24999999959601));
#13600=CARTESIAN_POINT('Ctrl Pts',(11.3107025569102,3.98751462744629E-15,
-2.39581565162524));
#13601=CARTESIAN_POINT('Ctrl Pts',(11.2535336199657,4.2949048620429E-12,
-2.54163130365436));
#13602=CARTESIAN_POINT('Ctrl Pts',(11.13924761349,4.2949048620429E-12,-2.83313031417626));
#13603=CARTESIAN_POINT('Ctrl Pts',(11.0821305439588,2.00190131796994E-14,
-2.97881367266907));
#13604=CARTESIAN_POINT('Ctrl Pts',(11.0250134744288,2.11995977951848E-15,
-3.12449703116234));
#13605=CARTESIAN_POINT('Origin',(9.8,0.,-1.75));
#13606=CARTESIAN_POINT('',(10.78,-1.07231969947071E-7,-3.12449703081926));
#13607=CARTESIAN_POINT('Ctrl Pts',(11.0250134741351,-2.08166817117217E-16,
-3.12449703075067));
#13608=CARTESIAN_POINT('Ctrl Pts',(10.9841756494234,-2.08166817117217E-16,
-3.12449703075067));
#13609=CARTESIAN_POINT('Ctrl Pts',(10.9433378247117,-2.08166817117217E-16,
-3.12449703075067));
#13610=CARTESIAN_POINT('Ctrl Pts',(10.8616666666667,-2.08166817117217E-16,
-3.12449703075067));
#13611=CARTESIAN_POINT('Ctrl Pts',(10.8208333333333,-2.08166817117217E-16,
-3.12449703075067));
#13612=CARTESIAN_POINT('Ctrl Pts',(10.78,-2.08166817117217E-16,-3.12449703075067));
#13613=CARTESIAN_POINT('',(10.5350134750064,1.02273221749522E-10,-3.1244970310227));
#13614=CARTESIAN_POINT('Ctrl Pts',(10.78,-2.08166817117217E-16,-3.12449703075067));
#13615=CARTESIAN_POINT('Ctrl Pts',(10.7391666666667,-2.08166817117217E-16,
-3.12449703075067));
#13616=CARTESIAN_POINT('Ctrl Pts',(10.6983333333333,-2.08166817117217E-16,
-3.12449703075067));
#13617=CARTESIAN_POINT('Ctrl Pts',(10.6166711583355,-2.08166817117217E-16,
-3.12449703075067));
#13618=CARTESIAN_POINT('Ctrl Pts',(10.5758423166709,-2.08166817117217E-16,
-3.12449703075067));
#13619=CARTESIAN_POINT('Ctrl Pts',(10.5350134750064,-2.08166817117217E-16,
-3.12449703075067));
#13620=CARTESIAN_POINT('Ctrl Pts',(10.5350134747368,-3.00103482296057E-15,
-3.12449703112841));
#13621=CARTESIAN_POINT('Ctrl Pts',(10.4778952085294,-2.57860806401112E-14,
-2.97881062037814));
#13622=CARTESIAN_POINT('Ctrl Pts',(10.4207769423208,-5.52122510811137E-12,
-2.83312420962837));
#13623=CARTESIAN_POINT('Ctrl Pts',(10.3064909358382,-5.52122510811137E-12,
-2.54162519908909));
#13624=CARTESIAN_POINT('Ctrl Pts',(10.2493231955644,-4.57359866157433E-15,
-2.39581259929954));
#13625=CARTESIAN_POINT('Ctrl Pts',(10.1921554552908,6.1604094142004E-16,
-2.24999999950992));
#13626=CARTESIAN_POINT('Ctrl Pts',(5.553050567538,0.9783309087959,3.010992931911));
#13627=CARTESIAN_POINT('Ctrl Pts',(5.606133900872,0.4659514397387,3.177475113353));
#13628=CARTESIAN_POINT('Ctrl Pts',(5.712300567538,-0.6449686970874,3.242911847755));
#13629=CARTESIAN_POINT('Ctrl Pts',(5.871550567538,-2.147408477853,2.51427130483));
#13630=CARTESIAN_POINT('Ctrl Pts',(6.030800567538,-3.102099467523,1.144425205895));
#13631=CARTESIAN_POINT('Ctrl Pts',(6.190050567538,-3.265768497555,-0.5172460551353));
#13632=CARTESIAN_POINT('Ctrl Pts',(6.349300567538,-2.59663025113,-2.047018765263));
#13633=CARTESIAN_POINT('Ctrl Pts',(6.508550567538,-1.265333295377,-3.054784452443));
#13634=CARTESIAN_POINT('Ctrl Pts',(6.667800567538,0.3886344899198,-3.283555947824));
#13635=CARTESIAN_POINT('Ctrl Pts',(6.827050567538,1.943497179912,-2.674994390568));
#13636=CARTESIAN_POINT('Ctrl Pts',(6.986300567538,3.002752621272,-1.384287918735));
#13637=CARTESIAN_POINT('Ctrl Pts',(7.145550567538,3.296282150534,0.2594230316885));
#13638=CARTESIAN_POINT('Ctrl Pts',(7.304800567538,2.749233411565,1.836979036087));
#13639=CARTESIAN_POINT('Ctrl Pts',(7.464050567538,1.501108196656,2.946090716765));
#13640=CARTESIAN_POINT('Ctrl Pts',(7.623300567538,-0.1298115957604,3.303925737529));
#13641=CARTESIAN_POINT('Ctrl Pts',(7.782550567538,-1.727628394674,2.819233310576));
#13642=CARTESIAN_POINT('Ctrl Pts',(7.941800567538,-2.884886156338,1.615613875434));
#13643=CARTESIAN_POINT('Ctrl Pts',(8.101050567538,-3.30647490986,1.287858708565E-14));
#13644=CARTESIAN_POINT('Ctrl Pts',(8.260300567538,-2.884886156338,-1.615613875434));
#13645=CARTESIAN_POINT('Ctrl Pts',(8.419550567538,-1.727628394674,-2.819233310576));
#13646=CARTESIAN_POINT('Ctrl Pts',(8.578800567538,-0.1298115957604,-3.303925737529));
#13647=CARTESIAN_POINT('Ctrl Pts',(8.738050567538,1.501108196656,-2.946090716765));
#13648=CARTESIAN_POINT('Ctrl Pts',(8.897300567538,2.749233411565,-1.836979036087));
#13649=CARTESIAN_POINT('Ctrl Pts',(9.056550567538,3.296282150534,-0.2594230316885));
#13650=CARTESIAN_POINT('Ctrl Pts',(9.215800567538,3.002752621272,1.384287918735));
#13651=CARTESIAN_POINT('Ctrl Pts',(9.375050567538,1.943497179912,2.674994390568));
#13652=CARTESIAN_POINT('Ctrl Pts',(9.534300567538,0.3886344899198,3.283555947824));
#13653=CARTESIAN_POINT('Ctrl Pts',(9.693550567538,-1.265333295377,3.054784452443));
#13654=CARTESIAN_POINT('Ctrl Pts',(9.852800567538,-2.59663025113,2.047018765263));
#13655=CARTESIAN_POINT('Ctrl Pts',(10.01205056754,-3.265768497555,0.5172460551353));
#13656=CARTESIAN_POINT('Ctrl Pts',(10.17130056754,-3.102099467523,-1.144425205895));
#13657=CARTESIAN_POINT('Ctrl Pts',(10.33055056754,-2.147408477853,-2.51427130483));
#13658=CARTESIAN_POINT('Ctrl Pts',(10.48980056754,-0.6449686970875,-3.242911847755));
#13659=CARTESIAN_POINT('Ctrl Pts',(10.5959672342,0.4659514397387,-3.177475113353));
#13660=CARTESIAN_POINT('Ctrl Pts',(10.64905056754,0.9783309087958,-3.010992931911));
#13661=CARTESIAN_POINT('Ctrl Pts',(5.428016855846,0.8797657511871,2.707640568999));
#13662=CARTESIAN_POINT('Ctrl Pts',(5.481100189179,0.4190076330134,2.857349956793));
#13663=CARTESIAN_POINT('Ctrl Pts',(5.587266855846,-0.5799892093603,2.91619405267));
#13664=CARTESIAN_POINT('Ctrl Pts',(5.746516855846,-1.931060764449,2.260962792133));
#13665=CARTESIAN_POINT('Ctrl Pts',(5.905766855846,-2.789568277733,1.029126333319));
#13666=CARTESIAN_POINT('Ctrl Pts',(6.065016855846,-2.936747934286,-0.4651344040686));
#13667=CARTESIAN_POINT('Ctrl Pts',(6.224266855846,-2.335024216144,-1.840785142863));
#13668=CARTESIAN_POINT('Ctrl Pts',(6.383516855846,-1.137853140589,-2.747020169102));
#13669=CARTESIAN_POINT('Ctrl Pts',(6.542766855846,0.3494802330045,-2.952743329512));
#13670=CARTESIAN_POINT('Ctrl Pts',(6.702016855846,1.747693179314,-2.405493303218));
#13671=CARTESIAN_POINT('Ctrl Pts',(6.861266855846,2.700230455495,-1.244823290091));
#13672=CARTESIAN_POINT('Ctrl Pts',(7.020516855846,2.964187389171,0.2332866071149));
#13673=CARTESIAN_POINT('Ctrl Pts',(7.179766855846,2.472252870444,1.651906555408));
#13674=CARTESIAN_POINT('Ctrl Pts',(7.339016855846,1.34987412579,2.649277140482));
#13675=CARTESIAN_POINT('Ctrl Pts',(7.498266855846,-0.116733300594,2.971060897913));
#13676=CARTESIAN_POINT('Ctrl Pts',(7.657516855846,-1.553572803177,2.535200399938));
#13677=CARTESIAN_POINT('Ctrl Pts',(7.816766855846,-2.594238834326,1.452843554231));
#13678=CARTESIAN_POINT('Ctrl Pts',(7.976016855846,-2.973353245513,1.228623977058E-14));
#13679=CARTESIAN_POINT('Ctrl Pts',(8.135266855846,-2.594238834326,-1.452843554231));
#13680=CARTESIAN_POINT('Ctrl Pts',(8.294516855846,-1.553572803177,-2.535200399938));
#13681=CARTESIAN_POINT('Ctrl Pts',(8.453766855846,-0.1167333005941,-2.971060897913));
#13682=CARTESIAN_POINT('Ctrl Pts',(8.613016855846,1.34987412579,-2.649277140482));
#13683=CARTESIAN_POINT('Ctrl Pts',(8.772266855846,2.472252870444,-1.651906555408));
#13684=CARTESIAN_POINT('Ctrl Pts',(8.931516855846,2.964187389171,-0.2332866071149));
#13685=CARTESIAN_POINT('Ctrl Pts',(9.090766855846,2.700230455495,1.244823290091));
#13686=CARTESIAN_POINT('Ctrl Pts',(9.250016855846,1.747693179314,2.405493303218));
#13687=CARTESIAN_POINT('Ctrl Pts',(9.409266855846,0.3494802330045,2.952743329512));
#13688=CARTESIAN_POINT('Ctrl Pts',(9.568516855846,-1.137853140589,2.747020169102));
#13689=CARTESIAN_POINT('Ctrl Pts',(9.727766855846,-2.335024216144,1.840785142863));
#13690=CARTESIAN_POINT('Ctrl Pts',(9.887016855846,-2.936747934286,0.4651344040686));
#13691=CARTESIAN_POINT('Ctrl Pts',(10.04626685585,-2.789568277733,-1.029126333319));
#13692=CARTESIAN_POINT('Ctrl Pts',(10.20551685585,-1.931060764449,-2.260962792133));
#13693=CARTESIAN_POINT('Ctrl Pts',(10.36476685585,-0.5799892093604,-2.91619405267));
#13694=CARTESIAN_POINT('Ctrl Pts',(10.47093352251,0.4190076330134,-2.857349956793));
#13695=CARTESIAN_POINT('Ctrl Pts',(10.52401685585,0.8797657511871,-2.707640568999));
#13696=CARTESIAN_POINT('Ctrl Pts',(5.302983144154,0.7812005935783,2.404288206087));
#13697=CARTESIAN_POINT('Ctrl Pts',(5.356066477487,0.3720638262881,2.537224800233));
#13698=CARTESIAN_POINT('Ctrl Pts',(5.462233144154,-0.5150097216332,2.589476257585));
#13699=CARTESIAN_POINT('Ctrl Pts',(5.621483144154,-1.714713051046,2.007654279437));
#13700=CARTESIAN_POINT('Ctrl Pts',(5.780733144154,-2.477037087943,0.9138274607431));
#13701=CARTESIAN_POINT('Ctrl Pts',(5.939983144154,-2.607727371018,-0.4130227530019));
#13702=CARTESIAN_POINT('Ctrl Pts',(6.099233144154,-2.073418181158,-1.634551520464));
#13703=CARTESIAN_POINT('Ctrl Pts',(6.258483144154,-1.010372985802,-2.439255885761));
#13704=CARTESIAN_POINT('Ctrl Pts',(6.417733144154,0.3103259760892,-2.6219307112));
#13705=CARTESIAN_POINT('Ctrl Pts',(6.576983144154,1.551889178717,-2.135992215868));
#13706=CARTESIAN_POINT('Ctrl Pts',(6.736233144154,2.397708289717,-1.105358661447));
#13707=CARTESIAN_POINT('Ctrl Pts',(6.895483144154,2.632092627808,0.2071501825414));
#13708=CARTESIAN_POINT('Ctrl Pts',(7.054733144154,2.195272329322,1.466834074728));
#13709=CARTESIAN_POINT('Ctrl Pts',(7.213983144154,1.198640054924,2.3524635642));
#13710=CARTESIAN_POINT('Ctrl Pts',(7.373233144154,-0.1036550054277,2.638196058298));
#13711=CARTESIAN_POINT('Ctrl Pts',(7.532483144154,-1.37951721168,2.251167489299));
#13712=CARTESIAN_POINT('Ctrl Pts',(7.691733144154,-2.303591512314,1.290073233029));
#13713=CARTESIAN_POINT('Ctrl Pts',(7.850983144154,-2.640231581167,1.108429745068E-14));
#13714=CARTESIAN_POINT('Ctrl Pts',(8.010233144154,-2.303591512314,-1.290073233029));
#13715=CARTESIAN_POINT('Ctrl Pts',(8.169483144154,-1.37951721168,-2.251167489299));
#13716=CARTESIAN_POINT('Ctrl Pts',(8.328733144154,-0.1036550054277,-2.638196058298));
#13717=CARTESIAN_POINT('Ctrl Pts',(8.487983144154,1.198640054924,-2.3524635642));
#13718=CARTESIAN_POINT('Ctrl Pts',(8.647233144154,2.195272329322,-1.466834074728));
#13719=CARTESIAN_POINT('Ctrl Pts',(8.806483144154,2.632092627808,-0.2071501825414));
#13720=CARTESIAN_POINT('Ctrl Pts',(8.965733144154,2.397708289717,1.105358661447));
#13721=CARTESIAN_POINT('Ctrl Pts',(9.124983144154,1.551889178717,2.135992215868));
#13722=CARTESIAN_POINT('Ctrl Pts',(9.284233144154,0.3103259760892,2.6219307112));
#13723=CARTESIAN_POINT('Ctrl Pts',(9.443483144154,-1.010372985802,2.439255885761));
#13724=CARTESIAN_POINT('Ctrl Pts',(9.602733144154,-2.073418181158,1.634551520464));
#13725=CARTESIAN_POINT('Ctrl Pts',(9.761983144154,-2.607727371018,0.4130227530019));
#13726=CARTESIAN_POINT('Ctrl Pts',(9.921233144154,-2.477037087943,-0.913827460743));
#13727=CARTESIAN_POINT('Ctrl Pts',(10.08048314415,-1.714713051046,-2.007654279437));
#13728=CARTESIAN_POINT('Ctrl Pts',(10.23973314415,-0.5150097216332,-2.589476257585));
#13729=CARTESIAN_POINT('Ctrl Pts',(10.34589981082,0.3720638262881,-2.537224800233));
#13730=CARTESIAN_POINT('Ctrl Pts',(10.39898314415,0.7812005935783,-2.404288206087));
#13731=CARTESIAN_POINT('Ctrl Pts',(5.177949432462,0.6826354359695,2.100935843176));
#13732=CARTESIAN_POINT('Ctrl Pts',(5.231032765795,0.3251200195628,2.217099643673));
#13733=CARTESIAN_POINT('Ctrl Pts',(5.337199432462,-0.4500302339061,2.2627584625));
#13734=CARTESIAN_POINT('Ctrl Pts',(5.496449432462,-1.498365337642,1.754345766741));
#13735=CARTESIAN_POINT('Ctrl Pts',(5.655699432462,-2.164505898152,0.7985285881669));
#13736=CARTESIAN_POINT('Ctrl Pts',(5.814949432462,-2.278706807749,-0.3609111019352));
#13737=CARTESIAN_POINT('Ctrl Pts',(5.974199432462,-1.811812146172,-1.428317898065));
#13738=CARTESIAN_POINT('Ctrl Pts',(6.133449432462,-0.8828928310149,-2.13149160242));
#13739=CARTESIAN_POINT('Ctrl Pts',(6.292699432462,0.271171719174,-2.291118092888));
#13740=CARTESIAN_POINT('Ctrl Pts',(6.451949432462,1.35608517812,-1.866491128517));
#13741=CARTESIAN_POINT('Ctrl Pts',(6.611199432462,2.09518612394,-0.9658940328033));
#13742=CARTESIAN_POINT('Ctrl Pts',(6.770449432462,2.299997866445,0.1810137579678));
#13743=CARTESIAN_POINT('Ctrl Pts',(6.929699432462,1.918291788201,1.281761594049));
#13744=CARTESIAN_POINT('Ctrl Pts',(7.088949432462,1.047405984058,2.055649987917));
#13745=CARTESIAN_POINT('Ctrl Pts',(7.248199432462,-0.0905767102614,2.305331218682));
#13746=CARTESIAN_POINT('Ctrl Pts',(7.407449432462,-1.205461620183,1.967134578661));
#13747=CARTESIAN_POINT('Ctrl Pts',(7.566699432462,-2.012944190303,1.127302911826));
#13748=CARTESIAN_POINT('Ctrl Pts',(7.725949432462,-2.30710991682,0.));
#13749=CARTESIAN_POINT('Ctrl Pts',(7.885199432462,-2.012944190303,-1.127302911826));
#13750=CARTESIAN_POINT('Ctrl Pts',(8.044449432462,-1.205461620183,-1.967134578661));
#13751=CARTESIAN_POINT('Ctrl Pts',(8.203699432462,-0.09057671026141,-2.305331218682));
#13752=CARTESIAN_POINT('Ctrl Pts',(8.362949432462,1.047405984058,-2.055649987917));
#13753=CARTESIAN_POINT('Ctrl Pts',(8.522199432462,1.918291788201,-1.281761594049));
#13754=CARTESIAN_POINT('Ctrl Pts',(8.681449432462,2.299997866445,-0.1810137579678));
#13755=CARTESIAN_POINT('Ctrl Pts',(8.840699432462,2.09518612394,0.9658940328033));
#13756=CARTESIAN_POINT('Ctrl Pts',(8.999949432462,1.35608517812,1.866491128517));
#13757=CARTESIAN_POINT('Ctrl Pts',(9.159199432462,0.271171719174,2.291118092888));
#13758=CARTESIAN_POINT('Ctrl Pts',(9.318449432462,-0.8828928310149,2.13149160242));
#13759=CARTESIAN_POINT('Ctrl Pts',(9.477699432462,-1.811812146172,1.428317898065));
#13760=CARTESIAN_POINT('Ctrl Pts',(9.636949432462,-2.278706807749,0.3609111019352));
#13761=CARTESIAN_POINT('Ctrl Pts',(9.796199432462,-2.164505898152,-0.7985285881669));
#13762=CARTESIAN_POINT('Ctrl Pts',(9.955449432462,-1.498365337642,-1.754345766741));
#13763=CARTESIAN_POINT('Ctrl Pts',(10.11469943246,-0.4500302339061,-2.2627584625));
#13764=CARTESIAN_POINT('Ctrl Pts',(10.22086609913,0.3251200195628,-2.217099643673));
#13765=CARTESIAN_POINT('Ctrl Pts',(10.27394943246,0.6826354359695,-2.100935843176));
#13766=CARTESIAN_POINT('',(5.63499255472031,-7.41993575758981E-7,3.12499989450239));
#13767=CARTESIAN_POINT('Ctrl Pts',(5.634986107407,4.18742151866297E-6,3.12449702806922));
#13768=CARTESIAN_POINT('Ctrl Pts',(5.65695791239165,-0.220102539161386,
3.12463812164867));
#13769=CARTESIAN_POINT('Ctrl Pts',(5.67897662252065,-0.44064953200304,3.10173920341104));
#13770=CARTESIAN_POINT('Ctrl Pts',(5.72310569009851,-0.872618420486203,
3.00870846633561));
#13771=CARTESIAN_POINT('Ctrl Pts',(5.74514655866766,-1.08338856035468,2.93893917134752));
#13772=CARTESIAN_POINT('Ctrl Pts',(5.79629053209681,-1.55043320018977,2.72810358228179));
#13773=CARTESIAN_POINT('Ctrl Pts',(5.8377928382817,-1.92091911867348,2.51858797774256));
#13774=CARTESIAN_POINT('Ctrl Pts',(5.92921645078997,-2.54824617086085,1.8514803835448));
#13775=CARTESIAN_POINT('Ctrl Pts',(5.96919669615485,-2.76667000678542,1.50682910689432));
#13776=CARTESIAN_POINT('Ctrl Pts',(6.05240102883088,-3.06923750138772,0.73049620826951));
#13777=CARTESIAN_POINT('Ctrl Pts',(6.09319131879255,-3.13182588768285,0.318472133625857));
#13778=CARTESIAN_POINT('Ctrl Pts',(6.18384690093985,-3.11321199907849,-0.589454969171778));
#13779=CARTESIAN_POINT('Ctrl Pts',(6.22566769599382,-2.97612381593501,-0.996047824886898));
#13780=CARTESIAN_POINT('Ctrl Pts',(6.28566680271478,-2.7324562628559,-1.54560310783314));
#13781=CARTESIAN_POINT('Ctrl Pts',(6.32705708412113,-2.52230748364122,-1.91404302998656));
#13782=CARTESIAN_POINT('Ctrl Pts',(6.41557929492122,-1.87904024871203,-2.52442476815788));
#13783=CARTESIAN_POINT('Ctrl Pts',(6.4554980477788,-1.54078105288756,-2.75166775493571));
#13784=CARTESIAN_POINT('Ctrl Pts',(6.53843076181692,-0.768144592726403,
-3.05621103088525));
#13785=CARTESIAN_POINT('Ctrl Pts',(6.57908686746234,-0.359581070464692,
-3.13013165576389));
#13786=CARTESIAN_POINT('Ctrl Pts',(6.67176471540957,0.568604604224001,-3.11705696110184));
#13787=CARTESIAN_POINT('Ctrl Pts',(6.71373757339203,0.97756384079563,-2.98201038085689));
#13788=CARTESIAN_POINT('Ctrl Pts',(6.78430055630929,1.62585920990473,-2.69999321328485));
#13789=CARTESIAN_POINT('Ctrl Pts',(6.82487067374848,1.96613181358351,-2.46385086322353));
#13790=CARTESIAN_POINT('Ctrl Pts',(6.89543046710297,2.45553051679625,-1.95376212132779));
#13791=CARTESIAN_POINT('Ctrl Pts',(6.9367721787788,2.71875343764013,-1.62181272348741));
#13792=CARTESIAN_POINT('Ctrl Pts',(7.02751008605373,3.05336233804938,-0.776946962299042));
#13793=CARTESIAN_POINT('Ctrl Pts',(7.06791907246958,3.1286208842104,-0.371271841828463));
#13794=CARTESIAN_POINT('Ctrl Pts',(7.16122878779359,3.1195612174274,0.563189413652646));
#13795=CARTESIAN_POINT('Ctrl Pts',(7.20352621934902,2.98141015394773,0.975053271184048));
#13796=CARTESIAN_POINT('Ctrl Pts',(7.27288521992913,2.70782042248996,1.61380337445921));
#13797=CARTESIAN_POINT('Ctrl Pts',(7.31352769034975,2.47211612449969,1.95532520783703));
#13798=CARTESIAN_POINT('Ctrl Pts',(7.38355979919702,1.9681167518946,2.44349049201396));
#13799=CARTESIAN_POINT('Ctrl Pts',(7.42507806923627,1.63734153358997,2.7116624648552));
#13800=CARTESIAN_POINT('Ctrl Pts',(7.51669238599497,0.784710932292811,3.05077446246928));
#13801=CARTESIAN_POINT('Ctrl Pts',(7.55681070224769,0.382385740435282,3.12715191531059));
#13802=CARTESIAN_POINT('Ctrl Pts',(7.6420474933619,-0.471183768083625,3.12237996970145));
#13803=CARTESIAN_POINT('Ctrl Pts',(7.68300860642016,-0.877409231626726,
3.02091407068735));
#13804=CARTESIAN_POINT('Ctrl Pts',(7.7698414291264,-1.67903873524072,2.68319768942737));
#13805=CARTESIAN_POINT('Ctrl Pts',(7.81138319476979,-2.00874122018002,2.41423377541338));
#13806=CARTESIAN_POINT('Ctrl Pts',(7.87169428741273,-2.43162777346986,1.98258700351926));
#13807=CARTESIAN_POINT('Ctrl Pts',(7.91323523064669,-2.70311754303439,1.65387788875613));
#13808=CARTESIAN_POINT('Ctrl Pts',(8.00538249933744,-3.04697916736015,0.797280394573023));
#13809=CARTESIAN_POINT('Ctrl Pts',(8.04518829630558,-3.125,0.398671791438245));
#13810=CARTESIAN_POINT('Ctrl Pts',(8.12481170369442,-3.125,-0.398671791438237));
#13811=CARTESIAN_POINT('Ctrl Pts',(8.16461750066219,-3.04697916736015,-0.797280394573014));
#13812=CARTESIAN_POINT('Ctrl Pts',(8.25676476935278,-2.70311754303438,-1.65387788875615));
#13813=CARTESIAN_POINT('Ctrl Pts',(8.29830571258681,-2.43162777346985,-1.98258700351927));
#13814=CARTESIAN_POINT('Ctrl Pts',(8.35861680522996,-2.00874122018002,-2.41423377541338));
#13815=CARTESIAN_POINT('Ctrl Pts',(8.40015857087367,-1.67903873524071,-2.68319768942738));
#13816=CARTESIAN_POINT('Ctrl Pts',(8.48699139357988,-0.877409231626862,
-3.02091407068729));
#13817=CARTESIAN_POINT('Ctrl Pts',(8.52795250663794,-0.471183768083765,
-3.12237996970145));
#13818=CARTESIAN_POINT('Ctrl Pts',(8.61318929775226,0.382385740435305,-3.12715191531059));
#13819=CARTESIAN_POINT('Ctrl Pts',(8.65330761400518,0.78471093229284,-3.05077446246927));
#13820=CARTESIAN_POINT('Ctrl Pts',(8.74492193076395,1.63734153359001,-2.71166246485517));
#13821=CARTESIAN_POINT('Ctrl Pts',(8.78644020080312,1.96811675189465,-2.44349049201392));
#13822=CARTESIAN_POINT('Ctrl Pts',(8.85647230965024,2.47211612449972,-1.955325207837));
#13823=CARTESIAN_POINT('Ctrl Pts',(8.89711478007069,2.70782042248998,-1.61380337445918));
#13824=CARTESIAN_POINT('Ctrl Pts',(8.96647378065064,2.98141015394768,-0.975053271184154));
#13825=CARTESIAN_POINT('Ctrl Pts',(9.00877121220594,3.1195612174274,-0.563189413652753));
#13826=CARTESIAN_POINT('Ctrl Pts',(9.10208092752994,3.1286208842104,0.371271841828464));
#13827=CARTESIAN_POINT('Ctrl Pts',(9.14248991394583,3.05336233804938,0.776946962299041));
#13828=CARTESIAN_POINT('Ctrl Pts',(9.23322782122083,2.71875343764019,1.62181272348726));
#13829=CARTESIAN_POINT('Ctrl Pts',(9.27456953289673,2.45553051679638,1.95376212132765));
#13830=CARTESIAN_POINT('Ctrl Pts',(9.3451293262515,1.96613181358349,2.46385086322354));
#13831=CARTESIAN_POINT('Ctrl Pts',(9.38569944369098,1.6258592099047,2.69999321328487));
#13832=CARTESIAN_POINT('Ctrl Pts',(9.45626242660842,0.977563840795583,2.9820103808569));
#13833=CARTESIAN_POINT('Ctrl Pts',(9.49823528459103,0.568604604223939,3.11705696110185));
#13834=CARTESIAN_POINT('Ctrl Pts',(9.59091313253803,-0.35958107046477,3.13013165576388));
#13835=CARTESIAN_POINT('Ctrl Pts',(9.63156923818311,-0.768144592726469,
3.05621103088523));
#13836=CARTESIAN_POINT('Ctrl Pts',(9.71450195222103,-1.54078105288761,2.75166775493568));
#13837=CARTESIAN_POINT('Ctrl Pts',(9.75442070507848,-1.87904024871206,2.52442476815785));
#13838=CARTESIAN_POINT('Ctrl Pts',(9.84294291587878,-2.52230748364123,1.91404302998655));
#13839=CARTESIAN_POINT('Ctrl Pts',(9.88433319728545,-2.73245626285591,1.54560310783313));
#13840=CARTESIAN_POINT('Ctrl Pts',(9.94433230400693,-2.97612381593506,0.996047824886782));
#13841=CARTESIAN_POINT('Ctrl Pts',(9.98615309906173,-3.11321199907852,0.589454969171631));
#13842=CARTESIAN_POINT('Ctrl Pts',(10.0768086812096,-3.13182588768283,-0.318472133625934));
#13843=CARTESIAN_POINT('Ctrl Pts',(10.1175989711713,-3.06923750138772,-0.73049620826962));
#13844=CARTESIAN_POINT('Ctrl Pts',(10.2008033038473,-2.7666700067853,-1.50682910689455));
#13845=CARTESIAN_POINT('Ctrl Pts',(10.2407835492118,-2.54824617086069,-1.85148038354501));
#13846=CARTESIAN_POINT('Ctrl Pts',(10.33220716172,-1.92091911867334,-2.51858797774264));
#13847=CARTESIAN_POINT('Ctrl Pts',(10.3737094679055,-1.55043320018966,-2.72810358228187));
#13848=CARTESIAN_POINT('Ctrl Pts',(10.4248534244673,-1.08338871438423,-2.93893910181472));
#13849=CARTESIAN_POINT('Ctrl Pts',(10.446894276161,-0.872618743151924,-3.00870835952902));
#13850=CARTESIAN_POINT('Ctrl Pts',(10.4910232042645,-0.44065123519992,-3.10173887397661));
#13851=CARTESIAN_POINT('Ctrl Pts',(10.5130417918927,-0.220105501026149,
-3.12463783133622));
#13852=CARTESIAN_POINT('Ctrl Pts',(10.5350134746029,1.42376700706937E-10,
-3.12449703075058));
#13853=CARTESIAN_POINT('',(5.635,0.,3.125));
#13854=CARTESIAN_POINT('Ctrl Pts',(0.6530505675382,-0.9783309087958,-3.010992931911));
#13855=CARTESIAN_POINT('Ctrl Pts',(0.7061339008715,-0.4659514397387,-3.177475113353));
#13856=CARTESIAN_POINT('Ctrl Pts',(0.8123005675382,0.6449686970875,-3.242911847755));
#13857=CARTESIAN_POINT('Ctrl Pts',(0.9715505675382,2.147408477853,-2.51427130483));
#13858=CARTESIAN_POINT('Ctrl Pts',(1.130800567538,3.102099467523,-1.144425205895));
#13859=CARTESIAN_POINT('Ctrl Pts',(1.290050567538,3.265768497555,0.5172460551354));
#13860=CARTESIAN_POINT('Ctrl Pts',(1.449300567538,2.59663025113,2.047018765263));
#13861=CARTESIAN_POINT('Ctrl Pts',(1.608550567538,1.265333295377,3.054784452443));
#13862=CARTESIAN_POINT('Ctrl Pts',(1.767800567538,-0.3886344899198,3.283555947824));
#13863=CARTESIAN_POINT('Ctrl Pts',(1.927050567538,-1.943497179912,2.674994390568));
#13864=CARTESIAN_POINT('Ctrl Pts',(2.086300567538,-3.002752621272,1.384287918735));
#13865=CARTESIAN_POINT('Ctrl Pts',(2.245550567538,-3.296282150534,-0.2594230316885));
#13866=CARTESIAN_POINT('Ctrl Pts',(2.404800567538,-2.749233411565,-1.836979036087));
#13867=CARTESIAN_POINT('Ctrl Pts',(2.564050567538,-1.501108196656,-2.946090716765));
#13868=CARTESIAN_POINT('Ctrl Pts',(2.723300567538,0.1298115957604,-3.303925737529));
#13869=CARTESIAN_POINT('Ctrl Pts',(2.882550567538,1.727628394674,-2.819233310576));
#13870=CARTESIAN_POINT('Ctrl Pts',(3.041800567538,2.884886156338,-1.615613875434));
#13871=CARTESIAN_POINT('Ctrl Pts',(3.201050567538,3.30647490986,0.));
#13872=CARTESIAN_POINT('Ctrl Pts',(3.360300567538,2.884886156338,1.615613875434));
#13873=CARTESIAN_POINT('Ctrl Pts',(3.519550567538,1.727628394674,2.819233310576));
#13874=CARTESIAN_POINT('Ctrl Pts',(3.678800567538,0.1298115957604,3.303925737529));
#13875=CARTESIAN_POINT('Ctrl Pts',(3.838050567538,-1.501108196656,2.946090716765));
#13876=CARTESIAN_POINT('Ctrl Pts',(3.997300567538,-2.749233411565,1.836979036087));
#13877=CARTESIAN_POINT('Ctrl Pts',(4.156550567538,-3.296282150534,0.2594230316885));
#13878=CARTESIAN_POINT('Ctrl Pts',(4.315800567538,-3.002752621272,-1.384287918735));
#13879=CARTESIAN_POINT('Ctrl Pts',(4.475050567538,-1.943497179912,-2.674994390568));
#13880=CARTESIAN_POINT('Ctrl Pts',(4.634300567538,-0.3886344899198,-3.283555947824));
#13881=CARTESIAN_POINT('Ctrl Pts',(4.793550567538,1.265333295377,-3.054784452443));
#13882=CARTESIAN_POINT('Ctrl Pts',(4.952800567538,2.59663025113,-2.047018765263));
#13883=CARTESIAN_POINT('Ctrl Pts',(5.112050567538,3.265768497555,-0.5172460551353));
#13884=CARTESIAN_POINT('Ctrl Pts',(5.271300567538,3.102099467523,1.144425205895));
#13885=CARTESIAN_POINT('Ctrl Pts',(5.430550567538,2.147408477853,2.51427130483));
#13886=CARTESIAN_POINT('Ctrl Pts',(5.589800567538,0.6449686970875,3.242911847755));
#13887=CARTESIAN_POINT('Ctrl Pts',(5.695967234205,-0.4659514397387,3.177475113353));
#13888=CARTESIAN_POINT('Ctrl Pts',(5.749050567538,-0.9783309087958,3.010992931911));
#13889=CARTESIAN_POINT('Ctrl Pts',(0.5280168558461,-0.8797657511871,-2.707640568999));
#13890=CARTESIAN_POINT('Ctrl Pts',(0.5811001891794,-0.4190076330134,-2.857349956793));
#13891=CARTESIAN_POINT('Ctrl Pts',(0.6872668558461,0.5799892093603,-2.91619405267));
#13892=CARTESIAN_POINT('Ctrl Pts',(0.8465168558461,1.931060764449,-2.260962792133));
#13893=CARTESIAN_POINT('Ctrl Pts',(1.005766855846,2.789568277733,-1.029126333319));
#13894=CARTESIAN_POINT('Ctrl Pts',(1.165016855846,2.936747934286,0.4651344040687));
#13895=CARTESIAN_POINT('Ctrl Pts',(1.324266855846,2.335024216144,1.840785142863));
#13896=CARTESIAN_POINT('Ctrl Pts',(1.483516855846,1.137853140589,2.747020169102));
#13897=CARTESIAN_POINT('Ctrl Pts',(1.642766855846,-0.3494802330045,2.952743329512));
#13898=CARTESIAN_POINT('Ctrl Pts',(1.802016855846,-1.747693179314,2.405493303218));
#13899=CARTESIAN_POINT('Ctrl Pts',(1.961266855846,-2.700230455495,1.244823290091));
#13900=CARTESIAN_POINT('Ctrl Pts',(2.120516855846,-2.964187389171,-0.2332866071149));
#13901=CARTESIAN_POINT('Ctrl Pts',(2.279766855846,-2.472252870444,-1.651906555408));
#13902=CARTESIAN_POINT('Ctrl Pts',(2.439016855846,-1.34987412579,-2.649277140482));
#13903=CARTESIAN_POINT('Ctrl Pts',(2.598266855846,0.1167333005941,-2.971060897913));
#13904=CARTESIAN_POINT('Ctrl Pts',(2.757516855846,1.553572803177,-2.535200399938));
#13905=CARTESIAN_POINT('Ctrl Pts',(2.916766855846,2.594238834326,-1.452843554231));
#13906=CARTESIAN_POINT('Ctrl Pts',(3.076016855846,2.973353245513,0.));
#13907=CARTESIAN_POINT('Ctrl Pts',(3.235266855846,2.594238834326,1.452843554231));
#13908=CARTESIAN_POINT('Ctrl Pts',(3.394516855846,1.553572803177,2.535200399938));
#13909=CARTESIAN_POINT('Ctrl Pts',(3.553766855846,0.1167333005941,2.971060897913));
#13910=CARTESIAN_POINT('Ctrl Pts',(3.713016855846,-1.34987412579,2.649277140482));
#13911=CARTESIAN_POINT('Ctrl Pts',(3.872266855846,-2.472252870444,1.651906555408));
#13912=CARTESIAN_POINT('Ctrl Pts',(4.031516855846,-2.964187389171,0.2332866071149));
#13913=CARTESIAN_POINT('Ctrl Pts',(4.190766855846,-2.700230455495,-1.244823290091));
#13914=CARTESIAN_POINT('Ctrl Pts',(4.350016855846,-1.747693179314,-2.405493303218));
#13915=CARTESIAN_POINT('Ctrl Pts',(4.509266855846,-0.3494802330045,-2.952743329512));
#13916=CARTESIAN_POINT('Ctrl Pts',(4.668516855846,1.137853140589,-2.747020169102));
#13917=CARTESIAN_POINT('Ctrl Pts',(4.827766855846,2.335024216144,-1.840785142863));
#13918=CARTESIAN_POINT('Ctrl Pts',(4.987016855846,2.936747934286,-0.4651344040686));
#13919=CARTESIAN_POINT('Ctrl Pts',(5.146266855846,2.789568277733,1.029126333319));
#13920=CARTESIAN_POINT('Ctrl Pts',(5.305516855846,1.931060764449,2.260962792133));
#13921=CARTESIAN_POINT('Ctrl Pts',(5.464766855846,0.5799892093604,2.91619405267));
#13922=CARTESIAN_POINT('Ctrl Pts',(5.570933522513,-0.4190076330134,2.857349956793));
#13923=CARTESIAN_POINT('Ctrl Pts',(5.624016855846,-0.8797657511871,2.707640568999));
#13924=CARTESIAN_POINT('Ctrl Pts',(0.4029831441539,-0.7812005935783,-2.404288206087));
#13925=CARTESIAN_POINT('Ctrl Pts',(0.4560664774873,-0.3720638262881,-2.537224800233));
#13926=CARTESIAN_POINT('Ctrl Pts',(0.5622331441539,0.5150097216332,-2.589476257585));
#13927=CARTESIAN_POINT('Ctrl Pts',(0.7214831441539,1.714713051046,-2.007654279437));
#13928=CARTESIAN_POINT('Ctrl Pts',(0.8807331441539,2.477037087943,-0.9138274607431));
#13929=CARTESIAN_POINT('Ctrl Pts',(1.039983144154,2.607727371018,0.413022753002));
#13930=CARTESIAN_POINT('Ctrl Pts',(1.199233144154,2.073418181158,1.634551520464));
#13931=CARTESIAN_POINT('Ctrl Pts',(1.358483144154,1.010372985802,2.439255885761));
#13932=CARTESIAN_POINT('Ctrl Pts',(1.517733144154,-0.3103259760893,2.6219307112));
#13933=CARTESIAN_POINT('Ctrl Pts',(1.676983144154,-1.551889178717,2.135992215868));
#13934=CARTESIAN_POINT('Ctrl Pts',(1.836233144154,-2.397708289717,1.105358661447));
#13935=CARTESIAN_POINT('Ctrl Pts',(1.995483144154,-2.632092627808,-0.2071501825414));
#13936=CARTESIAN_POINT('Ctrl Pts',(2.154733144154,-2.195272329322,-1.466834074728));
#13937=CARTESIAN_POINT('Ctrl Pts',(2.313983144154,-1.198640054924,-2.3524635642));
#13938=CARTESIAN_POINT('Ctrl Pts',(2.473233144154,0.1036550054277,-2.638196058298));
#13939=CARTESIAN_POINT('Ctrl Pts',(2.632483144154,1.37951721168,-2.251167489299));
#13940=CARTESIAN_POINT('Ctrl Pts',(2.791733144154,2.303591512314,-1.290073233029));
#13941=CARTESIAN_POINT('Ctrl Pts',(2.950983144154,2.640231581167,0.));
#13942=CARTESIAN_POINT('Ctrl Pts',(3.110233144154,2.303591512314,1.290073233029));
#13943=CARTESIAN_POINT('Ctrl Pts',(3.269483144154,1.37951721168,2.251167489299));
#13944=CARTESIAN_POINT('Ctrl Pts',(3.428733144154,0.1036550054277,2.638196058298));
#13945=CARTESIAN_POINT('Ctrl Pts',(3.587983144154,-1.198640054924,2.3524635642));
#13946=CARTESIAN_POINT('Ctrl Pts',(3.747233144154,-2.195272329322,1.466834074728));
#13947=CARTESIAN_POINT('Ctrl Pts',(3.906483144154,-2.632092627808,0.2071501825414));
#13948=CARTESIAN_POINT('Ctrl Pts',(4.065733144154,-2.397708289717,-1.105358661447));
#13949=CARTESIAN_POINT('Ctrl Pts',(4.224983144154,-1.551889178717,-2.135992215868));
#13950=CARTESIAN_POINT('Ctrl Pts',(4.384233144154,-0.3103259760893,-2.6219307112));
#13951=CARTESIAN_POINT('Ctrl Pts',(4.543483144154,1.010372985802,-2.439255885761));
#13952=CARTESIAN_POINT('Ctrl Pts',(4.702733144154,2.073418181158,-1.634551520464));
#13953=CARTESIAN_POINT('Ctrl Pts',(4.861983144154,2.607727371018,-0.4130227530019));
#13954=CARTESIAN_POINT('Ctrl Pts',(5.021233144154,2.477037087943,0.913827460743));
#13955=CARTESIAN_POINT('Ctrl Pts',(5.180483144154,1.714713051046,2.007654279437));
#13956=CARTESIAN_POINT('Ctrl Pts',(5.339733144154,0.5150097216332,2.589476257585));
#13957=CARTESIAN_POINT('Ctrl Pts',(5.445899810821,-0.3720638262881,2.537224800233));
#13958=CARTESIAN_POINT('Ctrl Pts',(5.498983144154,-0.7812005935783,2.404288206087));
#13959=CARTESIAN_POINT('Ctrl Pts',(0.2779494324618,-0.6826354359695,-2.100935843176));
#13960=CARTESIAN_POINT('Ctrl Pts',(0.3310327657952,-0.3251200195628,-2.217099643673));
#13961=CARTESIAN_POINT('Ctrl Pts',(0.4371994324618,0.4500302339061,-2.2627584625));
#13962=CARTESIAN_POINT('Ctrl Pts',(0.5964494324618,1.498365337642,-1.754345766741));
#13963=CARTESIAN_POINT('Ctrl Pts',(0.7556994324618,2.164505898152,-0.7985285881669));
#13964=CARTESIAN_POINT('Ctrl Pts',(0.9149494324618,2.278706807749,0.3609111019353));
#13965=CARTESIAN_POINT('Ctrl Pts',(1.074199432462,1.811812146172,1.428317898065));
#13966=CARTESIAN_POINT('Ctrl Pts',(1.233449432462,0.8828928310149,2.13149160242));
#13967=CARTESIAN_POINT('Ctrl Pts',(1.392699432462,-0.271171719174,2.291118092888));
#13968=CARTESIAN_POINT('Ctrl Pts',(1.551949432462,-1.35608517812,1.866491128517));
#13969=CARTESIAN_POINT('Ctrl Pts',(1.711199432462,-2.09518612394,0.9658940328033));
#13970=CARTESIAN_POINT('Ctrl Pts',(1.870449432462,-2.299997866445,-0.1810137579678));
#13971=CARTESIAN_POINT('Ctrl Pts',(2.029699432462,-1.918291788201,-1.281761594049));
#13972=CARTESIAN_POINT('Ctrl Pts',(2.188949432462,-1.047405984058,-2.055649987917));
#13973=CARTESIAN_POINT('Ctrl Pts',(2.348199432462,0.09057671026141,-2.305331218682));
#13974=CARTESIAN_POINT('Ctrl Pts',(2.507449432462,1.205461620183,-1.967134578661));
#13975=CARTESIAN_POINT('Ctrl Pts',(2.666699432462,2.012944190303,-1.127302911826));
#13976=CARTESIAN_POINT('Ctrl Pts',(2.825949432462,2.30710991682,0.));
#13977=CARTESIAN_POINT('Ctrl Pts',(2.985199432462,2.012944190303,1.127302911826));
#13978=CARTESIAN_POINT('Ctrl Pts',(3.144449432462,1.205461620183,1.967134578661));
#13979=CARTESIAN_POINT('Ctrl Pts',(3.303699432462,0.09057671026142,2.305331218682));
#13980=CARTESIAN_POINT('Ctrl Pts',(3.462949432462,-1.047405984058,2.055649987917));
#13981=CARTESIAN_POINT('Ctrl Pts',(3.622199432462,-1.918291788201,1.281761594049));
#13982=CARTESIAN_POINT('Ctrl Pts',(3.781449432462,-2.299997866445,0.1810137579678));
#13983=CARTESIAN_POINT('Ctrl Pts',(3.940699432462,-2.09518612394,-0.9658940328033));
#13984=CARTESIAN_POINT('Ctrl Pts',(4.099949432462,-1.35608517812,-1.866491128517));
#13985=CARTESIAN_POINT('Ctrl Pts',(4.259199432462,-0.271171719174,-2.291118092888));
#13986=CARTESIAN_POINT('Ctrl Pts',(4.418449432462,0.8828928310149,-2.13149160242));
#13987=CARTESIAN_POINT('Ctrl Pts',(4.577699432462,1.811812146172,-1.428317898065));
#13988=CARTESIAN_POINT('Ctrl Pts',(4.736949432462,2.278706807749,-0.3609111019352));
#13989=CARTESIAN_POINT('Ctrl Pts',(4.896199432462,2.164505898152,0.7985285881669));
#13990=CARTESIAN_POINT('Ctrl Pts',(5.055449432462,1.498365337642,1.754345766741));
#13991=CARTESIAN_POINT('Ctrl Pts',(5.214699432462,0.4500302339061,2.2627584625));
#13992=CARTESIAN_POINT('Ctrl Pts',(5.320866099128,-0.3251200195628,2.217099643673));
#13993=CARTESIAN_POINT('Ctrl Pts',(5.373949432462,-0.6826354359695,2.100935843176));
#13994=CARTESIAN_POINT('Ctrl Pts',(0.734986525425182,1.56341571633245E-10,
-3.12449703075077));
#13995=CARTESIAN_POINT('Ctrl Pts',(0.756958211791874,0.220105537948462,
-3.12463783133899));
#13996=CARTESIAN_POINT('Ctrl Pts',(0.77897680314279,0.440651309409153,-3.10173886632448));
#13997=CARTESIAN_POINT('Ctrl Pts',(0.823105731360934,0.872618815068403,
-3.00870833572373));
#13998=CARTESIAN_POINT('Ctrl Pts',(0.845146579294268,1.08338874871482,-2.93893908631705));
#13999=CARTESIAN_POINT('Ctrl Pts',(0.896290532096981,1.55043320018977,-2.72810358228179));
#14000=CARTESIAN_POINT('Ctrl Pts',(0.937792838281873,1.92091911867349,-2.51858797774255));
#14001=CARTESIAN_POINT('Ctrl Pts',(1.02921645079008,2.54824617086085,-1.85148038354479));
#14002=CARTESIAN_POINT('Ctrl Pts',(1.06919669615493,2.76667000678543,-1.50682910689431));
#14003=CARTESIAN_POINT('Ctrl Pts',(1.1524010288309,3.06923750138774,-0.730496208269469));
#14004=CARTESIAN_POINT('Ctrl Pts',(1.19319131879256,3.13182588768285,-0.318472133625813));
#14005=CARTESIAN_POINT('Ctrl Pts',(1.28384690093984,3.11321199907849,0.589454969171711));
#14006=CARTESIAN_POINT('Ctrl Pts',(1.32566769599381,2.97612381593505,0.996047824886831));
#14007=CARTESIAN_POINT('Ctrl Pts',(1.38566680271478,2.73245626285591,1.54560310783312));
#14008=CARTESIAN_POINT('Ctrl Pts',(1.42705708412114,2.52230748364124,1.91404302998655));
#14009=CARTESIAN_POINT('Ctrl Pts',(1.51557929492124,1.879040248712,2.5244247681579));
#14010=CARTESIAN_POINT('Ctrl Pts',(1.55549804777882,1.54078105288753,2.75166775493572));
#14011=CARTESIAN_POINT('Ctrl Pts',(1.63843076181693,0.768144592726395,3.05621103088525));
#14012=CARTESIAN_POINT('Ctrl Pts',(1.67908686746235,0.359581070464684,3.13013165576389));
#14013=CARTESIAN_POINT('Ctrl Pts',(1.77176471540958,-0.56860460422401,3.11705696110184));
#14014=CARTESIAN_POINT('Ctrl Pts',(1.81373757339203,-0.977563840795641,
2.98201038085689));
#14015=CARTESIAN_POINT('Ctrl Pts',(1.8843005563093,-1.62585920990474,2.69999321328485));
#14016=CARTESIAN_POINT('Ctrl Pts',(1.92487067374849,-1.96613181358352,2.46385086322352));
#14017=CARTESIAN_POINT('Ctrl Pts',(1.99543046710298,-2.45553051679632,1.95376212132772));
#14018=CARTESIAN_POINT('Ctrl Pts',(2.03677217877881,-2.71875343764016,1.62181272348734));
#14019=CARTESIAN_POINT('Ctrl Pts',(2.12751008605373,-3.05336233804938,0.776946962299037));
#14020=CARTESIAN_POINT('Ctrl Pts',(2.16791907246958,-3.1286208842104,0.371271841828459));
#14021=CARTESIAN_POINT('Ctrl Pts',(2.2612287877936,-3.1195612174274,-0.563189413652693));
#14022=CARTESIAN_POINT('Ctrl Pts',(2.30352621934903,-2.98141015394771,-0.975053271184097));
#14023=CARTESIAN_POINT('Ctrl Pts',(2.37288521992913,-2.70782042248996,-1.61380337445921));
#14024=CARTESIAN_POINT('Ctrl Pts',(2.41352769034975,-2.47211612449969,-1.95532520783703));
#14025=CARTESIAN_POINT('Ctrl Pts',(2.48355979919702,-1.9681167518946,-2.44349049201396));
#14026=CARTESIAN_POINT('Ctrl Pts',(2.52507806923627,-1.63734153358997,-2.7116624648552));
#14027=CARTESIAN_POINT('Ctrl Pts',(2.61669238599497,-0.784710932292806,
-3.05077446246928));
#14028=CARTESIAN_POINT('Ctrl Pts',(2.65681070224768,-0.382385740435277,
-3.12715191531059));
#14029=CARTESIAN_POINT('Ctrl Pts',(2.74204749336189,0.471183768083628,-3.12237996970145));
#14030=CARTESIAN_POINT('Ctrl Pts',(2.78300860642015,0.877409231626729,-3.02091407068735));
#14031=CARTESIAN_POINT('Ctrl Pts',(2.8698414291264,1.67903873524071,-2.68319768942737));
#14032=CARTESIAN_POINT('Ctrl Pts',(2.91138319476978,2.00874122018001,-2.41423377541338));
#14033=CARTESIAN_POINT('Ctrl Pts',(2.97169428741273,2.43162777346987,-1.98258700351926));
#14034=CARTESIAN_POINT('Ctrl Pts',(3.01323523064669,2.70311754303439,-1.65387788875612));
#14035=CARTESIAN_POINT('Ctrl Pts',(3.10538249933744,3.04697916736015,-0.797280394573023));
#14036=CARTESIAN_POINT('Ctrl Pts',(3.14518829630558,3.125,-0.398671791438245));
#14037=CARTESIAN_POINT('Ctrl Pts',(3.22481170369442,3.125,0.398671791438237));
#14038=CARTESIAN_POINT('Ctrl Pts',(3.26461750066218,3.04697916736015,0.797280394573014));
#14039=CARTESIAN_POINT('Ctrl Pts',(3.35676476935278,2.70311754303438,1.65387788875616));
#14040=CARTESIAN_POINT('Ctrl Pts',(3.39830571258681,2.43162777346985,1.98258700351928));
#14041=CARTESIAN_POINT('Ctrl Pts',(3.45861680522996,2.00874122018001,2.41423377541339));
#14042=CARTESIAN_POINT('Ctrl Pts',(3.50015857087367,1.6790387352407,2.68319768942739));
#14043=CARTESIAN_POINT('Ctrl Pts',(3.58699139357987,0.877409231626872,3.02091407068728));
#14044=CARTESIAN_POINT('Ctrl Pts',(3.62795250663793,0.471183768083777,3.12237996970145));
#14045=CARTESIAN_POINT('Ctrl Pts',(3.71318929775225,-0.3823857404353,3.12715191531059));
#14046=CARTESIAN_POINT('Ctrl Pts',(3.75330761400518,-0.784710932292834,
3.05077446246928));
#14047=CARTESIAN_POINT('Ctrl Pts',(3.84492193076394,-1.63734153359002,2.71166246485517));
#14048=CARTESIAN_POINT('Ctrl Pts',(3.88644020080312,-1.96811675189465,2.44349049201392));
#14049=CARTESIAN_POINT('Ctrl Pts',(3.95647230965024,-2.47211612449971,1.955325207837));
#14050=CARTESIAN_POINT('Ctrl Pts',(3.99711478007069,-2.70782042248997,1.61380337445918));
#14051=CARTESIAN_POINT('Ctrl Pts',(4.06647378065064,-2.98141015394767,0.975053271184186));
#14052=CARTESIAN_POINT('Ctrl Pts',(4.10877121220594,-3.1195612174274,0.563189413652785));
#14053=CARTESIAN_POINT('Ctrl Pts',(4.20208092752994,-3.1286208842104,-0.371271841828458));
#14054=CARTESIAN_POINT('Ctrl Pts',(4.24248991394583,-3.05336233804938,-0.776946962299035));
#14055=CARTESIAN_POINT('Ctrl Pts',(4.33322782122083,-2.71875343764019,-1.62181272348727));
#14056=CARTESIAN_POINT('Ctrl Pts',(4.37456953289673,-2.45553051679637,-1.95376212132766));
#14057=CARTESIAN_POINT('Ctrl Pts',(4.44512932625149,-1.9661318135835,-2.46385086322354));
#14058=CARTESIAN_POINT('Ctrl Pts',(4.48569944369097,-1.62585920990471,-2.69999321328487));
#14059=CARTESIAN_POINT('Ctrl Pts',(4.55626242660842,-0.97756384079559,-2.9820103808569));
#14060=CARTESIAN_POINT('Ctrl Pts',(4.59823528459102,-0.568604604223948,
-3.11705696110185));
#14061=CARTESIAN_POINT('Ctrl Pts',(4.69091313253802,0.35958107046476,-3.13013165576389));
#14062=CARTESIAN_POINT('Ctrl Pts',(4.73156923818309,0.76814459272646,-3.05621103088524));
#14063=CARTESIAN_POINT('Ctrl Pts',(4.81450195222101,1.5407810528876,-2.75166775493569));
#14064=CARTESIAN_POINT('Ctrl Pts',(4.85442070507863,1.87904024871205,-2.52442476815786));
#14065=CARTESIAN_POINT('Ctrl Pts',(4.94294291587866,2.52230748364104,-1.91404302998674));
#14066=CARTESIAN_POINT('Ctrl Pts',(4.98433319728502,2.7324562628558,-1.54560310783341));
#14067=CARTESIAN_POINT('Ctrl Pts',(5.04433230400602,2.97612381593511,-0.996047824886731));
#14068=CARTESIAN_POINT('Ctrl Pts',(5.08615309905995,3.1132119990785,-0.589454969171663));
#14069=CARTESIAN_POINT('Ctrl Pts',(5.17680868120734,3.13182588768285,0.318472133625777));
#14070=CARTESIAN_POINT('Ctrl Pts',(5.21759897116921,3.06923750138774,0.730496208269473));
#14071=CARTESIAN_POINT('Ctrl Pts',(5.30080330384511,2.7666700067854,1.50682910689435));
#14072=CARTESIAN_POINT('Ctrl Pts',(5.3407835492096,2.54824617086083,1.85148038354482));
#14073=CARTESIAN_POINT('Ctrl Pts',(5.43220716171777,1.92091911867348,2.51858797774255));
#14074=CARTESIAN_POINT('Ctrl Pts',(5.47370946790287,1.55043320018978,2.72810358228179));
#14075=CARTESIAN_POINT('Ctrl Pts',(5.52485344133227,1.08338856035471,2.9389391713475));
#14076=CARTESIAN_POINT('Ctrl Pts',(5.54689430990158,0.87261842048627,3.00870846633559));
#14077=CARTESIAN_POINT('Ctrl Pts',(5.59102300077564,0.440653219467686,3.1017384092623));
#14078=CARTESIAN_POINT('Ctrl Pts',(5.61304133631232,0.220110064033209,3.12463734035084));
#14079=CARTESIAN_POINT('Ctrl Pts',(5.63501276810388,7.07736163903239E-6,
3.12449703527009));
#14080=CARTESIAN_POINT('Ctrl Pts',(0.9259788629516,-0.9656781074217,-2.972051613422));
#14081=CARTESIAN_POINT('Ctrl Pts',(0.979062196285,-0.4599252670358,-3.136380672689));
#14082=CARTESIAN_POINT('Ctrl Pts',(1.085228862952,0.6366272854614,-3.200971110614));
#14083=CARTESIAN_POINT('Ctrl Pts',(1.244478862952,2.119635939241,-2.481754111378));
#14084=CARTESIAN_POINT('Ctrl Pts',(1.403728862952,3.061979863765,-1.129624298873));
#14085=CARTESIAN_POINT('Ctrl Pts',(1.562978862952,3.223532154246,0.5105564866689));
#14086=CARTESIAN_POINT('Ctrl Pts',(1.722228862952,2.563047905408,2.020544571702));
#14087=CARTESIAN_POINT('Ctrl Pts',(1.881478862952,1.248968678135,3.015276776083));
#14088=CARTESIAN_POINT('Ctrl Pts',(2.040728862952,-0.383608261101,3.241089558554));
#14089=CARTESIAN_POINT('Ctrl Pts',(2.199978862952,-1.918361836065,2.640398557608));
#14090=CARTESIAN_POINT('Ctrl Pts',(2.359228862952,-2.963917875123,1.366384855545));
#14091=CARTESIAN_POINT('Ctrl Pts',(2.518478862952,-3.253651172662,-0.256067900963));
#14092=CARTESIAN_POINT('Ctrl Pts',(2.677728862952,-2.713677441724,-1.813221296591));
#14093=CARTESIAN_POINT('Ctrl Pts',(2.836978862952,-1.481694291113,-2.907988781792));
#14094=CARTESIAN_POINT('Ctrl Pts',(2.996228862952,0.1281327360592,-3.261195904774));
#14095=CARTESIAN_POINT('Ctrl Pts',(3.155478862952,1.705284892359,-2.782772028626));
#14096=CARTESIAN_POINT('Ctrl Pts',(3.314728862952,2.84757578293,-1.59471906236));
#14097=CARTESIAN_POINT('Ctrl Pts',(3.473978862952,3.263712108535,0.));
#14098=CARTESIAN_POINT('Ctrl Pts',(3.633228862952,2.84757578293,1.59471906236));
#14099=CARTESIAN_POINT('Ctrl Pts',(3.792478862952,1.705284892359,2.782772028626));
#14100=CARTESIAN_POINT('Ctrl Pts',(3.951728862952,0.1281327360592,3.261195904774));
#14101=CARTESIAN_POINT('Ctrl Pts',(4.110978862952,-1.481694291113,2.907988781792));
#14102=CARTESIAN_POINT('Ctrl Pts',(4.270228862952,-2.713677441724,1.813221296591));
#14103=CARTESIAN_POINT('Ctrl Pts',(4.429478862952,-3.253651172662,0.256067900963));
#14104=CARTESIAN_POINT('Ctrl Pts',(4.588728862952,-2.963917875123,-1.366384855545));
#14105=CARTESIAN_POINT('Ctrl Pts',(4.747978862952,-1.918361836065,-2.640398557608));
#14106=CARTESIAN_POINT('Ctrl Pts',(4.907228862952,-0.383608261101,-3.241089558554));
#14107=CARTESIAN_POINT('Ctrl Pts',(5.066478862952,1.248968678135,-3.015276776083));
#14108=CARTESIAN_POINT('Ctrl Pts',(5.225728862952,2.563047905408,-2.020544571702));
#14109=CARTESIAN_POINT('Ctrl Pts',(5.384978862952,3.223532154246,-0.510556486669));
#14110=CARTESIAN_POINT('Ctrl Pts',(5.544228862952,3.061979863765,1.129624298873));
#14111=CARTESIAN_POINT('Ctrl Pts',(5.703478862952,2.119635939241,2.481754111378));
#14112=CARTESIAN_POINT('Ctrl Pts',(5.862728862952,0.6366272854614,3.200971110614));
#14113=CARTESIAN_POINT('Ctrl Pts',(5.968895529618,-0.4599252670358,3.136380672689));
#14114=CARTESIAN_POINT('Ctrl Pts',(6.021978862952,-0.9656781074217,2.972051613422));
#14115=CARTESIAN_POINT('Ctrl Pts',(0.8149929543172,-0.9656781074217,-2.972051613422));
#14116=CARTESIAN_POINT('Ctrl Pts',(0.8680762876505,-0.4599252670358,-3.136380672689));
#14117=CARTESIAN_POINT('Ctrl Pts',(0.9742429543172,0.6366272854614,-3.200971110614));
#14118=CARTESIAN_POINT('Ctrl Pts',(1.133492954317,2.119635939241,-2.481754111378));
#14119=CARTESIAN_POINT('Ctrl Pts',(1.292742954317,3.061979863765,-1.129624298873));
#14120=CARTESIAN_POINT('Ctrl Pts',(1.451992954317,3.223532154246,0.5105564866689));
#14121=CARTESIAN_POINT('Ctrl Pts',(1.611242954317,2.563047905408,2.020544571702));
#14122=CARTESIAN_POINT('Ctrl Pts',(1.770492954317,1.248968678135,3.015276776083));
#14123=CARTESIAN_POINT('Ctrl Pts',(1.929742954317,-0.383608261101,3.241089558554));
#14124=CARTESIAN_POINT('Ctrl Pts',(2.088992954317,-1.918361836065,2.640398557608));
#14125=CARTESIAN_POINT('Ctrl Pts',(2.248242954317,-2.963917875123,1.366384855545));
#14126=CARTESIAN_POINT('Ctrl Pts',(2.407492954317,-3.253651172662,-0.256067900963));
#14127=CARTESIAN_POINT('Ctrl Pts',(2.566742954317,-2.713677441724,-1.813221296591));
#14128=CARTESIAN_POINT('Ctrl Pts',(2.725992954317,-1.481694291113,-2.907988781792));
#14129=CARTESIAN_POINT('Ctrl Pts',(2.885242954317,0.1281327360592,-3.261195904774));
#14130=CARTESIAN_POINT('Ctrl Pts',(3.044492954317,1.705284892359,-2.782772028626));
#14131=CARTESIAN_POINT('Ctrl Pts',(3.203742954317,2.84757578293,-1.59471906236));
#14132=CARTESIAN_POINT('Ctrl Pts',(3.362992954317,3.263712108535,0.));
#14133=CARTESIAN_POINT('Ctrl Pts',(3.522242954317,2.84757578293,1.59471906236));
#14134=CARTESIAN_POINT('Ctrl Pts',(3.681492954317,1.705284892359,2.782772028626));
#14135=CARTESIAN_POINT('Ctrl Pts',(3.840742954317,0.1281327360592,3.261195904774));
#14136=CARTESIAN_POINT('Ctrl Pts',(3.999992954317,-1.481694291113,2.907988781792));
#14137=CARTESIAN_POINT('Ctrl Pts',(4.159242954317,-2.713677441724,1.813221296591));
#14138=CARTESIAN_POINT('Ctrl Pts',(4.318492954317,-3.253651172662,0.256067900963));
#14139=CARTESIAN_POINT('Ctrl Pts',(4.477742954317,-2.963917875123,-1.366384855545));
#14140=CARTESIAN_POINT('Ctrl Pts',(4.636992954317,-1.918361836065,-2.640398557608));
#14141=CARTESIAN_POINT('Ctrl Pts',(4.796242954317,-0.383608261101,-3.241089558554));
#14142=CARTESIAN_POINT('Ctrl Pts',(4.955492954317,1.248968678135,-3.015276776083));
#14143=CARTESIAN_POINT('Ctrl Pts',(5.114742954317,2.563047905408,-2.020544571702));
#14144=CARTESIAN_POINT('Ctrl Pts',(5.273992954317,3.223532154246,-0.510556486669));
#14145=CARTESIAN_POINT('Ctrl Pts',(5.433242954317,3.061979863765,1.129624298873));
#14146=CARTESIAN_POINT('Ctrl Pts',(5.592492954317,2.119635939241,2.481754111378));
#14147=CARTESIAN_POINT('Ctrl Pts',(5.751742954317,0.6366272854614,3.200971110614));
#14148=CARTESIAN_POINT('Ctrl Pts',(5.857909620984,-0.4599252670358,3.136380672689));
#14149=CARTESIAN_POINT('Ctrl Pts',(5.910992954317,-0.9656781074217,2.972051613422));
#14150=CARTESIAN_POINT('Ctrl Pts',(0.7040070456828,-0.9656781074217,-2.972051613422));
#14151=CARTESIAN_POINT('Ctrl Pts',(0.7570903790161,-0.4599252670358,-3.136380672689));
#14152=CARTESIAN_POINT('Ctrl Pts',(0.8632570456828,0.6366272854614,-3.200971110614));
#14153=CARTESIAN_POINT('Ctrl Pts',(1.022507045683,2.119635939241,-2.481754111378));
#14154=CARTESIAN_POINT('Ctrl Pts',(1.181757045683,3.061979863765,-1.129624298873));
#14155=CARTESIAN_POINT('Ctrl Pts',(1.341007045683,3.223532154246,0.5105564866689));
#14156=CARTESIAN_POINT('Ctrl Pts',(1.500257045683,2.563047905408,2.020544571702));
#14157=CARTESIAN_POINT('Ctrl Pts',(1.659507045683,1.248968678135,3.015276776083));
#14158=CARTESIAN_POINT('Ctrl Pts',(1.818757045683,-0.383608261101,3.241089558554));
#14159=CARTESIAN_POINT('Ctrl Pts',(1.978007045683,-1.918361836065,2.640398557608));
#14160=CARTESIAN_POINT('Ctrl Pts',(2.137257045683,-2.963917875123,1.366384855545));
#14161=CARTESIAN_POINT('Ctrl Pts',(2.296507045683,-3.253651172662,-0.256067900963));
#14162=CARTESIAN_POINT('Ctrl Pts',(2.455757045683,-2.713677441724,-1.813221296591));
#14163=CARTESIAN_POINT('Ctrl Pts',(2.615007045683,-1.481694291113,-2.907988781792));
#14164=CARTESIAN_POINT('Ctrl Pts',(2.774257045683,0.1281327360592,-3.261195904774));
#14165=CARTESIAN_POINT('Ctrl Pts',(2.933507045683,1.705284892359,-2.782772028626));
#14166=CARTESIAN_POINT('Ctrl Pts',(3.092757045683,2.84757578293,-1.59471906236));
#14167=CARTESIAN_POINT('Ctrl Pts',(3.252007045683,3.263712108535,0.));
#14168=CARTESIAN_POINT('Ctrl Pts',(3.411257045683,2.84757578293,1.59471906236));
#14169=CARTESIAN_POINT('Ctrl Pts',(3.570507045683,1.705284892359,2.782772028626));
#14170=CARTESIAN_POINT('Ctrl Pts',(3.729757045683,0.1281327360592,3.261195904774));
#14171=CARTESIAN_POINT('Ctrl Pts',(3.889007045683,-1.481694291113,2.907988781792));
#14172=CARTESIAN_POINT('Ctrl Pts',(4.048257045683,-2.713677441724,1.813221296591));
#14173=CARTESIAN_POINT('Ctrl Pts',(4.207507045683,-3.253651172662,0.256067900963));
#14174=CARTESIAN_POINT('Ctrl Pts',(4.366757045683,-2.963917875123,-1.366384855545));
#14175=CARTESIAN_POINT('Ctrl Pts',(4.526007045683,-1.918361836065,-2.640398557608));
#14176=CARTESIAN_POINT('Ctrl Pts',(4.685257045683,-0.383608261101,-3.241089558554));
#14177=CARTESIAN_POINT('Ctrl Pts',(4.844507045683,1.248968678135,-3.015276776083));
#14178=CARTESIAN_POINT('Ctrl Pts',(5.003757045683,2.563047905408,-2.020544571702));
#14179=CARTESIAN_POINT('Ctrl Pts',(5.163007045683,3.223532154246,-0.510556486669));
#14180=CARTESIAN_POINT('Ctrl Pts',(5.322257045683,3.061979863765,1.129624298873));
#14181=CARTESIAN_POINT('Ctrl Pts',(5.481507045683,2.119635939241,2.481754111378));
#14182=CARTESIAN_POINT('Ctrl Pts',(5.640757045683,0.6366272854614,3.200971110614));
#14183=CARTESIAN_POINT('Ctrl Pts',(5.746923712349,-0.4599252670358,3.136380672689));
#14184=CARTESIAN_POINT('Ctrl Pts',(5.800007045683,-0.9656781074217,2.972051613422));
#14185=CARTESIAN_POINT('Ctrl Pts',(0.5930211370484,-0.9656781074217,-2.972051613422));
#14186=CARTESIAN_POINT('Ctrl Pts',(0.6461044703817,-0.4599252670358,-3.136380672689));
#14187=CARTESIAN_POINT('Ctrl Pts',(0.7522711370484,0.6366272854614,-3.200971110614));
#14188=CARTESIAN_POINT('Ctrl Pts',(0.9115211370484,2.119635939241,-2.481754111378));
#14189=CARTESIAN_POINT('Ctrl Pts',(1.070771137048,3.061979863765,-1.129624298873));
#14190=CARTESIAN_POINT('Ctrl Pts',(1.230021137048,3.223532154246,0.5105564866689));
#14191=CARTESIAN_POINT('Ctrl Pts',(1.389271137048,2.563047905408,2.020544571702));
#14192=CARTESIAN_POINT('Ctrl Pts',(1.548521137048,1.248968678135,3.015276776083));
#14193=CARTESIAN_POINT('Ctrl Pts',(1.707771137048,-0.383608261101,3.241089558554));
#14194=CARTESIAN_POINT('Ctrl Pts',(1.867021137048,-1.918361836065,2.640398557608));
#14195=CARTESIAN_POINT('Ctrl Pts',(2.026271137048,-2.963917875123,1.366384855545));
#14196=CARTESIAN_POINT('Ctrl Pts',(2.185521137048,-3.253651172662,-0.256067900963));
#14197=CARTESIAN_POINT('Ctrl Pts',(2.344771137048,-2.713677441724,-1.813221296591));
#14198=CARTESIAN_POINT('Ctrl Pts',(2.504021137048,-1.481694291113,-2.907988781792));
#14199=CARTESIAN_POINT('Ctrl Pts',(2.663271137048,0.1281327360592,-3.261195904774));
#14200=CARTESIAN_POINT('Ctrl Pts',(2.822521137048,1.705284892359,-2.782772028626));
#14201=CARTESIAN_POINT('Ctrl Pts',(2.981771137048,2.84757578293,-1.59471906236));
#14202=CARTESIAN_POINT('Ctrl Pts',(3.141021137048,3.263712108535,0.));
#14203=CARTESIAN_POINT('Ctrl Pts',(3.300271137048,2.84757578293,1.59471906236));
#14204=CARTESIAN_POINT('Ctrl Pts',(3.459521137048,1.705284892359,2.782772028626));
#14205=CARTESIAN_POINT('Ctrl Pts',(3.618771137048,0.1281327360592,3.261195904774));
#14206=CARTESIAN_POINT('Ctrl Pts',(3.778021137048,-1.481694291113,2.907988781792));
#14207=CARTESIAN_POINT('Ctrl Pts',(3.937271137048,-2.713677441724,1.813221296591));
#14208=CARTESIAN_POINT('Ctrl Pts',(4.096521137048,-3.253651172662,0.256067900963));
#14209=CARTESIAN_POINT('Ctrl Pts',(4.255771137048,-2.963917875123,-1.366384855545));
#14210=CARTESIAN_POINT('Ctrl Pts',(4.415021137048,-1.918361836065,-2.640398557608));
#14211=CARTESIAN_POINT('Ctrl Pts',(4.574271137048,-0.383608261101,-3.241089558554));
#14212=CARTESIAN_POINT('Ctrl Pts',(4.733521137048,1.248968678135,-3.015276776083));
#14213=CARTESIAN_POINT('Ctrl Pts',(4.892771137048,2.563047905408,-2.020544571702));
#14214=CARTESIAN_POINT('Ctrl Pts',(5.052021137048,3.223532154246,-0.510556486669));
#14215=CARTESIAN_POINT('Ctrl Pts',(5.211271137048,3.061979863765,1.129624298873));
#14216=CARTESIAN_POINT('Ctrl Pts',(5.370521137048,2.119635939241,2.481754111378));
#14217=CARTESIAN_POINT('Ctrl Pts',(5.529771137048,0.6366272854614,3.200971110614));
#14218=CARTESIAN_POINT('Ctrl Pts',(5.635937803715,-0.4599252670358,3.136380672689));
#14219=CARTESIAN_POINT('Ctrl Pts',(5.689021137048,-0.9656781074217,2.972051613422));
#14220=CARTESIAN_POINT('',(5.88,-1.32348898008484E-22,3.125));
#14221=CARTESIAN_POINT('',(5.88,0.,3.125));
#14222=CARTESIAN_POINT('Ctrl Pts',(0.98,3.2169591004938E-7,-3.12449703095644));
#14223=CARTESIAN_POINT('Ctrl Pts',(0.9957051282051,0.157306535044492,-3.12459764304402));
#14224=CARTESIAN_POINT('Ctrl Pts',(1.01141025641005,0.314639539052909,-3.112929841749));
#14225=CARTESIAN_POINT('Ctrl Pts',(1.02711538461519,0.470193579471061,-3.08937038670253));
#14226=CARTESIAN_POINT('Ctrl Pts',(1.03182698771781,0.516860431844727,-3.08230245321972));
#14227=CARTESIAN_POINT('Ctrl Pts',(1.03653859082045,0.563365438343652,-3.07416446995282));
#14228=CARTESIAN_POINT('Ctrl Pts',(1.04125019392309,0.609657256300367,-3.06495400126008));
#14229=CARTESIAN_POINT('Ctrl Pts',(1.05224371902567,0.717669381189642,-3.04346332885533));
#14230=CARTESIAN_POINT('Ctrl Pts',(1.0632372441283,0.824520523417935,-3.01613287001461));
#14231=CARTESIAN_POINT('Ctrl Pts',(1.07423076923084,0.929617596829347,-2.98324879794399));
#14232=CARTESIAN_POINT('Ctrl Pts',(1.089935897436,1.07975715593506,-2.93627127590627));
#14233=CARTESIAN_POINT('Ctrl Pts',(1.10564102564099,1.22632914373851,-2.87796151164342));
#14234=CARTESIAN_POINT('Ctrl Pts',(1.12134615384615,1.36775803719343,-2.8091039241222));
#14235=CARTESIAN_POINT('Ctrl Pts',(1.13705128205133,1.5091869306485,-2.74024633660091));
#14236=CARTESIAN_POINT('Ctrl Pts',(1.15275641025667,1.64548597437029,-2.66083432711573));
#14237=CARTESIAN_POINT('Ctrl Pts',(1.16846153846185,1.77506014945936,-2.57161807835128));
#14238=CARTESIAN_POINT('Ctrl Pts',(1.17914097076807,1.86317013579121,-2.51095134091064));
#14239=CARTESIAN_POINT('Ctrl Pts',(1.18982040307421,1.94817288076982,-2.44574669164713));
#14240=CARTESIAN_POINT('Ctrl Pts',(1.20049983538033,2.02952515103173,-2.37626864249983));
#14241=CARTESIAN_POINT('Ctrl Pts',(1.20552553127922,2.06780918704612,-2.34357256496935));
#14242=CARTESIAN_POINT('Ctrl Pts',(1.2105512271781,2.10528488988288,-2.30993026036317));
#14243=CARTESIAN_POINT('Ctrl Pts',(1.21557692307699,2.14191592065948,-2.27539299236903));
#14244=CARTESIAN_POINT('Ctrl Pts',(1.23128205128199,2.25638664196909,-2.16746520831449));
#14245=CARTESIAN_POINT('Ctrl Pts',(1.24698717948701,2.36259770943883,-2.05080969082419));
#14246=CARTESIAN_POINT('Ctrl Pts',(1.26269230769218,2.45953351178139,-1.92692186650592));
#14247=CARTESIAN_POINT('Ctrl Pts',(1.27839743589734,2.55646931412384,-1.80303404218777));
#14248=CARTESIAN_POINT('Ctrl Pts',(1.29410256410266,2.64414127751746,-1.6719042538725));
#14249=CARTESIAN_POINT('Ctrl Pts',(1.30980769230782,2.72154967470347,-1.53495847225765));
#14250=CARTESIAN_POINT('Ctrl Pts',(1.32551282051299,2.79895807188956,-1.39801269064265));
#14251=CARTESIAN_POINT('Ctrl Pts',(1.34121794871801,2.86610550760182,-1.25523572060086));
#14252=CARTESIAN_POINT('Ctrl Pts',(1.35692307692301,2.92192333127629,-1.10813935100359));
#14253=CARTESIAN_POINT('Ctrl Pts',(1.35786539277047,2.9252724296811,-1.09931349244548));
#14254=CARTESIAN_POINT('Ctrl Pts',(1.35880770861792,2.92858070337731,-1.09047219858789));
#14255=CARTESIAN_POINT('Ctrl Pts',(1.35975002446537,2.93184792475783,-1.08161580336685));
#14256=CARTESIAN_POINT('Ctrl Pts',(1.37451283682291,2.98303392179007,-0.942866889013087));
#14257=CARTESIAN_POINT('Ctrl Pts',(1.38927564918046,3.02414182613375,-0.800411122418192));
#14258=CARTESIAN_POINT('Ctrl Pts',(1.40403846153816,3.05502438429729,-0.655798952752522));
#14259=CARTESIAN_POINT('Ctrl Pts',(1.41974358974334,3.08787818772652,-0.50195613408092));
#14260=CARTESIAN_POINT('Ctrl Pts',(1.4354487179487,3.10916841598543,-0.345660030799849));
#14261=CARTESIAN_POINT('Ctrl Pts',(1.45115384615389,3.1187342224115,-0.188648419769014));
#14262=CARTESIAN_POINT('Ctrl Pts',(1.46685897435902,3.12830002883752,-0.0316368087388328));
#14263=CARTESIAN_POINT('Ctrl Pts',(1.48256410256397,3.12614026969898,0.12610510103707));
#14264=CARTESIAN_POINT('Ctrl Pts',(1.49826923076908,3.11205714799653,0.282798238157188));
#14265=CARTESIAN_POINT('Ctrl Pts',(1.50517951072145,3.10586055333675,0.351743453374321));
#14266=CARTESIAN_POINT('Ctrl Pts',(1.51208979067384,3.09735519217736,0.420484489677447));
#14267=CARTESIAN_POINT('Ctrl Pts',(1.51900007062624,3.0865260643595,0.488857703250767));
#14268=CARTESIAN_POINT('Ctrl Pts',(1.52779491887912,3.07274362189333,0.575877627491321));
#14269=CARTESIAN_POINT('Ctrl Pts',(1.536589767132,3.05519690668903,0.66230164565767));
#14270=CARTESIAN_POINT('Ctrl Pts',(1.54538461538482,3.0340200977109,0.74781859016398));
#14271=CARTESIAN_POINT('Ctrl Pts',(1.56108974359,2.99620426616755,0.900527828411023));
#14272=CARTESIAN_POINT('Ctrl Pts',(1.576794871795,2.94681582966476,1.05034855944726));
#14273=CARTESIAN_POINT('Ctrl Pts',(1.5925,2.88658577275698,1.1956628320182));
#14274=CARTESIAN_POINT('Ctrl Pts',(1.608205128205,2.82635571584919,1.34097710458913));
#14275=CARTESIAN_POINT('Ctrl Pts',(1.62391025641,2.75527937991822,1.48179891776845));
#14276=CARTESIAN_POINT('Ctrl Pts',(1.63961538461517,2.67404531641151,1.61651716219695));
#14277=CARTESIAN_POINT('Ctrl Pts',(1.65249354986765,2.60743359059155,1.72698578057497));
#14278=CARTESIAN_POINT('Ctrl Pts',(1.66537171512024,2.53398384454478,1.83335602635669));
#14279=CARTESIAN_POINT('Ctrl Pts',(1.67824988037278,2.45411540900217,1.93466859159332));
#14280=CARTESIAN_POINT('Ctrl Pts',(1.68107684332548,2.43658301180572,1.9569083177461));
#14281=CARTESIAN_POINT('Ctrl Pts',(1.68390380627817,2.41874138908149,1.97890437133876));
#14282=CARTESIAN_POINT('Ctrl Pts',(1.68673076923086,2.4005992967642,2.00064999697506));
#14283=CARTESIAN_POINT('Ctrl Pts',(1.70243589743605,2.29981131668746,2.12145732421479));
#14284=CARTESIAN_POINT('Ctrl Pts',(1.71814102564111,2.18976698077217,2.23451450223418));
#14285=CARTESIAN_POINT('Ctrl Pts',(1.73384615384633,2.07193616153301,2.33873186210924));
#14286=CARTESIAN_POINT('Ctrl Pts',(1.74955128205139,1.95410534229508,2.44294922198321));
#14287=CARTESIAN_POINT('Ctrl Pts',(1.76525641025661,1.82847988986133,2.53833958057375));
#14288=CARTESIAN_POINT('Ctrl Pts',(1.78096153846167,1.69644712969505,2.62385329049029));
#14289=CARTESIAN_POINT('Ctrl Pts',(1.79666666666689,1.56441436952739,2.70936700040773));
#14290=CARTESIAN_POINT('Ctrl Pts',(1.81237179487195,1.42595984987577,2.78500861783667));
#14291=CARTESIAN_POINT('Ctrl Pts',(1.82807692307697,1.28252819003516,2.84966078036119));
#14292=CARTESIAN_POINT('Ctrl Pts',(1.83121799320022,1.25384145182002,2.86259139598291));
#14293=CARTESIAN_POINT('Ctrl Pts',(1.83435906332346,1.22495656311743,2.8750820037678));
#14294=CARTESIAN_POINT('Ctrl Pts',(1.83750013344671,1.19588572614117,2.887123539098));
#14295=CARTESIAN_POINT('Ctrl Pts',(1.85006419152849,1.07960443666829,2.93528882778825));
#14296=CARTESIAN_POINT('Ctrl Pts',(1.86262824961027,0.960347655502351,2.97626761538678));
#14297=CARTESIAN_POINT('Ctrl Pts',(1.87519230769217,0.83908019289306,3.00992620370386));
#14298=CARTESIAN_POINT('Ctrl Pts',(1.89089743589733,0.687495327956873,3.05199958805779));
#14299=CARTESIAN_POINT('Ctrl Pts',(1.90660256410267,0.532757793114142,3.08264413157538));
#14300=CARTESIAN_POINT('Ctrl Pts',(1.92230769230783,0.376606556598297,3.10163498008567));
#14301=CARTESIAN_POINT('Ctrl Pts',(1.938012820513,0.220455320082452,3.12062582859596));
#14302=CARTESIAN_POINT('Ctrl Pts',(1.953717948718,0.0628756645481053,3.12796387302098));
#14303=CARTESIAN_POINT('Ctrl Pts',(1.96942307692303,-0.0943789619765685,
3.12338542308761));
#14304=CARTESIAN_POINT('Ctrl Pts',(1.97853202085236,-0.185586340671023,
3.12072993099726));
#14305=CARTESIAN_POINT('Ctrl Pts',(1.9876409647817,-0.276685802602259,3.11406434039434));
#14306=CARTESIAN_POINT('Ctrl Pts',(1.99674990871107,-0.367304367055667,
3.1033389279845));
#14307=CARTESIAN_POINT('Ctrl Pts',(2.0033460929868,-0.432925228768213,3.09557218825737));
#14308=CARTESIAN_POINT('Ctrl Pts',(2.00994227726255,-0.49829389512535,3.0856767051092));
#14309=CARTESIAN_POINT('Ctrl Pts',(2.01653846153833,-0.563276981103758,
3.07370359533635));
#14310=CARTESIAN_POINT('Ctrl Pts',(2.03224358974339,-0.717997900620613,
3.04519632262624));
#14311=CARTESIAN_POINT('Ctrl Pts',(2.04794871794861,-0.870526272338106,
3.00491480017494));
#14312=CARTESIAN_POINT('Ctrl Pts',(2.06365384615367,-1.01920094228015,2.95353305961267));
#14313=CARTESIAN_POINT('Ctrl Pts',(2.07935897435889,-1.16787561222373,2.90215131904986));
#14314=CARTESIAN_POINT('Ctrl Pts',(2.09506410256395,-1.31271118268685,2.83966664030563));
#14315=CARTESIAN_POINT('Ctrl Pts',(2.11076923076914,-1.45207966320917,2.76670577109897));
#14316=CARTESIAN_POINT('Ctrl Pts',(2.12584614949763,-1.58587336592168,2.69666335686228));
#14317=CARTESIAN_POINT('Ctrl Pts',(2.14092306822624,-1.71463784791186,2.61695511461419));
#14318=CARTESIAN_POINT('Ctrl Pts',(2.15599998695471,-1.836828913414,2.52817810742183));
#14319=CARTESIAN_POINT('Ctrl Pts',(2.15662819643142,-1.84192024452083,2.52447903878345));
#14320=CARTESIAN_POINT('Ctrl Pts',(2.15725640590813,-1.8470001649315,2.52076422913783));
#14321=CARTESIAN_POINT('Ctrl Pts',(2.15788461538483,-1.85206859791098,2.51703377008661));
#14322=CARTESIAN_POINT('Ctrl Pts',(2.17358974359,-1.97877854529902,2.42377293936711));
#14323=CARTESIAN_POINT('Ctrl Pts',(2.189294871795,-2.09828043057227,2.32075011669408));
#14324=CARTESIAN_POINT('Ctrl Pts',(2.205,-2.20940661429584,2.20940720229315));
#14325=CARTESIAN_POINT('Ctrl Pts',(2.220705128205,-2.32053279801942,2.09806428789222));
#14326=CARTESIAN_POINT('Ctrl Pts',(2.23641025641,-2.42329735285879,1.97839483543744));
#14327=CARTESIAN_POINT('Ctrl Pts',(2.25211538461517,-2.51660034679189,1.85174928324409));
#14328=CARTESIAN_POINT('Ctrl Pts',(2.26782051282033,-2.60990334072498,1.72510373105075));
#14329=CARTESIAN_POINT('Ctrl Pts',(2.28352564102567,-2.69375117108915,1.59146857523107));
#14330=CARTESIAN_POINT('Ctrl Pts',(2.29923076923086,-2.76698261297629,1.45222443021403));
#14331=CARTESIAN_POINT('Ctrl Pts',(2.30457056320872,-2.79188153817257,1.40488097415942));
#14332=CARTESIAN_POINT('Ctrl Pts',(2.30991035718657,-2.81555228674541,1.35689047491984));
#14333=CARTESIAN_POINT('Ctrl Pts',(2.31525015116441,-2.83794741820317,1.30831167980417));
#14334=CARTESIAN_POINT('Ctrl Pts',(2.3256154853917,-2.88141969889172,1.21401301400872));
#14335=CARTESIAN_POINT('Ctrl Pts',(2.33598081961898,-2.9200846630212,1.11749740512214));
#14336=CARTESIAN_POINT('Ctrl Pts',(2.34634615384633,-2.95384328122045,1.01930854475146));
#14337=CARTESIAN_POINT('Ctrl Pts',(2.36205128205139,-3.00499295138217,0.87053682098386));
#14338=CARTESIAN_POINT('Ctrl Pts',(2.37775641025661,-3.04488646955173,0.717917299307509));
#14339=CARTESIAN_POINT('Ctrl Pts',(2.39346153846167,-3.07323267657501,0.563190821606756));
#14340=CARTESIAN_POINT('Ctrl Pts',(2.40916666666689,-3.10157888359858,0.408464343904395));
#14341=CARTESIAN_POINT('Ctrl Pts',(2.42487179487195,-3.11838067165169,0.25161647302184));
#14342=CARTESIAN_POINT('Ctrl Pts',(2.44057692307697,-3.12331108802163,0.094376207787104));
#14343=CARTESIAN_POINT('Ctrl Pts',(2.45188456103662,-3.12686097074617,-0.0188362390481932));
#14344=CARTESIAN_POINT('Ctrl Pts',(2.46319219899625,-3.12425420322951,-0.132257831845052));
#14345=CARTESIAN_POINT('Ctrl Pts',(2.47449983695594,-3.11536666791583,-0.245184674149663));
#14346=CARTESIAN_POINT('Ctrl Pts',(2.47889732720134,-3.11191034485466,-0.289101422213973));
#14347=CARTESIAN_POINT('Ctrl Pts',(2.48329481744675,-3.10750429091715,-0.332943335439869));
#14348=CARTESIAN_POINT('Ctrl Pts',(2.48769230769217,-3.10216193300488,-0.37667061407462));
#14349=CARTESIAN_POINT('Ctrl Pts',(2.50339743589733,-3.08308231912341,-0.532837536272352));
#14350=CARTESIAN_POINT('Ctrl Pts',(2.51910256410267,-3.05206338319806,-0.687523279012142));
#14351=CARTESIAN_POINT('Ctrl Pts',(2.53480769230783,-3.0097189125242,-0.839021679403842));
#14352=CARTESIAN_POINT('Ctrl Pts',(2.550512820513,-2.96737444185033,-0.990520079795541));
#14353=CARTESIAN_POINT('Ctrl Pts',(2.566217948718,-2.91370372918221,-1.13884614555346));
#14354=CARTESIAN_POINT('Ctrl Pts',(2.58192307692303,-2.84927329204631,-1.28235426733883));
#14355=CARTESIAN_POINT('Ctrl Pts',(2.59762820512805,-2.78484285491041,-1.42586238912421));
#14356=CARTESIAN_POINT('Ctrl Pts',(2.61333333333311,-2.70964227733817,-1.56456383704047));
#14357=CARTESIAN_POINT('Ctrl Pts',(2.62903846153833,-2.62426134529928,-1.69671142476984));
#14358=CARTESIAN_POINT('Ctrl Pts',(2.6306089923509,-2.61572315428164,-1.70992633493315));
#14359=CARTESIAN_POINT('Ctrl Pts',(2.63217952316347,-2.60708334093589,-1.72307544280506));
#14360=CARTESIAN_POINT('Ctrl Pts',(2.63375005397604,-2.59834253844517,-1.7361569781865));
#14361=CARTESIAN_POINT('Ctrl Pts',(2.64788465136855,-2.5196763173783,-1.85388929799372));
#14362=CARTESIAN_POINT('Ctrl Pts',(2.66201924876118,-2.4328286128156,-1.96614691665661));
#14363=CARTESIAN_POINT('Ctrl Pts',(2.67615384615367,-2.33882800562177,-2.07202028766332));
#14364=CARTESIAN_POINT('Ctrl Pts',(2.69185897435889,-2.23438275356725,-2.18965751630222));
#14365=CARTESIAN_POINT('Ctrl Pts',(2.70756410256395,-2.12110179310409,-2.29942752308062));
#14366=CARTESIAN_POINT('Ctrl Pts',(2.72326923076914,-2.00029920318409,-2.40017868230316));
#14367=CARTESIAN_POINT('Ctrl Pts',(2.73897435897433,-1.87949661326408,-2.5009298415257));
#14368=CARTESIAN_POINT('Ctrl Pts',(2.75467948717967,-1.75116000914845,-2.59267025933498));
#14369=CARTESIAN_POINT('Ctrl Pts',(2.77038461538483,-1.61660883785066,-2.674197927153));
#14370=CARTESIAN_POINT('Ctrl Pts',(2.77792308497015,-1.55202420668778,-2.71333124947796));
#14371=CARTESIAN_POINT('Ctrl Pts',(2.78546155455542,-1.48600787178097,-2.75011066378684));
#14372=CARTESIAN_POINT('Ctrl Pts',(2.79300002414067,-1.41872031168613,-2.78439538808883));
#14373=CARTESIAN_POINT('Ctrl Pts',(2.80116668276046,-1.34582560455246,-2.82153709650612));
#14374=CARTESIAN_POINT('Ctrl Pts',(2.80933334138023,-1.27143900290213,-2.85575093945237));
#14375=CARTESIAN_POINT('Ctrl Pts',(2.8175,-1.19582529175154,-2.88697719853058));
#14376=CARTESIAN_POINT('Ctrl Pts',(2.833205128205,-1.05041416549221,-2.94702775592731));
#14377=CARTESIAN_POINT('Ctrl Pts',(2.84891025641,-0.900465813463126,-2.99603287482205));
#14378=CARTESIAN_POINT('Ctrl Pts',(2.86461538461517,-0.747723396432291,
-3.03363235324925));
#14379=CARTESIAN_POINT('Ctrl Pts',(2.88032051282033,-0.594980979401457,
-3.07123183167645));
#14380=CARTESIAN_POINT('Ctrl Pts',(2.89602564102567,-0.439430544027183,
-3.09743052627249));
#14381=CARTESIAN_POINT('Ctrl Pts',(2.91173076923086,-0.282778041871423,
-3.11184033086417));
#14382=CARTESIAN_POINT('Ctrl Pts',(2.92523715029811,-0.148057181168531,
-3.12423273603125));
#14383=CARTESIAN_POINT('Ctrl Pts',(2.93874353136525,-0.0125106239082456,
-3.12790266438722));
#14384=CARTESIAN_POINT('Ctrl Pts',(2.95224991243248,0.122686924247132,-3.12259073825233));
#14385=CARTESIAN_POINT('Ctrl Pts',(2.95444865957043,0.144696167180856,-3.1217259927422));
#14386=CARTESIAN_POINT('Ctrl Pts',(2.95664740670838,0.166696155154839,-3.12062326574181));
#14387=CARTESIAN_POINT('Ctrl Pts',(2.95884615384633,0.1886819155548,-3.11928401449904));
#14388=CARTESIAN_POINT('Ctrl Pts',(2.97455128205139,0.345720976484957,-3.10971806118707));
#14389=CARTESIAN_POINT('Ctrl Pts',(2.99025641025661,0.502004351790296,-3.08808590041721));
#14390=CARTESIAN_POINT('Ctrl Pts',(3.00596153846167,0.655779338422631,-3.05493687313145));
#14391=CARTESIAN_POINT('Ctrl Pts',(3.02166666666689,0.809554325056565,-3.02178784584535));
#14392=CARTESIAN_POINT('Ctrl Pts',(3.03737179487195,0.960836126315138,-2.9771233215876));
#14393=CARTESIAN_POINT('Ctrl Pts',(3.05307692307697,1.10796040920211,-2.9214504428197));
#14394=CARTESIAN_POINT('Ctrl Pts',(3.068782051282,1.25508469208908,-2.86577756405179));
#14395=CARTESIAN_POINT('Ctrl Pts',(3.084487179487,1.39806382918831,-2.79908769904581));
#14396=CARTESIAN_POINT('Ctrl Pts',(3.10019230769217,1.53515081641421,-2.72188982514671));
#14397=CARTESIAN_POINT('Ctrl Pts',(3.10396158983553,1.56805214178305,-2.70336208288368));
#14398=CARTESIAN_POINT('Ctrl Pts',(3.1077308719789,1.60061292833792,-2.68422968792613));
#14399=CARTESIAN_POINT('Ctrl Pts',(3.11150015412227,1.63280801473754,-2.66450051360633));
#14400=CARTESIAN_POINT('Ctrl Pts',(3.12343600018412,1.73475729329959,-2.60202591535358));
#14401=CARTESIAN_POINT('Ctrl Pts',(3.13537184624603,1.8330386668105,-2.53356607404464));
#14402=CARTESIAN_POINT('Ctrl Pts',(3.14730769230783,1.92707055798493,-2.45972435726965));
#14403=CARTESIAN_POINT('Ctrl Pts',(3.163012820513,2.05079726312352,-2.36256378542284));
#14404=CARTESIAN_POINT('Ctrl Pts',(3.178717948718,2.16717972241397,-2.25608242363812));
#14405=CARTESIAN_POINT('Ctrl Pts',(3.19442307692303,2.27501273852753,-2.14155794469054));
#14406=CARTESIAN_POINT('Ctrl Pts',(3.21012820512806,2.3828457546411,-2.02703346574295));
#14407=CARTESIAN_POINT('Ctrl Pts',(3.22583333333311,2.48213900530219,-1.90445476333191));
#14408=CARTESIAN_POINT('Ctrl Pts',(3.24153846153833,2.57165193077396,-1.77508287620843));
#14409=CARTESIAN_POINT('Ctrl Pts',(3.25127559877096,2.62714970373215,-1.69487265426663));
#14410=CARTESIAN_POINT('Ctrl Pts',(3.26101273600365,2.67888797642152,-1.61204808608716));
#14411=CARTESIAN_POINT('Ctrl Pts',(3.27074987323633,2.72655002210233,-1.52694137967767));
#14412=CARTESIAN_POINT('Ctrl Pts',(3.27671786420879,2.75576257724611,-1.47477860910038));
#14413=CARTESIAN_POINT('Ctrl Pts',(3.28268585518124,2.78344401079767,-1.42175865550711));
#14414=CARTESIAN_POINT('Ctrl Pts',(3.28865384615367,2.80956688241491,-1.36798352909411));
#14415=CARTESIAN_POINT('Ctrl Pts',(3.30435897435889,2.87831079468499,-1.22647104047447));
#14416=CARTESIAN_POINT('Ctrl Pts',(3.32006410256394,2.9362584893282,-1.07973927060473));
#14417=CARTESIAN_POINT('Ctrl Pts',(3.33576923076914,2.982977349702,-0.929533639746724));
#14418=CARTESIAN_POINT('Ctrl Pts',(3.35147435897433,3.0296962100758,-0.779328008888721));
#14419=CARTESIAN_POINT('Ctrl Pts',(3.36717948717967,3.06519301000169,-0.625635251226046));
#14420=CARTESIAN_POINT('Ctrl Pts',(3.38288461538483,3.08901983228559,-0.470139769698067));
#14421=CARTESIAN_POINT('Ctrl Pts',(3.39858974359,3.11284665456948,-0.314644288170088));
#14422=CARTESIAN_POINT('Ctrl Pts',(3.414294871795,3.125,-0.157330906751383));
#14423=CARTESIAN_POINT('Ctrl Pts',(3.43,3.125,0.));
#14424=CARTESIAN_POINT('Ctrl Pts',(3.445705128205,3.125,0.157330906751383));
#14425=CARTESIAN_POINT('Ctrl Pts',(3.46141025641,3.11284665456948,0.314644288170091));
#14426=CARTESIAN_POINT('Ctrl Pts',(3.47711538461517,3.08901983228559,0.47013976969807));
#14427=CARTESIAN_POINT('Ctrl Pts',(3.49282051282033,3.06519301000169,0.625635251226049));
#14428=CARTESIAN_POINT('Ctrl Pts',(3.50852564102567,3.0296962100758,0.779328008888722));
#14429=CARTESIAN_POINT('Ctrl Pts',(3.52423076923086,2.982977349702,0.929533639746725));
#14430=CARTESIAN_POINT('Ctrl Pts',(3.53993589743606,2.9362584893282,1.07973927060473));
#14431=CARTESIAN_POINT('Ctrl Pts',(3.55564102564111,2.87831079468499,1.22647104047447));
#14432=CARTESIAN_POINT('Ctrl Pts',(3.57134615384633,2.80956688241491,1.36798352909411));
#14433=CARTESIAN_POINT('Ctrl Pts',(3.57731414481876,2.78344401079767,1.42175865550711));
#14434=CARTESIAN_POINT('Ctrl Pts',(3.58328213579121,2.75576257724611,1.47477860910038));
#14435=CARTESIAN_POINT('Ctrl Pts',(3.58925012676367,2.72655002210233,1.52694137967767));
#14436=CARTESIAN_POINT('Ctrl Pts',(3.59898726399635,2.67888797642152,1.61204808608716));
#14437=CARTESIAN_POINT('Ctrl Pts',(3.60872440122904,2.62714970373215,1.69487265426663));
#14438=CARTESIAN_POINT('Ctrl Pts',(3.61846153846167,2.57165193077395,1.77508287620844));
#14439=CARTESIAN_POINT('Ctrl Pts',(3.63416666666689,2.48213900530219,1.90445476333191));
#14440=CARTESIAN_POINT('Ctrl Pts',(3.64987179487195,2.3828457546411,2.02703346574295));
#14441=CARTESIAN_POINT('Ctrl Pts',(3.66557692307697,2.27501273852753,2.14155794469054));
#14442=CARTESIAN_POINT('Ctrl Pts',(3.681282051282,2.16717972241396,2.25608242363812));
#14443=CARTESIAN_POINT('Ctrl Pts',(3.696987179487,2.05079726312352,2.36256378542284));
#14444=CARTESIAN_POINT('Ctrl Pts',(3.71269230769217,1.92707055798493,2.45972435726965));
#14445=CARTESIAN_POINT('Ctrl Pts',(3.72462815375397,1.8330386668105,2.53356607404464));
#14446=CARTESIAN_POINT('Ctrl Pts',(3.73656399981588,1.73475729329959,2.60202591535358));
#14447=CARTESIAN_POINT('Ctrl Pts',(3.74849984587773,1.63280801473754,2.66450051360633));
#14448=CARTESIAN_POINT('Ctrl Pts',(3.7522691280211,1.60061292833792,2.68422968792613));
#14449=CARTESIAN_POINT('Ctrl Pts',(3.75603841016447,1.56805214178305,2.70336208288368));
#14450=CARTESIAN_POINT('Ctrl Pts',(3.75980769230783,1.53515081641421,2.72188982514671));
#14451=CARTESIAN_POINT('Ctrl Pts',(3.775512820513,1.39806382918831,2.79908769904581));
#14452=CARTESIAN_POINT('Ctrl Pts',(3.791217948718,1.25508469208908,2.86577756405179));
#14453=CARTESIAN_POINT('Ctrl Pts',(3.80692307692303,1.10796040920211,2.92145044281969));
#14454=CARTESIAN_POINT('Ctrl Pts',(3.82262820512805,0.960836126315141,2.9771233215876));
#14455=CARTESIAN_POINT('Ctrl Pts',(3.83833333333311,0.809554325056562,3.02178784584535));
#14456=CARTESIAN_POINT('Ctrl Pts',(3.85403846153833,0.655779338422628,3.05493687313145));
#14457=CARTESIAN_POINT('Ctrl Pts',(3.86974358974339,0.502004351790293,3.08808590041721));
#14458=CARTESIAN_POINT('Ctrl Pts',(3.88544871794861,0.345720976484962,3.10971806118707));
#14459=CARTESIAN_POINT('Ctrl Pts',(3.90115384615367,0.188681915554805,3.11928401449904));
#14460=CARTESIAN_POINT('Ctrl Pts',(3.90335259329162,0.166696155154845,3.12062326574181));
#14461=CARTESIAN_POINT('Ctrl Pts',(3.90555134042957,0.144696167180862,3.1217259927422));
#14462=CARTESIAN_POINT('Ctrl Pts',(3.90775008756752,0.122686924247137,3.12259073825233));
#14463=CARTESIAN_POINT('Ctrl Pts',(3.92125646863475,-0.0125106239082456,
3.12790266438722));
#14464=CARTESIAN_POINT('Ctrl Pts',(3.9347628497019,-0.148057181168534,3.12423273603126));
#14465=CARTESIAN_POINT('Ctrl Pts',(3.94826923076914,-0.282778041871425,
3.11184033086417));
#14466=CARTESIAN_POINT('Ctrl Pts',(3.96397435897433,-0.439430544027182,
3.09743052627249));
#14467=CARTESIAN_POINT('Ctrl Pts',(3.97967948717967,-0.594980979401456,
3.07123183167645));
#14468=CARTESIAN_POINT('Ctrl Pts',(3.99538461538483,-0.747723396432294,
3.03363235324925));
#14469=CARTESIAN_POINT('Ctrl Pts',(4.01108974359,-0.900465813463131,2.99603287482204));
#14470=CARTESIAN_POINT('Ctrl Pts',(4.026794871795,-1.05041416549222,2.94702775592731));
#14471=CARTESIAN_POINT('Ctrl Pts',(4.0425,-1.19582529175154,2.88697719853058));
#14472=CARTESIAN_POINT('Ctrl Pts',(4.05066665861977,-1.27143900290213,2.85575093945237));
#14473=CARTESIAN_POINT('Ctrl Pts',(4.05883331723954,-1.34582560455246,2.82153709650612));
#14474=CARTESIAN_POINT('Ctrl Pts',(4.06699997585933,-1.41872031168613,2.78439538808883));
#14475=CARTESIAN_POINT('Ctrl Pts',(4.07453844544458,-1.48600787178097,2.75011066378684));
#14476=CARTESIAN_POINT('Ctrl Pts',(4.08207691502986,-1.55202420668778,2.71333124947796));
#14477=CARTESIAN_POINT('Ctrl Pts',(4.08961538461517,-1.61660883785066,2.674197927153));
#14478=CARTESIAN_POINT('Ctrl Pts',(4.10532051282033,-1.75116000914844,2.59267025933498));
#14479=CARTESIAN_POINT('Ctrl Pts',(4.12102564102567,-1.87949661326408,2.5009298415257));
#14480=CARTESIAN_POINT('Ctrl Pts',(4.13673076923086,-2.00029920318409,2.40017868230316));
#14481=CARTESIAN_POINT('Ctrl Pts',(4.15243589743605,-2.12110179310409,2.29942752308062));
#14482=CARTESIAN_POINT('Ctrl Pts',(4.16814102564111,-2.23438275356726,2.18965751630222));
#14483=CARTESIAN_POINT('Ctrl Pts',(4.18384615384633,-2.33882800562177,2.07202028766331));
#14484=CARTESIAN_POINT('Ctrl Pts',(4.19798075123882,-2.4328286128156,1.9661469166566));
#14485=CARTESIAN_POINT('Ctrl Pts',(4.21211534863145,-2.5196763173783,1.85388929799372));
#14486=CARTESIAN_POINT('Ctrl Pts',(4.22624994602396,-2.59834253844517,1.7361569781865));
#14487=CARTESIAN_POINT('Ctrl Pts',(4.22782047683653,-2.60708334093589,1.72307544280507));
#14488=CARTESIAN_POINT('Ctrl Pts',(4.2293910076491,-2.61572315428164,1.70992633493316));
#14489=CARTESIAN_POINT('Ctrl Pts',(4.23096153846167,-2.62426134529928,1.69671142476984));
#14490=CARTESIAN_POINT('Ctrl Pts',(4.24666666666689,-2.70964227733817,1.56456383704048));
#14491=CARTESIAN_POINT('Ctrl Pts',(4.26237179487195,-2.78484285491041,1.42586238912421));
#14492=CARTESIAN_POINT('Ctrl Pts',(4.27807692307697,-2.84927329204631,1.28235426733883));
#14493=CARTESIAN_POINT('Ctrl Pts',(4.293782051282,-2.91370372918221,1.13884614555346));
#14494=CARTESIAN_POINT('Ctrl Pts',(4.309487179487,-2.96737444185033,0.990520079795544));
#14495=CARTESIAN_POINT('Ctrl Pts',(4.32519230769217,-3.0097189125242,0.839021679403841));
#14496=CARTESIAN_POINT('Ctrl Pts',(4.34089743589733,-3.05206338319806,0.687523279012144));
#14497=CARTESIAN_POINT('Ctrl Pts',(4.35660256410267,-3.08308231912341,0.532837536272352));
#14498=CARTESIAN_POINT('Ctrl Pts',(4.37230769230783,-3.10216193300488,0.376670614074617));
#14499=CARTESIAN_POINT('Ctrl Pts',(4.37670518255325,-3.10750429091715,0.332943335439869));
#14500=CARTESIAN_POINT('Ctrl Pts',(4.38110267279866,-3.11191034485466,0.289101422213986));
#14501=CARTESIAN_POINT('Ctrl Pts',(4.38550016304406,-3.11536666791583,0.245184674149674));
#14502=CARTESIAN_POINT('Ctrl Pts',(4.39680780100375,-3.12425420322951,0.132257831845052));
#14503=CARTESIAN_POINT('Ctrl Pts',(4.40811543896338,-3.12686097074617,0.0188362390481956));
#14504=CARTESIAN_POINT('Ctrl Pts',(4.41942307692303,-3.12331108802163,-0.0943762077871013));
#14505=CARTESIAN_POINT('Ctrl Pts',(4.43512820512805,-3.11838067165169,-0.251616473021838));
#14506=CARTESIAN_POINT('Ctrl Pts',(4.45083333333311,-3.10157888359858,-0.408464343904398));
#14507=CARTESIAN_POINT('Ctrl Pts',(4.46653846153833,-3.07323267657501,-0.563190821606759));
#14508=CARTESIAN_POINT('Ctrl Pts',(4.48224358974339,-3.04488646955173,-0.717917299307511));
#14509=CARTESIAN_POINT('Ctrl Pts',(4.49794871794861,-3.00499295138217,-0.87053682098386));
#14510=CARTESIAN_POINT('Ctrl Pts',(4.51365384615367,-2.95384328122045,-1.01930854475146));
#14511=CARTESIAN_POINT('Ctrl Pts',(4.52401918038102,-2.9200846630212,-1.11749740512214));
#14512=CARTESIAN_POINT('Ctrl Pts',(4.5343845146083,-2.88141969889172,-1.21401301400872));
#14513=CARTESIAN_POINT('Ctrl Pts',(4.54474984883559,-2.83794741820317,-1.30831167980417));
#14514=CARTESIAN_POINT('Ctrl Pts',(4.55008964281343,-2.8155522867454,-1.35689047491985));
#14515=CARTESIAN_POINT('Ctrl Pts',(4.55542943679128,-2.79188153817257,-1.40488097415943));
#14516=CARTESIAN_POINT('Ctrl Pts',(4.56076923076914,-2.76698261297628,-1.45222443021404));
#14517=CARTESIAN_POINT('Ctrl Pts',(4.57647435897433,-2.69375117108915,-1.59146857523107));
#14518=CARTESIAN_POINT('Ctrl Pts',(4.59217948717967,-2.60990334072498,-1.72510373105075));
#14519=CARTESIAN_POINT('Ctrl Pts',(4.60788461538483,-2.51660034679189,-1.8517492832441));
#14520=CARTESIAN_POINT('Ctrl Pts',(4.62358974359,-2.42329735285879,-1.97839483543744));
#14521=CARTESIAN_POINT('Ctrl Pts',(4.639294871795,-2.32053279801942,-2.09806428789222));
#14522=CARTESIAN_POINT('Ctrl Pts',(4.655,-2.20940661429584,-2.20940720229315));
#14523=CARTESIAN_POINT('Ctrl Pts',(4.670705128205,-2.09828043057227,-2.32075011669408));
#14524=CARTESIAN_POINT('Ctrl Pts',(4.68641025641,-1.97877854529902,-2.42377293936711));
#14525=CARTESIAN_POINT('Ctrl Pts',(4.70211538461517,-1.85206859791098,-2.51703377008662));
#14526=CARTESIAN_POINT('Ctrl Pts',(4.70274359409187,-1.84700016493149,-2.52076422913783));
#14527=CARTESIAN_POINT('Ctrl Pts',(4.70337180356858,-1.84192024452082,-2.52447903878346));
#14528=CARTESIAN_POINT('Ctrl Pts',(4.70400001304529,-1.83682891341399,-2.52817810742184));
#14529=CARTESIAN_POINT('Ctrl Pts',(4.71907693177376,-1.71463784791186,-2.61695511461419));
#14530=CARTESIAN_POINT('Ctrl Pts',(4.73415385050237,-1.58587336592168,-2.69666335686228));
#14531=CARTESIAN_POINT('Ctrl Pts',(4.74923076923086,-1.45207966320917,-2.76670577109897));
#14532=CARTESIAN_POINT('Ctrl Pts',(4.76493589743605,-1.31271118268685,-2.83966664030563));
#14533=CARTESIAN_POINT('Ctrl Pts',(4.78064102564111,-1.16787561222373,-2.90215131904986));
#14534=CARTESIAN_POINT('Ctrl Pts',(4.79634615384633,-1.01920094228016,-2.95353305961267));
#14535=CARTESIAN_POINT('Ctrl Pts',(4.81205128205139,-0.870526272338138,
-3.00491480017493));
#14536=CARTESIAN_POINT('Ctrl Pts',(4.82775641025661,-0.717997900620678,
-3.04519632262622));
#14537=CARTESIAN_POINT('Ctrl Pts',(4.84346153846167,-0.563276981103821,
-3.07370359533634));
#14538=CARTESIAN_POINT('Ctrl Pts',(4.85005772273745,-0.498293895125397,
-3.08567670510919));
#14539=CARTESIAN_POINT('Ctrl Pts',(4.8566539070132,-0.432925228768243,-3.09557218825737));
#14540=CARTESIAN_POINT('Ctrl Pts',(4.86325009128893,-0.367304367055667,
-3.1033389279845));
#14541=CARTESIAN_POINT('Ctrl Pts',(4.87235903521831,-0.276685802602259,
-3.11406434039434));
#14542=CARTESIAN_POINT('Ctrl Pts',(4.88146797914764,-0.185586340671027,
-3.12072993099726));
#14543=CARTESIAN_POINT('Ctrl Pts',(4.89057692307697,-0.0943789619765783,
-3.12338542308761));
#14544=CARTESIAN_POINT('Ctrl Pts',(4.906282051282,0.0628756645481118,-3.12796387302098));
#14545=CARTESIAN_POINT('Ctrl Pts',(4.921987179487,0.220455320082457,-3.12062582859596));
#14546=CARTESIAN_POINT('Ctrl Pts',(4.93769230769217,0.376606556598298,-3.10163498008567));
#14547=CARTESIAN_POINT('Ctrl Pts',(4.95339743589733,0.53275779311414,-3.08264413157538));
#14548=CARTESIAN_POINT('Ctrl Pts',(4.96910256410267,0.687495327956871,-3.0519995880578));
#14549=CARTESIAN_POINT('Ctrl Pts',(4.98480769230783,0.839080192893056,-3.00992620370386));
#14550=CARTESIAN_POINT('Ctrl Pts',(4.99737175038973,0.960347655502346,-2.97626761538679));
#14551=CARTESIAN_POINT('Ctrl Pts',(5.00993580847151,1.07960443666828,-2.93528882778825));
#14552=CARTESIAN_POINT('Ctrl Pts',(5.02249986655329,1.19588572614116,-2.887123539098));
#14553=CARTESIAN_POINT('Ctrl Pts',(5.02564093667654,1.22495656311742,-2.8750820037678));
#14554=CARTESIAN_POINT('Ctrl Pts',(5.02878200679978,1.25384145182002,-2.86259139598291));
#14555=CARTESIAN_POINT('Ctrl Pts',(5.03192307692303,1.28252819003516,-2.84966078036119));
#14556=CARTESIAN_POINT('Ctrl Pts',(5.04762820512805,1.42595984987577,-2.78500861783667));
#14557=CARTESIAN_POINT('Ctrl Pts',(5.06333333333311,1.56441436952739,-2.70936700040773));
#14558=CARTESIAN_POINT('Ctrl Pts',(5.07903846153833,1.69644712969505,-2.62385329049029));
#14559=CARTESIAN_POINT('Ctrl Pts',(5.09474358974339,1.82847988986133,-2.53833958057375));
#14560=CARTESIAN_POINT('Ctrl Pts',(5.11044871794861,1.95410534229508,-2.44294922198321));
#14561=CARTESIAN_POINT('Ctrl Pts',(5.12615384615367,2.07193616153302,-2.33873186210924));
#14562=CARTESIAN_POINT('Ctrl Pts',(5.14185897435889,2.18976698077217,-2.23451450223419));
#14563=CARTESIAN_POINT('Ctrl Pts',(5.15756410256395,2.29981131668746,-2.12145732421479));
#14564=CARTESIAN_POINT('Ctrl Pts',(5.17326923076914,2.40059929676421,-2.00064999697507));
#14565=CARTESIAN_POINT('Ctrl Pts',(5.17609619372183,2.4187413890815,-1.97890437133877));
#14566=CARTESIAN_POINT('Ctrl Pts',(5.17892315667452,2.43658301180573,-1.95690831774611));
#14567=CARTESIAN_POINT('Ctrl Pts',(5.18175011962722,2.45411540900217,-1.93466859159333));
#14568=CARTESIAN_POINT('Ctrl Pts',(5.19462828487976,2.53398384454479,-1.83335602635671));
#14569=CARTESIAN_POINT('Ctrl Pts',(5.20750645013235,2.60743359059156,-1.72698578057499));
#14570=CARTESIAN_POINT('Ctrl Pts',(5.22038461538483,2.67404531641152,-1.61651716219696));
#14571=CARTESIAN_POINT('Ctrl Pts',(5.23608974359,2.75527937991824,-1.48179891776846));
#14572=CARTESIAN_POINT('Ctrl Pts',(5.251794871795,2.82635571584921,-1.34097710458914));
#14573=CARTESIAN_POINT('Ctrl Pts',(5.2675,2.886585772757,-1.1956628320182));
#14574=CARTESIAN_POINT('Ctrl Pts',(5.283205128205,2.94681582966478,-1.05034855944727));
#14575=CARTESIAN_POINT('Ctrl Pts',(5.29891025641,2.99620426616756,-0.900527828411028));
#14576=CARTESIAN_POINT('Ctrl Pts',(5.31461538461517,3.03402009771089,-0.747818590164115));
#14577=CARTESIAN_POINT('Ctrl Pts',(5.323410232868,3.05519690668903,-0.662301645657758));
#14578=CARTESIAN_POINT('Ctrl Pts',(5.33220508112087,3.07274362189333,-0.575877627491407));
#14579=CARTESIAN_POINT('Ctrl Pts',(5.34099992937375,3.0865260643595,-0.488857703250828));
#14580=CARTESIAN_POINT('Ctrl Pts',(5.34791020932613,3.09735519217733,-0.420484489677707));
#14581=CARTESIAN_POINT('Ctrl Pts',(5.35482048927851,3.1058605533367,-0.351743453374755));
#14582=CARTESIAN_POINT('Ctrl Pts',(5.36173076923086,3.11205714799649,-0.282798238157759));
#14583=CARTESIAN_POINT('Ctrl Pts',(5.37743589743605,3.12614026969903,-0.126105101036853));
#14584=CARTESIAN_POINT('Ctrl Pts',(5.39314102564111,3.12830002883755,0.0316368087400967));
#14585=CARTESIAN_POINT('Ctrl Pts',(5.40884615384633,3.11873422241136,0.188648419771248));
#14586=CARTESIAN_POINT('Ctrl Pts',(5.42455128205139,3.10916841598526,0.345660030800768));
#14587=CARTESIAN_POINT('Ctrl Pts',(5.44025641025661,3.08787818772652,0.501956134080478));
#14588=CARTESIAN_POINT('Ctrl Pts',(5.45596153846167,3.05502438429764,0.655798952750868));
#14589=CARTESIAN_POINT('Ctrl Pts',(5.47072435081943,3.02414182613405,0.80041112241712));
#14590=CARTESIAN_POINT('Ctrl Pts',(5.48548716317704,2.98303392179022,0.942866889012676));
#14591=CARTESIAN_POINT('Ctrl Pts',(5.50024997553463,2.93184792475783,1.08161580336684));
#14592=CARTESIAN_POINT('Ctrl Pts',(5.50119229138207,2.92858070337733,1.09047219858784));
#14593=CARTESIAN_POINT('Ctrl Pts',(5.50213460722953,2.92527242968113,1.09931349244539));
#14594=CARTESIAN_POINT('Ctrl Pts',(5.50307692307697,2.92192333127633,1.10813935100346));
#14595=CARTESIAN_POINT('Ctrl Pts',(5.518782051282,2.8661055076018,1.25523572060092));
#14596=CARTESIAN_POINT('Ctrl Pts',(5.534487179487,2.79895807188958,1.3980126906426));
#14597=CARTESIAN_POINT('Ctrl Pts',(5.55019230769217,2.72154967470353,1.53495847225753));
#14598=CARTESIAN_POINT('Ctrl Pts',(5.56589743589733,2.64414127751749,1.67190425387245));
#14599=CARTESIAN_POINT('Ctrl Pts',(5.58160256410267,2.55646931412381,1.80303404218782));
#14600=CARTESIAN_POINT('Ctrl Pts',(5.59730769230783,2.45953351178131,1.92692186650602));
#14601=CARTESIAN_POINT('Ctrl Pts',(5.613012820513,2.3625977094388,2.05080969082422));
#14602=CARTESIAN_POINT('Ctrl Pts',(5.628717948718,2.25638664196914,2.16746520831446));
#14603=CARTESIAN_POINT('Ctrl Pts',(5.64442307692303,2.14191592065938,2.27539299236912));
#14604=CARTESIAN_POINT('Ctrl Pts',(5.64944877282191,2.10528488988284,2.30993026036321));
#14605=CARTESIAN_POINT('Ctrl Pts',(5.65447446872079,2.0678091870461,2.34357256496936));
#14606=CARTESIAN_POINT('Ctrl Pts',(5.65950016461967,2.02952515103173,2.37626864249984));
#14607=CARTESIAN_POINT('Ctrl Pts',(5.67017959692584,1.94817288076942,2.44574669164748));
#14608=CARTESIAN_POINT('Ctrl Pts',(5.68085902923205,1.86317013579029,2.51095134091135));
#14609=CARTESIAN_POINT('Ctrl Pts',(5.69153846153833,1.7750601494579,2.57161807835228));
#14610=CARTESIAN_POINT('Ctrl Pts',(5.70724358974339,1.64548597436975,2.66083432711599));
#14611=CARTESIAN_POINT('Ctrl Pts',(5.72294871794861,1.509186930649,2.74024633660057));
#14612=CARTESIAN_POINT('Ctrl Pts',(5.73865384615367,1.36775803719504,2.80910392412142));
#14613=CARTESIAN_POINT('Ctrl Pts',(5.75435897435889,1.22632914373961,2.87796151164299));
#14614=CARTESIAN_POINT('Ctrl Pts',(5.77006410256395,1.07975715593558,2.9362712759061));
#14615=CARTESIAN_POINT('Ctrl Pts',(5.78576923076914,0.929617596829541,2.98324879794393));
#14616=CARTESIAN_POINT('Ctrl Pts',(5.7967627558717,0.82452052341797,3.01613287001461));
#14617=CARTESIAN_POINT('Ctrl Pts',(5.80775628097433,0.717669381189646,3.04346332885533));
#14618=CARTESIAN_POINT('Ctrl Pts',(5.81874980607692,0.609657256300376,3.06495400126008));
#14619=CARTESIAN_POINT('Ctrl Pts',(5.82346140917957,0.563365438343646,3.07416446995282));
#14620=CARTESIAN_POINT('Ctrl Pts',(5.82817301228221,0.516860431844721,3.08230245321972));
#14621=CARTESIAN_POINT('Ctrl Pts',(5.83288461538483,0.470193579471047,3.08937038670253));
#14622=CARTESIAN_POINT('Ctrl Pts',(5.84858974359,0.31463953905291,3.112929841749));
#14623=CARTESIAN_POINT('Ctrl Pts',(5.864294871795,0.157306535044493,3.12459764304402));
#14624=CARTESIAN_POINT('Ctrl Pts',(5.88,3.21695909424879E-7,3.12449703095644));
#14625=CARTESIAN_POINT('Ctrl Pts',(1.170978862952,-0.9656781074217,-2.972051613422));
#14626=CARTESIAN_POINT('Ctrl Pts',(1.224062196285,-0.4599252670358,-3.136380672689));
#14627=CARTESIAN_POINT('Ctrl Pts',(1.330228862952,0.6366272854614,-3.200971110614));
#14628=CARTESIAN_POINT('Ctrl Pts',(1.489478862952,2.119635939241,-2.481754111378));
#14629=CARTESIAN_POINT('Ctrl Pts',(1.648728862952,3.061979863765,-1.129624298873));
#14630=CARTESIAN_POINT('Ctrl Pts',(1.807978862952,3.223532154246,0.5105564866689));
#14631=CARTESIAN_POINT('Ctrl Pts',(1.967228862952,2.563047905408,2.020544571702));
#14632=CARTESIAN_POINT('Ctrl Pts',(2.126478862952,1.248968678135,3.015276776083));
#14633=CARTESIAN_POINT('Ctrl Pts',(2.285728862952,-0.383608261101,3.241089558554));
#14634=CARTESIAN_POINT('Ctrl Pts',(2.444978862952,-1.918361836065,2.640398557608));
#14635=CARTESIAN_POINT('Ctrl Pts',(2.604228862952,-2.963917875123,1.366384855545));
#14636=CARTESIAN_POINT('Ctrl Pts',(2.763478862952,-3.253651172662,-0.256067900963));
#14637=CARTESIAN_POINT('Ctrl Pts',(2.922728862952,-2.713677441724,-1.813221296591));
#14638=CARTESIAN_POINT('Ctrl Pts',(3.081978862952,-1.481694291113,-2.907988781792));
#14639=CARTESIAN_POINT('Ctrl Pts',(3.241228862952,0.1281327360592,-3.261195904774));
#14640=CARTESIAN_POINT('Ctrl Pts',(3.400478862952,1.705284892359,-2.782772028626));
#14641=CARTESIAN_POINT('Ctrl Pts',(3.559728862952,2.84757578293,-1.59471906236));
#14642=CARTESIAN_POINT('Ctrl Pts',(3.718978862952,3.263712108535,0.));
#14643=CARTESIAN_POINT('Ctrl Pts',(3.878228862952,2.84757578293,1.59471906236));
#14644=CARTESIAN_POINT('Ctrl Pts',(4.037478862952,1.705284892359,2.782772028626));
#14645=CARTESIAN_POINT('Ctrl Pts',(4.196728862952,0.1281327360592,3.261195904774));
#14646=CARTESIAN_POINT('Ctrl Pts',(4.355978862952,-1.481694291113,2.907988781792));
#14647=CARTESIAN_POINT('Ctrl Pts',(4.515228862952,-2.713677441724,1.813221296591));
#14648=CARTESIAN_POINT('Ctrl Pts',(4.674478862952,-3.253651172662,0.256067900963));
#14649=CARTESIAN_POINT('Ctrl Pts',(4.833728862952,-2.963917875123,-1.366384855545));
#14650=CARTESIAN_POINT('Ctrl Pts',(4.992978862952,-1.918361836065,-2.640398557608));
#14651=CARTESIAN_POINT('Ctrl Pts',(5.152228862952,-0.383608261101,-3.241089558554));
#14652=CARTESIAN_POINT('Ctrl Pts',(5.311478862952,1.248968678135,-3.015276776083));
#14653=CARTESIAN_POINT('Ctrl Pts',(5.470728862952,2.563047905408,-2.020544571702));
#14654=CARTESIAN_POINT('Ctrl Pts',(5.629978862952,3.223532154246,-0.510556486669));
#14655=CARTESIAN_POINT('Ctrl Pts',(5.789228862952,3.061979863765,1.129624298873));
#14656=CARTESIAN_POINT('Ctrl Pts',(5.948478862952,2.119635939241,2.481754111378));
#14657=CARTESIAN_POINT('Ctrl Pts',(6.107728862952,0.6366272854614,3.200971110614));
#14658=CARTESIAN_POINT('Ctrl Pts',(6.213895529618,-0.4599252670358,3.136380672689));
#14659=CARTESIAN_POINT('Ctrl Pts',(6.266978862952,-0.9656781074217,2.972051613422));
#14660=CARTESIAN_POINT('Ctrl Pts',(1.059992954317,-0.9656781074217,-2.972051613422));
#14661=CARTESIAN_POINT('Ctrl Pts',(1.113076287651,-0.4599252670358,-3.136380672689));
#14662=CARTESIAN_POINT('Ctrl Pts',(1.219242954317,0.6366272854614,-3.200971110614));
#14663=CARTESIAN_POINT('Ctrl Pts',(1.378492954317,2.119635939241,-2.481754111378));
#14664=CARTESIAN_POINT('Ctrl Pts',(1.537742954317,3.061979863765,-1.129624298873));
#14665=CARTESIAN_POINT('Ctrl Pts',(1.696992954317,3.223532154246,0.5105564866689));
#14666=CARTESIAN_POINT('Ctrl Pts',(1.856242954317,2.563047905408,2.020544571702));
#14667=CARTESIAN_POINT('Ctrl Pts',(2.015492954317,1.248968678135,3.015276776083));
#14668=CARTESIAN_POINT('Ctrl Pts',(2.174742954317,-0.383608261101,3.241089558554));
#14669=CARTESIAN_POINT('Ctrl Pts',(2.333992954317,-1.918361836065,2.640398557608));
#14670=CARTESIAN_POINT('Ctrl Pts',(2.493242954317,-2.963917875123,1.366384855545));
#14671=CARTESIAN_POINT('Ctrl Pts',(2.652492954317,-3.253651172662,-0.256067900963));
#14672=CARTESIAN_POINT('Ctrl Pts',(2.811742954317,-2.713677441724,-1.813221296591));
#14673=CARTESIAN_POINT('Ctrl Pts',(2.970992954317,-1.481694291113,-2.907988781792));
#14674=CARTESIAN_POINT('Ctrl Pts',(3.130242954317,0.1281327360592,-3.261195904774));
#14675=CARTESIAN_POINT('Ctrl Pts',(3.289492954317,1.705284892359,-2.782772028626));
#14676=CARTESIAN_POINT('Ctrl Pts',(3.448742954317,2.84757578293,-1.59471906236));
#14677=CARTESIAN_POINT('Ctrl Pts',(3.607992954317,3.263712108535,0.));
#14678=CARTESIAN_POINT('Ctrl Pts',(3.767242954317,2.84757578293,1.59471906236));
#14679=CARTESIAN_POINT('Ctrl Pts',(3.926492954317,1.705284892359,2.782772028626));
#14680=CARTESIAN_POINT('Ctrl Pts',(4.085742954317,0.1281327360592,3.261195904774));
#14681=CARTESIAN_POINT('Ctrl Pts',(4.244992954317,-1.481694291113,2.907988781792));
#14682=CARTESIAN_POINT('Ctrl Pts',(4.404242954317,-2.713677441724,1.813221296591));
#14683=CARTESIAN_POINT('Ctrl Pts',(4.563492954317,-3.253651172662,0.256067900963));
#14684=CARTESIAN_POINT('Ctrl Pts',(4.722742954317,-2.963917875123,-1.366384855545));
#14685=CARTESIAN_POINT('Ctrl Pts',(4.881992954317,-1.918361836065,-2.640398557608));
#14686=CARTESIAN_POINT('Ctrl Pts',(5.041242954317,-0.383608261101,-3.241089558554));
#14687=CARTESIAN_POINT('Ctrl Pts',(5.200492954317,1.248968678135,-3.015276776083));
#14688=CARTESIAN_POINT('Ctrl Pts',(5.359742954317,2.563047905408,-2.020544571702));
#14689=CARTESIAN_POINT('Ctrl Pts',(5.518992954317,3.223532154246,-0.510556486669));
#14690=CARTESIAN_POINT('Ctrl Pts',(5.678242954317,3.061979863765,1.129624298873));
#14691=CARTESIAN_POINT('Ctrl Pts',(5.837492954317,2.119635939241,2.481754111378));
#14692=CARTESIAN_POINT('Ctrl Pts',(5.996742954317,0.6366272854614,3.200971110614));
#14693=CARTESIAN_POINT('Ctrl Pts',(6.102909620984,-0.4599252670358,3.136380672689));
#14694=CARTESIAN_POINT('Ctrl Pts',(6.155992954317,-0.9656781074217,2.972051613422));
#14695=CARTESIAN_POINT('Ctrl Pts',(0.9490070456828,-0.9656781074217,-2.972051613422));
#14696=CARTESIAN_POINT('Ctrl Pts',(1.002090379016,-0.4599252670358,-3.136380672689));
#14697=CARTESIAN_POINT('Ctrl Pts',(1.108257045683,0.6366272854614,-3.200971110614));
#14698=CARTESIAN_POINT('Ctrl Pts',(1.267507045683,2.119635939241,-2.481754111378));
#14699=CARTESIAN_POINT('Ctrl Pts',(1.426757045683,3.061979863765,-1.129624298873));
#14700=CARTESIAN_POINT('Ctrl Pts',(1.586007045683,3.223532154246,0.5105564866689));
#14701=CARTESIAN_POINT('Ctrl Pts',(1.745257045683,2.563047905408,2.020544571702));
#14702=CARTESIAN_POINT('Ctrl Pts',(1.904507045683,1.248968678135,3.015276776083));
#14703=CARTESIAN_POINT('Ctrl Pts',(2.063757045683,-0.383608261101,3.241089558554));
#14704=CARTESIAN_POINT('Ctrl Pts',(2.223007045683,-1.918361836065,2.640398557608));
#14705=CARTESIAN_POINT('Ctrl Pts',(2.382257045683,-2.963917875123,1.366384855545));
#14706=CARTESIAN_POINT('Ctrl Pts',(2.541507045683,-3.253651172662,-0.256067900963));
#14707=CARTESIAN_POINT('Ctrl Pts',(2.700757045683,-2.713677441724,-1.813221296591));
#14708=CARTESIAN_POINT('Ctrl Pts',(2.860007045683,-1.481694291113,-2.907988781792));
#14709=CARTESIAN_POINT('Ctrl Pts',(3.019257045683,0.1281327360592,-3.261195904774));
#14710=CARTESIAN_POINT('Ctrl Pts',(3.178507045683,1.705284892359,-2.782772028626));
#14711=CARTESIAN_POINT('Ctrl Pts',(3.337757045683,2.84757578293,-1.59471906236));
#14712=CARTESIAN_POINT('Ctrl Pts',(3.497007045683,3.263712108535,0.));
#14713=CARTESIAN_POINT('Ctrl Pts',(3.656257045683,2.84757578293,1.59471906236));
#14714=CARTESIAN_POINT('Ctrl Pts',(3.815507045683,1.705284892359,2.782772028626));
#14715=CARTESIAN_POINT('Ctrl Pts',(3.974757045683,0.1281327360592,3.261195904774));
#14716=CARTESIAN_POINT('Ctrl Pts',(4.134007045683,-1.481694291113,2.907988781792));
#14717=CARTESIAN_POINT('Ctrl Pts',(4.293257045683,-2.713677441724,1.813221296591));
#14718=CARTESIAN_POINT('Ctrl Pts',(4.452507045683,-3.253651172662,0.256067900963));
#14719=CARTESIAN_POINT('Ctrl Pts',(4.611757045683,-2.963917875123,-1.366384855545));
#14720=CARTESIAN_POINT('Ctrl Pts',(4.771007045683,-1.918361836065,-2.640398557608));
#14721=CARTESIAN_POINT('Ctrl Pts',(4.930257045683,-0.383608261101,-3.241089558554));
#14722=CARTESIAN_POINT('Ctrl Pts',(5.089507045683,1.248968678135,-3.015276776083));
#14723=CARTESIAN_POINT('Ctrl Pts',(5.248757045683,2.563047905408,-2.020544571702));
#14724=CARTESIAN_POINT('Ctrl Pts',(5.408007045683,3.223532154246,-0.510556486669));
#14725=CARTESIAN_POINT('Ctrl Pts',(5.567257045683,3.061979863765,1.129624298873));
#14726=CARTESIAN_POINT('Ctrl Pts',(5.726507045683,2.119635939241,2.481754111378));
#14727=CARTESIAN_POINT('Ctrl Pts',(5.885757045683,0.6366272854614,3.200971110614));
#14728=CARTESIAN_POINT('Ctrl Pts',(5.991923712349,-0.4599252670358,3.136380672689));
#14729=CARTESIAN_POINT('Ctrl Pts',(6.045007045683,-0.9656781074217,2.972051613422));
#14730=CARTESIAN_POINT('Ctrl Pts',(0.8380211370484,-0.9656781074217,-2.972051613422));
#14731=CARTESIAN_POINT('Ctrl Pts',(0.8911044703817,-0.4599252670358,-3.136380672689));
#14732=CARTESIAN_POINT('Ctrl Pts',(0.9972711370484,0.6366272854614,-3.200971110614));
#14733=CARTESIAN_POINT('Ctrl Pts',(1.156521137048,2.119635939241,-2.481754111378));
#14734=CARTESIAN_POINT('Ctrl Pts',(1.315771137048,3.061979863765,-1.129624298873));
#14735=CARTESIAN_POINT('Ctrl Pts',(1.475021137048,3.223532154246,0.5105564866689));
#14736=CARTESIAN_POINT('Ctrl Pts',(1.634271137048,2.563047905408,2.020544571702));
#14737=CARTESIAN_POINT('Ctrl Pts',(1.793521137048,1.248968678135,3.015276776083));
#14738=CARTESIAN_POINT('Ctrl Pts',(1.952771137048,-0.383608261101,3.241089558554));
#14739=CARTESIAN_POINT('Ctrl Pts',(2.112021137048,-1.918361836065,2.640398557608));
#14740=CARTESIAN_POINT('Ctrl Pts',(2.271271137048,-2.963917875123,1.366384855545));
#14741=CARTESIAN_POINT('Ctrl Pts',(2.430521137048,-3.253651172662,-0.256067900963));
#14742=CARTESIAN_POINT('Ctrl Pts',(2.589771137048,-2.713677441724,-1.813221296591));
#14743=CARTESIAN_POINT('Ctrl Pts',(2.749021137048,-1.481694291113,-2.907988781792));
#14744=CARTESIAN_POINT('Ctrl Pts',(2.908271137048,0.1281327360592,-3.261195904774));
#14745=CARTESIAN_POINT('Ctrl Pts',(3.067521137048,1.705284892359,-2.782772028626));
#14746=CARTESIAN_POINT('Ctrl Pts',(3.226771137048,2.84757578293,-1.59471906236));
#14747=CARTESIAN_POINT('Ctrl Pts',(3.386021137048,3.263712108535,0.));
#14748=CARTESIAN_POINT('Ctrl Pts',(3.545271137048,2.84757578293,1.59471906236));
#14749=CARTESIAN_POINT('Ctrl Pts',(3.704521137048,1.705284892359,2.782772028626));
#14750=CARTESIAN_POINT('Ctrl Pts',(3.863771137048,0.1281327360592,3.261195904774));
#14751=CARTESIAN_POINT('Ctrl Pts',(4.023021137048,-1.481694291113,2.907988781792));
#14752=CARTESIAN_POINT('Ctrl Pts',(4.182271137048,-2.713677441724,1.813221296591));
#14753=CARTESIAN_POINT('Ctrl Pts',(4.341521137048,-3.253651172662,0.256067900963));
#14754=CARTESIAN_POINT('Ctrl Pts',(4.500771137048,-2.963917875123,-1.366384855545));
#14755=CARTESIAN_POINT('Ctrl Pts',(4.660021137048,-1.918361836065,-2.640398557608));
#14756=CARTESIAN_POINT('Ctrl Pts',(4.819271137048,-0.383608261101,-3.241089558554));
#14757=CARTESIAN_POINT('Ctrl Pts',(4.978521137048,1.248968678135,-3.015276776083));
#14758=CARTESIAN_POINT('Ctrl Pts',(5.137771137048,2.563047905408,-2.020544571702));
#14759=CARTESIAN_POINT('Ctrl Pts',(5.297021137048,3.223532154246,-0.510556486669));
#14760=CARTESIAN_POINT('Ctrl Pts',(5.456271137048,3.061979863765,1.129624298873));
#14761=CARTESIAN_POINT('Ctrl Pts',(5.615521137048,2.119635939241,2.481754111378));
#14762=CARTESIAN_POINT('Ctrl Pts',(5.774771137048,0.6366272854614,3.200971110614));
#14763=CARTESIAN_POINT('Ctrl Pts',(5.880937803715,-0.4599252670358,3.136380672689));
#14764=CARTESIAN_POINT('Ctrl Pts',(5.934021137048,-0.9656781074217,2.972051613422));
#14765=CARTESIAN_POINT('',(6.125,0.,3.125));
#14766=CARTESIAN_POINT('Ctrl Pts',(6.070978862952,0.9656781074217,2.972051613422));
#14767=CARTESIAN_POINT('Ctrl Pts',(6.124062196285,0.4599252670358,3.136380672689));
#14768=CARTESIAN_POINT('Ctrl Pts',(6.230228862952,-0.6366272854614,3.200971110614));
#14769=CARTESIAN_POINT('Ctrl Pts',(6.389478862952,-2.119635939241,2.481754111378));
#14770=CARTESIAN_POINT('Ctrl Pts',(6.548728862952,-3.061979863765,1.129624298873));
#14771=CARTESIAN_POINT('Ctrl Pts',(6.707978862952,-3.223532154246,-0.5105564866689));
#14772=CARTESIAN_POINT('Ctrl Pts',(6.867228862952,-2.563047905408,-2.020544571702));
#14773=CARTESIAN_POINT('Ctrl Pts',(7.026478862952,-1.248968678135,-3.015276776083));
#14774=CARTESIAN_POINT('Ctrl Pts',(7.185728862952,0.383608261101,-3.241089558554));
#14775=CARTESIAN_POINT('Ctrl Pts',(7.344978862952,1.918361836065,-2.640398557608));
#14776=CARTESIAN_POINT('Ctrl Pts',(7.504228862952,2.963917875123,-1.366384855545));
#14777=CARTESIAN_POINT('Ctrl Pts',(7.663478862952,3.253651172662,0.256067900963));
#14778=CARTESIAN_POINT('Ctrl Pts',(7.822728862952,2.713677441724,1.813221296591));
#14779=CARTESIAN_POINT('Ctrl Pts',(7.981978862952,1.481694291113,2.907988781792));
#14780=CARTESIAN_POINT('Ctrl Pts',(8.141228862952,-0.1281327360592,3.261195904774));
#14781=CARTESIAN_POINT('Ctrl Pts',(8.300478862952,-1.705284892359,2.782772028626));
#14782=CARTESIAN_POINT('Ctrl Pts',(8.459728862952,-2.84757578293,1.59471906236));
#14783=CARTESIAN_POINT('Ctrl Pts',(8.618978862952,-3.263712108535,0.));
#14784=CARTESIAN_POINT('Ctrl Pts',(8.778228862952,-2.84757578293,-1.59471906236));
#14785=CARTESIAN_POINT('Ctrl Pts',(8.937478862952,-1.705284892359,-2.782772028626));
#14786=CARTESIAN_POINT('Ctrl Pts',(9.096728862952,-0.1281327360592,-3.261195904774));
#14787=CARTESIAN_POINT('Ctrl Pts',(9.255978862952,1.481694291113,-2.907988781792));
#14788=CARTESIAN_POINT('Ctrl Pts',(9.415228862952,2.713677441724,-1.813221296591));
#14789=CARTESIAN_POINT('Ctrl Pts',(9.574478862952,3.253651172662,-0.256067900963));
#14790=CARTESIAN_POINT('Ctrl Pts',(9.733728862952,2.963917875123,1.366384855545));
#14791=CARTESIAN_POINT('Ctrl Pts',(9.892978862952,1.918361836065,2.640398557608));
#14792=CARTESIAN_POINT('Ctrl Pts',(10.05222886295,0.383608261101,3.241089558554));
#14793=CARTESIAN_POINT('Ctrl Pts',(10.21147886295,-1.248968678135,3.015276776083));
#14794=CARTESIAN_POINT('Ctrl Pts',(10.37072886295,-2.563047905408,2.020544571702));
#14795=CARTESIAN_POINT('Ctrl Pts',(10.52997886295,-3.223532154246,0.5105564866689));
#14796=CARTESIAN_POINT('Ctrl Pts',(10.68922886295,-3.061979863765,-1.129624298873));
#14797=CARTESIAN_POINT('Ctrl Pts',(10.84847886295,-2.119635939241,-2.481754111378));
#14798=CARTESIAN_POINT('Ctrl Pts',(11.00772886295,-0.6366272854614,-3.200971110614));
#14799=CARTESIAN_POINT('Ctrl Pts',(11.11389552962,0.4599252670358,-3.136380672689));
#14800=CARTESIAN_POINT('Ctrl Pts',(11.16697886295,0.9656781074217,-2.972051613422));
#14801=CARTESIAN_POINT('Ctrl Pts',(5.959992954317,0.9656781074217,2.972051613422));
#14802=CARTESIAN_POINT('Ctrl Pts',(6.013076287651,0.4599252670358,3.136380672689));
#14803=CARTESIAN_POINT('Ctrl Pts',(6.119242954317,-0.6366272854614,3.200971110614));
#14804=CARTESIAN_POINT('Ctrl Pts',(6.278492954317,-2.119635939241,2.481754111378));
#14805=CARTESIAN_POINT('Ctrl Pts',(6.437742954317,-3.061979863765,1.129624298873));
#14806=CARTESIAN_POINT('Ctrl Pts',(6.596992954317,-3.223532154246,-0.5105564866689));
#14807=CARTESIAN_POINT('Ctrl Pts',(6.756242954317,-2.563047905408,-2.020544571702));
#14808=CARTESIAN_POINT('Ctrl Pts',(6.915492954317,-1.248968678135,-3.015276776083));
#14809=CARTESIAN_POINT('Ctrl Pts',(7.074742954317,0.383608261101,-3.241089558554));
#14810=CARTESIAN_POINT('Ctrl Pts',(7.233992954317,1.918361836065,-2.640398557608));
#14811=CARTESIAN_POINT('Ctrl Pts',(7.393242954317,2.963917875123,-1.366384855545));
#14812=CARTESIAN_POINT('Ctrl Pts',(7.552492954317,3.253651172662,0.256067900963));
#14813=CARTESIAN_POINT('Ctrl Pts',(7.711742954317,2.713677441724,1.813221296591));
#14814=CARTESIAN_POINT('Ctrl Pts',(7.870992954317,1.481694291113,2.907988781792));
#14815=CARTESIAN_POINT('Ctrl Pts',(8.030242954317,-0.1281327360592,3.261195904774));
#14816=CARTESIAN_POINT('Ctrl Pts',(8.189492954317,-1.705284892359,2.782772028626));
#14817=CARTESIAN_POINT('Ctrl Pts',(8.348742954317,-2.84757578293,1.59471906236));
#14818=CARTESIAN_POINT('Ctrl Pts',(8.507992954317,-3.263712108535,0.));
#14819=CARTESIAN_POINT('Ctrl Pts',(8.667242954317,-2.84757578293,-1.59471906236));
#14820=CARTESIAN_POINT('Ctrl Pts',(8.826492954317,-1.705284892359,-2.782772028626));
#14821=CARTESIAN_POINT('Ctrl Pts',(8.985742954317,-0.1281327360592,-3.261195904774));
#14822=CARTESIAN_POINT('Ctrl Pts',(9.144992954317,1.481694291113,-2.907988781792));
#14823=CARTESIAN_POINT('Ctrl Pts',(9.304242954317,2.713677441724,-1.813221296591));
#14824=CARTESIAN_POINT('Ctrl Pts',(9.463492954317,3.253651172662,-0.256067900963));
#14825=CARTESIAN_POINT('Ctrl Pts',(9.622742954317,2.963917875123,1.366384855545));
#14826=CARTESIAN_POINT('Ctrl Pts',(9.781992954317,1.918361836065,2.640398557608));
#14827=CARTESIAN_POINT('Ctrl Pts',(9.941242954317,0.383608261101,3.241089558554));
#14828=CARTESIAN_POINT('Ctrl Pts',(10.10049295432,-1.248968678135,3.015276776083));
#14829=CARTESIAN_POINT('Ctrl Pts',(10.25974295432,-2.563047905408,2.020544571702));
#14830=CARTESIAN_POINT('Ctrl Pts',(10.41899295432,-3.223532154246,0.5105564866689));
#14831=CARTESIAN_POINT('Ctrl Pts',(10.57824295432,-3.061979863765,-1.129624298873));
#14832=CARTESIAN_POINT('Ctrl Pts',(10.73749295432,-2.119635939241,-2.481754111378));
#14833=CARTESIAN_POINT('Ctrl Pts',(10.89674295432,-0.6366272854614,-3.200971110614));
#14834=CARTESIAN_POINT('Ctrl Pts',(11.00290962098,0.4599252670358,-3.136380672689));
#14835=CARTESIAN_POINT('Ctrl Pts',(11.05599295432,0.9656781074217,-2.972051613422));
#14836=CARTESIAN_POINT('Ctrl Pts',(5.849007045683,0.9656781074217,2.972051613422));
#14837=CARTESIAN_POINT('Ctrl Pts',(5.902090379016,0.4599252670358,3.136380672689));
#14838=CARTESIAN_POINT('Ctrl Pts',(6.008257045683,-0.6366272854614,3.200971110614));
#14839=CARTESIAN_POINT('Ctrl Pts',(6.167507045683,-2.119635939241,2.481754111378));
#14840=CARTESIAN_POINT('Ctrl Pts',(6.326757045683,-3.061979863765,1.129624298873));
#14841=CARTESIAN_POINT('Ctrl Pts',(6.486007045683,-3.223532154246,-0.5105564866689));
#14842=CARTESIAN_POINT('Ctrl Pts',(6.645257045683,-2.563047905408,-2.020544571702));
#14843=CARTESIAN_POINT('Ctrl Pts',(6.804507045683,-1.248968678135,-3.015276776083));
#14844=CARTESIAN_POINT('Ctrl Pts',(6.963757045683,0.383608261101,-3.241089558554));
#14845=CARTESIAN_POINT('Ctrl Pts',(7.123007045683,1.918361836065,-2.640398557608));
#14846=CARTESIAN_POINT('Ctrl Pts',(7.282257045683,2.963917875123,-1.366384855545));
#14847=CARTESIAN_POINT('Ctrl Pts',(7.441507045683,3.253651172662,0.256067900963));
#14848=CARTESIAN_POINT('Ctrl Pts',(7.600757045683,2.713677441724,1.813221296591));
#14849=CARTESIAN_POINT('Ctrl Pts',(7.760007045683,1.481694291113,2.907988781792));
#14850=CARTESIAN_POINT('Ctrl Pts',(7.919257045683,-0.1281327360592,3.261195904774));
#14851=CARTESIAN_POINT('Ctrl Pts',(8.078507045683,-1.705284892359,2.782772028626));
#14852=CARTESIAN_POINT('Ctrl Pts',(8.237757045683,-2.84757578293,1.59471906236));
#14853=CARTESIAN_POINT('Ctrl Pts',(8.397007045683,-3.263712108535,0.));
#14854=CARTESIAN_POINT('Ctrl Pts',(8.556257045683,-2.84757578293,-1.59471906236));
#14855=CARTESIAN_POINT('Ctrl Pts',(8.715507045683,-1.705284892359,-2.782772028626));
#14856=CARTESIAN_POINT('Ctrl Pts',(8.874757045683,-0.1281327360592,-3.261195904774));
#14857=CARTESIAN_POINT('Ctrl Pts',(9.034007045683,1.481694291113,-2.907988781792));
#14858=CARTESIAN_POINT('Ctrl Pts',(9.193257045683,2.713677441724,-1.813221296591));
#14859=CARTESIAN_POINT('Ctrl Pts',(9.352507045683,3.253651172662,-0.256067900963));
#14860=CARTESIAN_POINT('Ctrl Pts',(9.511757045683,2.963917875123,1.366384855545));
#14861=CARTESIAN_POINT('Ctrl Pts',(9.671007045683,1.918361836065,2.640398557608));
#14862=CARTESIAN_POINT('Ctrl Pts',(9.830257045683,0.383608261101,3.241089558554));
#14863=CARTESIAN_POINT('Ctrl Pts',(9.989507045683,-1.248968678135,3.015276776083));
#14864=CARTESIAN_POINT('Ctrl Pts',(10.14875704568,-2.563047905408,2.020544571702));
#14865=CARTESIAN_POINT('Ctrl Pts',(10.30800704568,-3.223532154246,0.5105564866689));
#14866=CARTESIAN_POINT('Ctrl Pts',(10.46725704568,-3.061979863765,-1.129624298873));
#14867=CARTESIAN_POINT('Ctrl Pts',(10.62650704568,-2.119635939241,-2.481754111378));
#14868=CARTESIAN_POINT('Ctrl Pts',(10.78575704568,-0.6366272854614,-3.200971110614));
#14869=CARTESIAN_POINT('Ctrl Pts',(10.89192371235,0.4599252670358,-3.136380672689));
#14870=CARTESIAN_POINT('Ctrl Pts',(10.94500704568,0.9656781074217,-2.972051613422));
#14871=CARTESIAN_POINT('Ctrl Pts',(5.738021137048,0.9656781074217,2.972051613422));
#14872=CARTESIAN_POINT('Ctrl Pts',(5.791104470382,0.4599252670358,3.136380672689));
#14873=CARTESIAN_POINT('Ctrl Pts',(5.897271137048,-0.6366272854614,3.200971110614));
#14874=CARTESIAN_POINT('Ctrl Pts',(6.056521137048,-2.119635939241,2.481754111378));
#14875=CARTESIAN_POINT('Ctrl Pts',(6.215771137048,-3.061979863765,1.129624298873));
#14876=CARTESIAN_POINT('Ctrl Pts',(6.375021137048,-3.223532154246,-0.5105564866689));
#14877=CARTESIAN_POINT('Ctrl Pts',(6.534271137048,-2.563047905408,-2.020544571702));
#14878=CARTESIAN_POINT('Ctrl Pts',(6.693521137048,-1.248968678135,-3.015276776083));
#14879=CARTESIAN_POINT('Ctrl Pts',(6.852771137048,0.383608261101,-3.241089558554));
#14880=CARTESIAN_POINT('Ctrl Pts',(7.012021137048,1.918361836065,-2.640398557608));
#14881=CARTESIAN_POINT('Ctrl Pts',(7.171271137048,2.963917875123,-1.366384855545));
#14882=CARTESIAN_POINT('Ctrl Pts',(7.330521137048,3.253651172662,0.256067900963));
#14883=CARTESIAN_POINT('Ctrl Pts',(7.489771137048,2.713677441724,1.813221296591));
#14884=CARTESIAN_POINT('Ctrl Pts',(7.649021137048,1.481694291113,2.907988781792));
#14885=CARTESIAN_POINT('Ctrl Pts',(7.808271137048,-0.1281327360592,3.261195904774));
#14886=CARTESIAN_POINT('Ctrl Pts',(7.967521137048,-1.705284892359,2.782772028626));
#14887=CARTESIAN_POINT('Ctrl Pts',(8.126771137048,-2.84757578293,1.59471906236));
#14888=CARTESIAN_POINT('Ctrl Pts',(8.286021137048,-3.263712108535,0.));
#14889=CARTESIAN_POINT('Ctrl Pts',(8.445271137048,-2.84757578293,-1.59471906236));
#14890=CARTESIAN_POINT('Ctrl Pts',(8.604521137048,-1.705284892359,-2.782772028626));
#14891=CARTESIAN_POINT('Ctrl Pts',(8.763771137048,-0.1281327360592,-3.261195904774));
#14892=CARTESIAN_POINT('Ctrl Pts',(8.923021137048,1.481694291113,-2.907988781792));
#14893=CARTESIAN_POINT('Ctrl Pts',(9.082271137048,2.713677441724,-1.813221296591));
#14894=CARTESIAN_POINT('Ctrl Pts',(9.241521137048,3.253651172662,-0.256067900963));
#14895=CARTESIAN_POINT('Ctrl Pts',(9.400771137048,2.963917875123,1.366384855545));
#14896=CARTESIAN_POINT('Ctrl Pts',(9.560021137048,1.918361836065,2.640398557608));
#14897=CARTESIAN_POINT('Ctrl Pts',(9.719271137048,0.383608261101,3.241089558554));
#14898=CARTESIAN_POINT('Ctrl Pts',(9.878521137048,-1.248968678135,3.015276776083));
#14899=CARTESIAN_POINT('Ctrl Pts',(10.03777113705,-2.563047905408,2.020544571702));
#14900=CARTESIAN_POINT('Ctrl Pts',(10.19702113705,-3.223532154246,0.5105564866689));
#14901=CARTESIAN_POINT('Ctrl Pts',(10.35627113705,-3.061979863765,-1.129624298873));
#14902=CARTESIAN_POINT('Ctrl Pts',(10.51552113705,-2.119635939241,-2.481754111378));
#14903=CARTESIAN_POINT('Ctrl Pts',(10.67477113705,-0.6366272854614,-3.200971110614));
#14904=CARTESIAN_POINT('Ctrl Pts',(10.78093780372,0.4599252670358,-3.136380672689));
#14905=CARTESIAN_POINT('Ctrl Pts',(10.83402113705,0.9656781074217,-2.972051613422));
#14906=CARTESIAN_POINT('Ctrl Pts',(5.88,-3.21695909910602E-7,3.12449703095644));
#14907=CARTESIAN_POINT('Ctrl Pts',(5.895705128205,-0.157306535044492,3.12459764304402));
#14908=CARTESIAN_POINT('Ctrl Pts',(5.91141025641,-0.314639539052909,3.112929841749));
#14909=CARTESIAN_POINT('Ctrl Pts',(5.92711538461517,-0.470193579471061,
3.08937038670253));
#14910=CARTESIAN_POINT('Ctrl Pts',(5.93182698771779,-0.516860431844728,
3.08230245321972));
#14911=CARTESIAN_POINT('Ctrl Pts',(5.93653859082043,-0.563365438343652,
3.07416446995282));
#14912=CARTESIAN_POINT('Ctrl Pts',(5.94125019392308,-0.609657256300367,
3.06495400126008));
#14913=CARTESIAN_POINT('Ctrl Pts',(5.95224371902567,-0.717669381189642,
3.04346332885533));
#14914=CARTESIAN_POINT('Ctrl Pts',(5.9632372441283,-0.824520523417935,3.01613287001461));
#14915=CARTESIAN_POINT('Ctrl Pts',(5.97423076923084,-0.929617596829347,
2.98324879794399));
#14916=CARTESIAN_POINT('Ctrl Pts',(5.989935897436,-1.07975715593506,2.93627127590627));
#14917=CARTESIAN_POINT('Ctrl Pts',(6.00564102564099,-1.22632914373851,2.87796151164342));
#14918=CARTESIAN_POINT('Ctrl Pts',(6.02134615384615,-1.36775803719343,2.8091039241222));
#14919=CARTESIAN_POINT('Ctrl Pts',(6.03705128205133,-1.5091869306485,2.74024633660091));
#14920=CARTESIAN_POINT('Ctrl Pts',(6.05275641025667,-1.64548597437029,2.66083432711573));
#14921=CARTESIAN_POINT('Ctrl Pts',(6.06846153846185,-1.77506014945936,2.57161807835128));
#14922=CARTESIAN_POINT('Ctrl Pts',(6.07914097076807,-1.86317013579121,2.51095134091064));
#14923=CARTESIAN_POINT('Ctrl Pts',(6.08982040307421,-1.94817288076982,2.44574669164713));
#14924=CARTESIAN_POINT('Ctrl Pts',(6.10049983538033,-2.02952515103173,2.37626864249983));
#14925=CARTESIAN_POINT('Ctrl Pts',(6.10552553127922,-2.06780918704612,2.34357256496935));
#14926=CARTESIAN_POINT('Ctrl Pts',(6.1105512271781,-2.10528488988288,2.30993026036317));
#14927=CARTESIAN_POINT('Ctrl Pts',(6.11557692307699,-2.14191592065948,2.27539299236903));
#14928=CARTESIAN_POINT('Ctrl Pts',(6.13128205128199,-2.25638664196909,2.16746520831449));
#14929=CARTESIAN_POINT('Ctrl Pts',(6.14698717948701,-2.36259770943883,2.05080969082419));
#14930=CARTESIAN_POINT('Ctrl Pts',(6.16269230769218,-2.45953351178139,1.92692186650592));
#14931=CARTESIAN_POINT('Ctrl Pts',(6.17839743589734,-2.55646931412384,1.80303404218777));
#14932=CARTESIAN_POINT('Ctrl Pts',(6.19410256410266,-2.64414127751746,1.6719042538725));
#14933=CARTESIAN_POINT('Ctrl Pts',(6.20980769230782,-2.72154967470347,1.53495847225765));
#14934=CARTESIAN_POINT('Ctrl Pts',(6.22551282051299,-2.79895807188956,1.39801269064265));
#14935=CARTESIAN_POINT('Ctrl Pts',(6.24121794871801,-2.86610550760182,1.25523572060086));
#14936=CARTESIAN_POINT('Ctrl Pts',(6.25692307692301,-2.92192333127629,1.10813935100359));
#14937=CARTESIAN_POINT('Ctrl Pts',(6.25786539277047,-2.9252724296811,1.09931349244548));
#14938=CARTESIAN_POINT('Ctrl Pts',(6.25880770861792,-2.92858070337731,1.09047219858789));
#14939=CARTESIAN_POINT('Ctrl Pts',(6.25975002446537,-2.93184792475783,1.08161580336685));
#14940=CARTESIAN_POINT('Ctrl Pts',(6.27451283682291,-2.98303392179007,0.942866889013087));
#14941=CARTESIAN_POINT('Ctrl Pts',(6.28927564918046,-3.02414182613375,0.800411122418192));
#14942=CARTESIAN_POINT('Ctrl Pts',(6.30403846153816,-3.05502438429729,0.655798952752522));
#14943=CARTESIAN_POINT('Ctrl Pts',(6.31974358974334,-3.08787818772652,0.50195613408092));
#14944=CARTESIAN_POINT('Ctrl Pts',(6.33544871794871,-3.10916841598543,0.345660030799849));
#14945=CARTESIAN_POINT('Ctrl Pts',(6.3511538461539,-3.1187342224115,0.188648419769014));
#14946=CARTESIAN_POINT('Ctrl Pts',(6.36685897435902,-3.12830002883752,0.0316368087388328));
#14947=CARTESIAN_POINT('Ctrl Pts',(6.38256410256397,-3.12614026969898,-0.12610510103707));
#14948=CARTESIAN_POINT('Ctrl Pts',(6.39826923076908,-3.11205714799653,-0.282798238157188));
#14949=CARTESIAN_POINT('Ctrl Pts',(6.40517951072145,-3.10586055333675,-0.351743453374321));
#14950=CARTESIAN_POINT('Ctrl Pts',(6.41208979067384,-3.09735519217736,-0.420484489677447));
#14951=CARTESIAN_POINT('Ctrl Pts',(6.41900007062624,-3.0865260643595,-0.488857703250767));
#14952=CARTESIAN_POINT('Ctrl Pts',(6.42779491887912,-3.07274362189333,-0.575877627491321));
#14953=CARTESIAN_POINT('Ctrl Pts',(6.436589767132,-3.05519690668903,-0.66230164565767));
#14954=CARTESIAN_POINT('Ctrl Pts',(6.44538461538482,-3.0340200977109,-0.74781859016398));
#14955=CARTESIAN_POINT('Ctrl Pts',(6.46108974359,-2.99620426616755,-0.900527828411023));
#14956=CARTESIAN_POINT('Ctrl Pts',(6.476794871795,-2.94681582966476,-1.05034855944726));
#14957=CARTESIAN_POINT('Ctrl Pts',(6.4925,-2.88658577275698,-1.1956628320182));
#14958=CARTESIAN_POINT('Ctrl Pts',(6.508205128205,-2.82635571584919,-1.34097710458913));
#14959=CARTESIAN_POINT('Ctrl Pts',(6.52391025641,-2.75527937991822,-1.48179891776845));
#14960=CARTESIAN_POINT('Ctrl Pts',(6.53961538461517,-2.67404531641151,-1.61651716219695));
#14961=CARTESIAN_POINT('Ctrl Pts',(6.55249354986765,-2.60743359059155,-1.72698578057497));
#14962=CARTESIAN_POINT('Ctrl Pts',(6.56537171512024,-2.53398384454478,-1.83335602635669));
#14963=CARTESIAN_POINT('Ctrl Pts',(6.57824988037278,-2.45411540900217,-1.93466859159332));
#14964=CARTESIAN_POINT('Ctrl Pts',(6.58107684332547,-2.43658301180572,-1.9569083177461));
#14965=CARTESIAN_POINT('Ctrl Pts',(6.58390380627817,-2.41874138908149,-1.97890437133876));
#14966=CARTESIAN_POINT('Ctrl Pts',(6.58673076923086,-2.4005992967642,-2.00064999697506));
#14967=CARTESIAN_POINT('Ctrl Pts',(6.60243589743606,-2.29981131668746,-2.12145732421479));
#14968=CARTESIAN_POINT('Ctrl Pts',(6.61814102564111,-2.18976698077217,-2.23451450223418));
#14969=CARTESIAN_POINT('Ctrl Pts',(6.63384615384633,-2.07193616153301,-2.33873186210924));
#14970=CARTESIAN_POINT('Ctrl Pts',(6.64955128205139,-1.95410534229508,-2.44294922198321));
#14971=CARTESIAN_POINT('Ctrl Pts',(6.66525641025661,-1.82847988986133,-2.53833958057375));
#14972=CARTESIAN_POINT('Ctrl Pts',(6.68096153846167,-1.69644712969505,-2.62385329049029));
#14973=CARTESIAN_POINT('Ctrl Pts',(6.69666666666689,-1.56441436952739,-2.70936700040773));
#14974=CARTESIAN_POINT('Ctrl Pts',(6.71237179487195,-1.42595984987577,-2.78500861783667));
#14975=CARTESIAN_POINT('Ctrl Pts',(6.72807692307697,-1.28252819003516,-2.84966078036119));
#14976=CARTESIAN_POINT('Ctrl Pts',(6.73121799320022,-1.25384145182002,-2.86259139598291));
#14977=CARTESIAN_POINT('Ctrl Pts',(6.73435906332347,-1.22495656311743,-2.8750820037678));
#14978=CARTESIAN_POINT('Ctrl Pts',(6.73750013344671,-1.19588572614117,-2.887123539098));
#14979=CARTESIAN_POINT('Ctrl Pts',(6.75006419152849,-1.07960443666829,-2.93528882778825));
#14980=CARTESIAN_POINT('Ctrl Pts',(6.76262824961027,-0.960347655502351,
-2.97626761538678));
#14981=CARTESIAN_POINT('Ctrl Pts',(6.77519230769217,-0.83908019289306,-3.00992620370386));
#14982=CARTESIAN_POINT('Ctrl Pts',(6.79089743589734,-0.687495327956873,
-3.05199958805779));
#14983=CARTESIAN_POINT('Ctrl Pts',(6.80660256410267,-0.532757793114142,
-3.08264413157538));
#14984=CARTESIAN_POINT('Ctrl Pts',(6.82230769230783,-0.376606556598297,
-3.10163498008567));
#14985=CARTESIAN_POINT('Ctrl Pts',(6.838012820513,-0.220455320082452,-3.12062582859596));
#14986=CARTESIAN_POINT('Ctrl Pts',(6.853717948718,-0.0628756645481069,-3.12796387302098));
#14987=CARTESIAN_POINT('Ctrl Pts',(6.86942307692303,0.0943789619765832,
-3.12338542308761));
#14988=CARTESIAN_POINT('Ctrl Pts',(6.87853202085236,0.185586340671031,-3.12072993099726));
#14989=CARTESIAN_POINT('Ctrl Pts',(6.88764096478169,0.276685802602264,-3.11406434039434));
#14990=CARTESIAN_POINT('Ctrl Pts',(6.89674990871107,0.367304367055668,-3.1033389279845));
#14991=CARTESIAN_POINT('Ctrl Pts',(6.9033460929868,0.432925228768241,-3.09557218825737));
#14992=CARTESIAN_POINT('Ctrl Pts',(6.90994227726255,0.498293895125398,-3.08567670510919));
#14993=CARTESIAN_POINT('Ctrl Pts',(6.91653846153833,0.563276981103822,-3.07370359533634));
#14994=CARTESIAN_POINT('Ctrl Pts',(6.93224358974339,0.717997900620677,-3.04519632262622));
#14995=CARTESIAN_POINT('Ctrl Pts',(6.94794871794861,0.870526272338136,-3.00491480017493));
#14996=CARTESIAN_POINT('Ctrl Pts',(6.96365384615367,1.01920094228016,-2.95353305961266));
#14997=CARTESIAN_POINT('Ctrl Pts',(6.97935897435889,1.16787561222373,-2.90215131904986));
#14998=CARTESIAN_POINT('Ctrl Pts',(6.99506410256395,1.31271118268685,-2.83966664030563));
#14999=CARTESIAN_POINT('Ctrl Pts',(7.01076923076914,1.45207966320917,-2.76670577109897));
#15000=CARTESIAN_POINT('Ctrl Pts',(7.02584614949763,1.58587336592168,-2.69666335686228));
#15001=CARTESIAN_POINT('Ctrl Pts',(7.04092306822624,1.71463784791186,-2.61695511461419));
#15002=CARTESIAN_POINT('Ctrl Pts',(7.05599998695472,1.836828913414,-2.52817810742183));
#15003=CARTESIAN_POINT('Ctrl Pts',(7.05662819643142,1.84192024452083,-2.52447903878345));
#15004=CARTESIAN_POINT('Ctrl Pts',(7.05725640590813,1.8470001649315,-2.52076422913783));
#15005=CARTESIAN_POINT('Ctrl Pts',(7.05788461538484,1.85206859791098,-2.51703377008661));
#15006=CARTESIAN_POINT('Ctrl Pts',(7.07358974359,1.97877854529902,-2.42377293936711));
#15007=CARTESIAN_POINT('Ctrl Pts',(7.089294871795,2.09828043057227,-2.32075011669408));
#15008=CARTESIAN_POINT('Ctrl Pts',(7.105,2.20940661429584,-2.20940720229315));
#15009=CARTESIAN_POINT('Ctrl Pts',(7.120705128205,2.32053279801942,-2.09806428789222));
#15010=CARTESIAN_POINT('Ctrl Pts',(7.13641025641,2.42329735285879,-1.97839483543744));
#15011=CARTESIAN_POINT('Ctrl Pts',(7.15211538461517,2.51660034679189,-1.85174928324409));
#15012=CARTESIAN_POINT('Ctrl Pts',(7.16782051282033,2.60990334072498,-1.72510373105075));
#15013=CARTESIAN_POINT('Ctrl Pts',(7.18352564102567,2.69375117108915,-1.59146857523107));
#15014=CARTESIAN_POINT('Ctrl Pts',(7.19923076923086,2.76698261297629,-1.45222443021403));
#15015=CARTESIAN_POINT('Ctrl Pts',(7.20457056320872,2.79188153817257,-1.40488097415942));
#15016=CARTESIAN_POINT('Ctrl Pts',(7.20991035718657,2.81555228674541,-1.35689047491985));
#15017=CARTESIAN_POINT('Ctrl Pts',(7.21525015116441,2.83794741820317,-1.30831167980417));
#15018=CARTESIAN_POINT('Ctrl Pts',(7.2256154853917,2.88141969889172,-1.21401301400872));
#15019=CARTESIAN_POINT('Ctrl Pts',(7.23598081961898,2.9200846630212,-1.11749740512213));
#15020=CARTESIAN_POINT('Ctrl Pts',(7.24634615384633,2.95384328122046,-1.01930854475145));
#15021=CARTESIAN_POINT('Ctrl Pts',(7.26205128205139,3.00499295138218,-0.870536820983832));
#15022=CARTESIAN_POINT('Ctrl Pts',(7.27775641025661,3.04488646955175,-0.717917299307448));
#15023=CARTESIAN_POINT('Ctrl Pts',(7.29346153846167,3.07323267657502,-0.563190821606695));
#15024=CARTESIAN_POINT('Ctrl Pts',(7.30916666666689,3.10157888359859,-0.408464343904331));
#15025=CARTESIAN_POINT('Ctrl Pts',(7.32487179487195,3.11838067165169,-0.251616473021808));
#15026=CARTESIAN_POINT('Ctrl Pts',(7.34057692307697,3.12331108802163,-0.0943762077870904));
#15027=CARTESIAN_POINT('Ctrl Pts',(7.35188456103662,3.12686097074617,0.018836239048195));
#15028=CARTESIAN_POINT('Ctrl Pts',(7.36319219899625,3.12425420322951,0.132257831845049));
#15029=CARTESIAN_POINT('Ctrl Pts',(7.37449983695594,3.11536666791583,0.245184674149663));
#15030=CARTESIAN_POINT('Ctrl Pts',(7.37889732720134,3.11191034485466,0.289101422213974));
#15031=CARTESIAN_POINT('Ctrl Pts',(7.38329481744675,3.10750429091715,0.332943335439869));
#15032=CARTESIAN_POINT('Ctrl Pts',(7.38769230769217,3.10216193300488,0.37667061407462));
#15033=CARTESIAN_POINT('Ctrl Pts',(7.40339743589733,3.08308231912341,0.532837536272352));
#15034=CARTESIAN_POINT('Ctrl Pts',(7.41910256410267,3.05206338319806,0.687523279012142));
#15035=CARTESIAN_POINT('Ctrl Pts',(7.43480769230783,3.0097189125242,0.839021679403842));
#15036=CARTESIAN_POINT('Ctrl Pts',(7.450512820513,2.96737444185033,0.990520079795541));
#15037=CARTESIAN_POINT('Ctrl Pts',(7.466217948718,2.91370372918221,1.13884614555346));
#15038=CARTESIAN_POINT('Ctrl Pts',(7.48192307692303,2.84927329204631,1.28235426733883));
#15039=CARTESIAN_POINT('Ctrl Pts',(7.49762820512805,2.78484285491041,1.42586238912421));
#15040=CARTESIAN_POINT('Ctrl Pts',(7.51333333333311,2.70964227733817,1.56456383704047));
#15041=CARTESIAN_POINT('Ctrl Pts',(7.52903846153833,2.62426134529928,1.69671142476984));
#15042=CARTESIAN_POINT('Ctrl Pts',(7.5306089923509,2.61572315428164,1.70992633493315));
#15043=CARTESIAN_POINT('Ctrl Pts',(7.53217952316347,2.60708334093589,1.72307544280506));
#15044=CARTESIAN_POINT('Ctrl Pts',(7.53375005397604,2.59834253844517,1.7361569781865));
#15045=CARTESIAN_POINT('Ctrl Pts',(7.54788465136856,2.5196763173783,1.85388929799372));
#15046=CARTESIAN_POINT('Ctrl Pts',(7.56201924876118,2.4328286128156,1.96614691665661));
#15047=CARTESIAN_POINT('Ctrl Pts',(7.57615384615367,2.33882800562177,2.07202028766332));
#15048=CARTESIAN_POINT('Ctrl Pts',(7.59185897435889,2.23438275356725,2.18965751630222));
#15049=CARTESIAN_POINT('Ctrl Pts',(7.60756410256395,2.12110179310409,2.29942752308062));
#15050=CARTESIAN_POINT('Ctrl Pts',(7.62326923076914,2.00029920318409,2.40017868230316));
#15051=CARTESIAN_POINT('Ctrl Pts',(7.63897435897433,1.87949661326408,2.5009298415257));
#15052=CARTESIAN_POINT('Ctrl Pts',(7.65467948717967,1.75116000914845,2.59267025933498));
#15053=CARTESIAN_POINT('Ctrl Pts',(7.67038461538483,1.61660883785066,2.674197927153));
#15054=CARTESIAN_POINT('Ctrl Pts',(7.67792308497015,1.55202420668778,2.71333124947796));
#15055=CARTESIAN_POINT('Ctrl Pts',(7.68546155455542,1.48600787178097,2.75011066378684));
#15056=CARTESIAN_POINT('Ctrl Pts',(7.69300002414067,1.41872031168613,2.78439538808883));
#15057=CARTESIAN_POINT('Ctrl Pts',(7.70116668276046,1.34582560455246,2.82153709650612));
#15058=CARTESIAN_POINT('Ctrl Pts',(7.70933334138023,1.27143900290213,2.85575093945237));
#15059=CARTESIAN_POINT('Ctrl Pts',(7.7175,1.19582529175154,2.88697719853058));
#15060=CARTESIAN_POINT('Ctrl Pts',(7.733205128205,1.05041416549221,2.94702775592731));
#15061=CARTESIAN_POINT('Ctrl Pts',(7.74891025641,0.900465813463126,2.99603287482205));
#15062=CARTESIAN_POINT('Ctrl Pts',(7.76461538461517,0.747723396432291,3.03363235324925));
#15063=CARTESIAN_POINT('Ctrl Pts',(7.78032051282033,0.594980979401457,3.07123183167645));
#15064=CARTESIAN_POINT('Ctrl Pts',(7.79602564102567,0.439430544027183,3.09743052627249));
#15065=CARTESIAN_POINT('Ctrl Pts',(7.81173076923086,0.282778041871423,3.11184033086417));
#15066=CARTESIAN_POINT('Ctrl Pts',(7.82523715029811,0.148057181168531,3.12423273603125));
#15067=CARTESIAN_POINT('Ctrl Pts',(7.83874353136525,0.0125106239082456,
3.12790266438722));
#15068=CARTESIAN_POINT('Ctrl Pts',(7.85224991243248,-0.122686924247132,
3.12259073825233));
#15069=CARTESIAN_POINT('Ctrl Pts',(7.85444865957043,-0.144696167180856,
3.1217259927422));
#15070=CARTESIAN_POINT('Ctrl Pts',(7.85664740670837,-0.166696155154839,
3.12062326574181));
#15071=CARTESIAN_POINT('Ctrl Pts',(7.85884615384633,-0.1886819155548,3.11928401449904));
#15072=CARTESIAN_POINT('Ctrl Pts',(7.87455128205139,-0.345720976484957,
3.10971806118707));
#15073=CARTESIAN_POINT('Ctrl Pts',(7.89025641025661,-0.502004351790296,
3.08808590041721));
#15074=CARTESIAN_POINT('Ctrl Pts',(7.90596153846167,-0.655779338422631,
3.05493687313145));
#15075=CARTESIAN_POINT('Ctrl Pts',(7.92166666666689,-0.809554325056565,
3.02178784584535));
#15076=CARTESIAN_POINT('Ctrl Pts',(7.93737179487195,-0.960836126315138,
2.9771233215876));
#15077=CARTESIAN_POINT('Ctrl Pts',(7.95307692307697,-1.10796040920211,2.9214504428197));
#15078=CARTESIAN_POINT('Ctrl Pts',(7.968782051282,-1.25508469208908,2.86577756405179));
#15079=CARTESIAN_POINT('Ctrl Pts',(7.984487179487,-1.39806382918831,2.79908769904581));
#15080=CARTESIAN_POINT('Ctrl Pts',(8.00019230769217,-1.53515081641421,2.72188982514671));
#15081=CARTESIAN_POINT('Ctrl Pts',(8.00396158983553,-1.56805214178305,2.70336208288368));
#15082=CARTESIAN_POINT('Ctrl Pts',(8.00773087197889,-1.60061292833792,2.68422968792613));
#15083=CARTESIAN_POINT('Ctrl Pts',(8.01150015412227,-1.63280801473754,2.66450051360633));
#15084=CARTESIAN_POINT('Ctrl Pts',(8.02343600018412,-1.73475729329959,2.60202591535358));
#15085=CARTESIAN_POINT('Ctrl Pts',(8.03537184624603,-1.8330386668105,2.53356607404464));
#15086=CARTESIAN_POINT('Ctrl Pts',(8.04730769230783,-1.92707055798493,2.45972435726965));
#15087=CARTESIAN_POINT('Ctrl Pts',(8.063012820513,-2.05079726312352,2.36256378542284));
#15088=CARTESIAN_POINT('Ctrl Pts',(8.078717948718,-2.16717972241397,2.25608242363812));
#15089=CARTESIAN_POINT('Ctrl Pts',(8.09442307692303,-2.27501273852753,2.14155794469054));
#15090=CARTESIAN_POINT('Ctrl Pts',(8.11012820512806,-2.3828457546411,2.02703346574295));
#15091=CARTESIAN_POINT('Ctrl Pts',(8.12583333333311,-2.48213900530219,1.90445476333191));
#15092=CARTESIAN_POINT('Ctrl Pts',(8.14153846153833,-2.57165193077396,1.77508287620843));
#15093=CARTESIAN_POINT('Ctrl Pts',(8.15127559877096,-2.62714970373215,1.69487265426663));
#15094=CARTESIAN_POINT('Ctrl Pts',(8.16101273600365,-2.67888797642152,1.61204808608716));
#15095=CARTESIAN_POINT('Ctrl Pts',(8.17074987323633,-2.72655002210233,1.52694137967767));
#15096=CARTESIAN_POINT('Ctrl Pts',(8.17671786420879,-2.75576257724611,1.47477860910038));
#15097=CARTESIAN_POINT('Ctrl Pts',(8.18268585518124,-2.78344401079767,1.42175865550711));
#15098=CARTESIAN_POINT('Ctrl Pts',(8.18865384615367,-2.80956688241491,1.36798352909411));
#15099=CARTESIAN_POINT('Ctrl Pts',(8.20435897435889,-2.87831079468499,1.22647104047447));
#15100=CARTESIAN_POINT('Ctrl Pts',(8.22006410256395,-2.9362584893282,1.07973927060473));
#15101=CARTESIAN_POINT('Ctrl Pts',(8.23576923076914,-2.982977349702,0.929533639746724));
#15102=CARTESIAN_POINT('Ctrl Pts',(8.25147435897433,-3.0296962100758,0.779328008888721));
#15103=CARTESIAN_POINT('Ctrl Pts',(8.26717948717967,-3.06519301000169,0.625635251226046));
#15104=CARTESIAN_POINT('Ctrl Pts',(8.28288461538483,-3.08901983228559,0.470139769698067));
#15105=CARTESIAN_POINT('Ctrl Pts',(8.29858974359,-3.11284665456948,0.314644288170088));
#15106=CARTESIAN_POINT('Ctrl Pts',(8.314294871795,-3.125,0.157330906751383));
#15107=CARTESIAN_POINT('Ctrl Pts',(8.33,-3.125,0.));
#15108=CARTESIAN_POINT('Ctrl Pts',(8.345705128205,-3.125,-0.157330906751383));
#15109=CARTESIAN_POINT('Ctrl Pts',(8.36141025641,-3.11284665456948,-0.314644288170091));
#15110=CARTESIAN_POINT('Ctrl Pts',(8.37711538461517,-3.08901983228559,-0.47013976969807));
#15111=CARTESIAN_POINT('Ctrl Pts',(8.39282051282033,-3.06519301000169,-0.625635251226049));
#15112=CARTESIAN_POINT('Ctrl Pts',(8.40852564102567,-3.0296962100758,-0.779328008888722));
#15113=CARTESIAN_POINT('Ctrl Pts',(8.42423076923086,-2.982977349702,-0.929533639746725));
#15114=CARTESIAN_POINT('Ctrl Pts',(8.43993589743605,-2.9362584893282,-1.07973927060473));
#15115=CARTESIAN_POINT('Ctrl Pts',(8.45564102564111,-2.87831079468499,-1.22647104047447));
#15116=CARTESIAN_POINT('Ctrl Pts',(8.47134615384633,-2.80956688241491,-1.36798352909411));
#15117=CARTESIAN_POINT('Ctrl Pts',(8.47731414481876,-2.78344401079767,-1.42175865550711));
#15118=CARTESIAN_POINT('Ctrl Pts',(8.48328213579122,-2.75576257724611,-1.47477860910038));
#15119=CARTESIAN_POINT('Ctrl Pts',(8.48925012676368,-2.72655002210233,-1.52694137967767));
#15120=CARTESIAN_POINT('Ctrl Pts',(8.49898726399635,-2.67888797642152,-1.61204808608716));
#15121=CARTESIAN_POINT('Ctrl Pts',(8.50872440122904,-2.62714970373215,-1.69487265426663));
#15122=CARTESIAN_POINT('Ctrl Pts',(8.51846153846167,-2.57165193077395,-1.77508287620844));
#15123=CARTESIAN_POINT('Ctrl Pts',(8.53416666666689,-2.48213900530219,-1.90445476333191));
#15124=CARTESIAN_POINT('Ctrl Pts',(8.54987179487195,-2.3828457546411,-2.02703346574295));
#15125=CARTESIAN_POINT('Ctrl Pts',(8.56557692307697,-2.27501273852753,-2.14155794469054));
#15126=CARTESIAN_POINT('Ctrl Pts',(8.581282051282,-2.16717972241396,-2.25608242363812));
#15127=CARTESIAN_POINT('Ctrl Pts',(8.596987179487,-2.05079726312352,-2.36256378542284));
#15128=CARTESIAN_POINT('Ctrl Pts',(8.61269230769217,-1.92707055798493,-2.45972435726965));
#15129=CARTESIAN_POINT('Ctrl Pts',(8.62462815375398,-1.8330386668105,-2.53356607404464));
#15130=CARTESIAN_POINT('Ctrl Pts',(8.63656399981588,-1.73475729329959,-2.60202591535358));
#15131=CARTESIAN_POINT('Ctrl Pts',(8.64849984587773,-1.63280801473754,-2.66450051360633));
#15132=CARTESIAN_POINT('Ctrl Pts',(8.65226912802111,-1.60061292833792,-2.68422968792613));
#15133=CARTESIAN_POINT('Ctrl Pts',(8.65603841016448,-1.56805214178305,-2.70336208288368));
#15134=CARTESIAN_POINT('Ctrl Pts',(8.65980769230783,-1.53515081641421,-2.72188982514671));
#15135=CARTESIAN_POINT('Ctrl Pts',(8.675512820513,-1.39806382918831,-2.79908769904581));
#15136=CARTESIAN_POINT('Ctrl Pts',(8.691217948718,-1.25508469208908,-2.86577756405179));
#15137=CARTESIAN_POINT('Ctrl Pts',(8.70692307692303,-1.10796040920211,-2.92145044281969));
#15138=CARTESIAN_POINT('Ctrl Pts',(8.72262820512806,-0.960836126315141,
-2.9771233215876));
#15139=CARTESIAN_POINT('Ctrl Pts',(8.73833333333311,-0.809554325056562,
-3.02178784584535));
#15140=CARTESIAN_POINT('Ctrl Pts',(8.75403846153833,-0.655779338422628,
-3.05493687313145));
#15141=CARTESIAN_POINT('Ctrl Pts',(8.76974358974339,-0.502004351790293,
-3.08808590041721));
#15142=CARTESIAN_POINT('Ctrl Pts',(8.78544871794861,-0.345720976484962,
-3.10971806118707));
#15143=CARTESIAN_POINT('Ctrl Pts',(8.80115384615367,-0.188681915554805,
-3.11928401449904));
#15144=CARTESIAN_POINT('Ctrl Pts',(8.80335259329162,-0.166696155154845,
-3.12062326574181));
#15145=CARTESIAN_POINT('Ctrl Pts',(8.80555134042957,-0.144696167180862,
-3.1217259927422));
#15146=CARTESIAN_POINT('Ctrl Pts',(8.80775008756752,-0.122686924247137,
-3.12259073825233));
#15147=CARTESIAN_POINT('Ctrl Pts',(8.82125646863476,0.0125106239082456,
-3.12790266438722));
#15148=CARTESIAN_POINT('Ctrl Pts',(8.83476284970189,0.148057181168534,-3.12423273603126));
#15149=CARTESIAN_POINT('Ctrl Pts',(8.84826923076914,0.282778041871425,-3.11184033086417));
#15150=CARTESIAN_POINT('Ctrl Pts',(8.86397435897433,0.439430544027182,-3.09743052627249));
#15151=CARTESIAN_POINT('Ctrl Pts',(8.87967948717967,0.594980979401456,-3.07123183167645));
#15152=CARTESIAN_POINT('Ctrl Pts',(8.89538461538483,0.747723396432294,-3.03363235324925));
#15153=CARTESIAN_POINT('Ctrl Pts',(8.91108974359,0.900465813463131,-2.99603287482204));
#15154=CARTESIAN_POINT('Ctrl Pts',(8.926794871795,1.05041416549222,-2.94702775592731));
#15155=CARTESIAN_POINT('Ctrl Pts',(8.9425,1.19582529175154,-2.88697719853058));
#15156=CARTESIAN_POINT('Ctrl Pts',(8.95066665861977,1.27143900290213,-2.85575093945237));
#15157=CARTESIAN_POINT('Ctrl Pts',(8.95883331723954,1.34582560455246,-2.82153709650612));
#15158=CARTESIAN_POINT('Ctrl Pts',(8.96699997585933,1.41872031168613,-2.78439538808883));
#15159=CARTESIAN_POINT('Ctrl Pts',(8.97453844544458,1.48600787178097,-2.75011066378684));
#15160=CARTESIAN_POINT('Ctrl Pts',(8.98207691502986,1.55202420668778,-2.71333124947796));
#15161=CARTESIAN_POINT('Ctrl Pts',(8.98961538461517,1.61660883785066,-2.674197927153));
#15162=CARTESIAN_POINT('Ctrl Pts',(9.00532051282033,1.75116000914844,-2.59267025933498));
#15163=CARTESIAN_POINT('Ctrl Pts',(9.02102564102567,1.87949661326408,-2.5009298415257));
#15164=CARTESIAN_POINT('Ctrl Pts',(9.03673076923086,2.00029920318409,-2.40017868230316));
#15165=CARTESIAN_POINT('Ctrl Pts',(9.05243589743606,2.12110179310409,-2.29942752308062));
#15166=CARTESIAN_POINT('Ctrl Pts',(9.06814102564111,2.23438275356726,-2.18965751630222));
#15167=CARTESIAN_POINT('Ctrl Pts',(9.08384615384633,2.33882800562177,-2.07202028766331));
#15168=CARTESIAN_POINT('Ctrl Pts',(9.09798075123882,2.4328286128156,-1.9661469166566));
#15169=CARTESIAN_POINT('Ctrl Pts',(9.11211534863145,2.5196763173783,-1.85388929799372));
#15170=CARTESIAN_POINT('Ctrl Pts',(9.12624994602396,2.59834253844517,-1.7361569781865));
#15171=CARTESIAN_POINT('Ctrl Pts',(9.12782047683653,2.60708334093589,-1.72307544280507));
#15172=CARTESIAN_POINT('Ctrl Pts',(9.1293910076491,2.61572315428164,-1.70992633493316));
#15173=CARTESIAN_POINT('Ctrl Pts',(9.13096153846167,2.62426134529928,-1.69671142476984));
#15174=CARTESIAN_POINT('Ctrl Pts',(9.14666666666689,2.70964227733817,-1.56456383704048));
#15175=CARTESIAN_POINT('Ctrl Pts',(9.16237179487195,2.78484285491041,-1.42586238912421));
#15176=CARTESIAN_POINT('Ctrl Pts',(9.17807692307697,2.84927329204631,-1.28235426733883));
#15177=CARTESIAN_POINT('Ctrl Pts',(9.193782051282,2.91370372918221,-1.13884614555346));
#15178=CARTESIAN_POINT('Ctrl Pts',(9.209487179487,2.96737444185033,-0.990520079795544));
#15179=CARTESIAN_POINT('Ctrl Pts',(9.22519230769217,3.0097189125242,-0.839021679403841));
#15180=CARTESIAN_POINT('Ctrl Pts',(9.24089743589733,3.05206338319806,-0.687523279012144));
#15181=CARTESIAN_POINT('Ctrl Pts',(9.25660256410267,3.08308231912341,-0.532837536272352));
#15182=CARTESIAN_POINT('Ctrl Pts',(9.27230769230784,3.10216193300488,-0.376670614074617));
#15183=CARTESIAN_POINT('Ctrl Pts',(9.27670518255326,3.10750429091715,-0.332943335439869));
#15184=CARTESIAN_POINT('Ctrl Pts',(9.28110267279866,3.11191034485466,-0.289101422213986));
#15185=CARTESIAN_POINT('Ctrl Pts',(9.28550016304406,3.11536666791583,-0.245184674149674));
#15186=CARTESIAN_POINT('Ctrl Pts',(9.29680780100375,3.12425420322951,-0.132257831845052));
#15187=CARTESIAN_POINT('Ctrl Pts',(9.30811543896338,3.12686097074617,-0.0188362390481956));
#15188=CARTESIAN_POINT('Ctrl Pts',(9.31942307692303,3.12331108802163,0.0943762077871013));
#15189=CARTESIAN_POINT('Ctrl Pts',(9.33512820512805,3.11838067165169,0.251616473021838));
#15190=CARTESIAN_POINT('Ctrl Pts',(9.35083333333311,3.10157888359858,0.408464343904398));
#15191=CARTESIAN_POINT('Ctrl Pts',(9.36653846153833,3.07323267657501,0.563190821606759));
#15192=CARTESIAN_POINT('Ctrl Pts',(9.38224358974339,3.04488646955173,0.717917299307511));
#15193=CARTESIAN_POINT('Ctrl Pts',(9.39794871794861,3.00499295138217,0.87053682098386));
#15194=CARTESIAN_POINT('Ctrl Pts',(9.41365384615367,2.95384328122045,1.01930854475146));
#15195=CARTESIAN_POINT('Ctrl Pts',(9.42401918038102,2.9200846630212,1.11749740512214));
#15196=CARTESIAN_POINT('Ctrl Pts',(9.4343845146083,2.88141969889172,1.21401301400872));
#15197=CARTESIAN_POINT('Ctrl Pts',(9.44474984883559,2.83794741820317,1.30831167980417));
#15198=CARTESIAN_POINT('Ctrl Pts',(9.45008964281343,2.8155522867454,1.35689047491985));
#15199=CARTESIAN_POINT('Ctrl Pts',(9.45542943679128,2.79188153817257,1.40488097415943));
#15200=CARTESIAN_POINT('Ctrl Pts',(9.46076923076914,2.76698261297628,1.45222443021404));
#15201=CARTESIAN_POINT('Ctrl Pts',(9.47647435897433,2.69375117108915,1.59146857523107));
#15202=CARTESIAN_POINT('Ctrl Pts',(9.49217948717967,2.60990334072498,1.72510373105075));
#15203=CARTESIAN_POINT('Ctrl Pts',(9.50788461538483,2.51660034679189,1.8517492832441));
#15204=CARTESIAN_POINT('Ctrl Pts',(9.52358974359,2.42329735285879,1.97839483543744));
#15205=CARTESIAN_POINT('Ctrl Pts',(9.539294871795,2.32053279801942,2.09806428789222));
#15206=CARTESIAN_POINT('Ctrl Pts',(9.555,2.20940661429584,2.20940720229315));
#15207=CARTESIAN_POINT('Ctrl Pts',(9.570705128205,2.09828043057227,2.32075011669408));
#15208=CARTESIAN_POINT('Ctrl Pts',(9.58641025641,1.97877854529902,2.42377293936711));
#15209=CARTESIAN_POINT('Ctrl Pts',(9.60211538461517,1.85206859791098,2.51703377008662));
#15210=CARTESIAN_POINT('Ctrl Pts',(9.60274359409187,1.84700016493149,2.52076422913783));
#15211=CARTESIAN_POINT('Ctrl Pts',(9.60337180356858,1.84192024452082,2.52447903878346));
#15212=CARTESIAN_POINT('Ctrl Pts',(9.60400001304529,1.83682891341399,2.52817810742184));
#15213=CARTESIAN_POINT('Ctrl Pts',(9.61907693177376,1.71463784791186,2.61695511461419));
#15214=CARTESIAN_POINT('Ctrl Pts',(9.63415385050238,1.58587336592168,2.69666335686228));
#15215=CARTESIAN_POINT('Ctrl Pts',(9.64923076923086,1.45207966320917,2.76670577109897));
#15216=CARTESIAN_POINT('Ctrl Pts',(9.66493589743606,1.31271118268685,2.83966664030563));
#15217=CARTESIAN_POINT('Ctrl Pts',(9.68064102564111,1.16787561222373,2.90215131904986));
#15218=CARTESIAN_POINT('Ctrl Pts',(9.69634615384633,1.01920094228016,2.95353305961267));
#15219=CARTESIAN_POINT('Ctrl Pts',(9.71205128205139,0.870526272338138,3.00491480017493));
#15220=CARTESIAN_POINT('Ctrl Pts',(9.72775641025661,0.717997900620678,3.04519632262622));
#15221=CARTESIAN_POINT('Ctrl Pts',(9.74346153846167,0.563276981103821,3.07370359533634));
#15222=CARTESIAN_POINT('Ctrl Pts',(9.75005772273745,0.498293895125397,3.08567670510919));
#15223=CARTESIAN_POINT('Ctrl Pts',(9.7566539070132,0.432925228768243,3.09557218825737));
#15224=CARTESIAN_POINT('Ctrl Pts',(9.76325009128893,0.367304367055667,3.1033389279845));
#15225=CARTESIAN_POINT('Ctrl Pts',(9.77235903521831,0.276685802602259,3.11406434039434));
#15226=CARTESIAN_POINT('Ctrl Pts',(9.78146797914765,0.185586340671027,3.12072993099726));
#15227=CARTESIAN_POINT('Ctrl Pts',(9.79057692307697,0.0943789619765783,
3.12338542308761));
#15228=CARTESIAN_POINT('Ctrl Pts',(9.806282051282,-0.0628756645481118,3.12796387302098));
#15229=CARTESIAN_POINT('Ctrl Pts',(9.821987179487,-0.220455320082457,3.12062582859596));
#15230=CARTESIAN_POINT('Ctrl Pts',(9.83769230769217,-0.376606556598298,
3.10163498008567));
#15231=CARTESIAN_POINT('Ctrl Pts',(9.85339743589733,-0.53275779311414,3.08264413157538));
#15232=CARTESIAN_POINT('Ctrl Pts',(9.86910256410266,-0.687495327956871,
3.0519995880578));
#15233=CARTESIAN_POINT('Ctrl Pts',(9.88480769230783,-0.839080192893056,
3.00992620370386));
#15234=CARTESIAN_POINT('Ctrl Pts',(9.89737175038972,-0.960347655502346,
2.97626761538679));
#15235=CARTESIAN_POINT('Ctrl Pts',(9.90993580847151,-1.07960443666828,2.93528882778825));
#15236=CARTESIAN_POINT('Ctrl Pts',(9.92249986655329,-1.19588572614116,2.887123539098));
#15237=CARTESIAN_POINT('Ctrl Pts',(9.92564093667654,-1.22495656311742,2.8750820037678));
#15238=CARTESIAN_POINT('Ctrl Pts',(9.92878200679978,-1.25384145182002,2.86259139598291));
#15239=CARTESIAN_POINT('Ctrl Pts',(9.93192307692303,-1.28252819003516,2.84966078036119));
#15240=CARTESIAN_POINT('Ctrl Pts',(9.94762820512806,-1.42595984987577,2.78500861783667));
#15241=CARTESIAN_POINT('Ctrl Pts',(9.96333333333311,-1.56441436952739,2.70936700040773));
#15242=CARTESIAN_POINT('Ctrl Pts',(9.97903846153766,-1.69644712969505,2.62385329049029));
#15243=CARTESIAN_POINT('Ctrl Pts',(9.99474358974206,-1.82847988986133,2.53833958057375));
#15244=CARTESIAN_POINT('Ctrl Pts',(10.0104487179459,-1.95410534229508,2.44294922198321));
#15245=CARTESIAN_POINT('Ctrl Pts',(10.0261538461512,-2.07193616153301,2.33873186210924));
#15246=CARTESIAN_POINT('Ctrl Pts',(10.0418589743566,-2.18976698077217,2.23451450223419));
#15247=CARTESIAN_POINT('Ctrl Pts',(10.0575641025633,-2.29981131668746,2.12145732421479));
#15248=CARTESIAN_POINT('Ctrl Pts',(10.0732692307683,-2.40059929676421,2.00064999697506));
#15249=CARTESIAN_POINT('Ctrl Pts',(10.076096193721,-2.4187413890815,1.97890437133876));
#15250=CARTESIAN_POINT('Ctrl Pts',(10.0789231566736,-2.43658301180573,1.9569083177461));
#15251=CARTESIAN_POINT('Ctrl Pts',(10.0817501196261,-2.45411540900217,1.93466859159331));
#15252=CARTESIAN_POINT('Ctrl Pts',(10.0946282848781,-2.53398384454479,1.83335602635669));
#15253=CARTESIAN_POINT('Ctrl Pts',(10.1075064501293,-2.60743359059154,1.72698578057498));
#15254=CARTESIAN_POINT('Ctrl Pts',(10.1203846153817,-2.67404531641151,1.61651716219696));
#15255=CARTESIAN_POINT('Ctrl Pts',(10.1360897435867,-2.75527937991822,1.48179891776845));
#15256=CARTESIAN_POINT('Ctrl Pts',(10.1517948717933,-2.82635571584919,1.34097710458913));
#15257=CARTESIAN_POINT('Ctrl Pts',(10.1675,-2.88658577275698,1.1956628320182));
#15258=CARTESIAN_POINT('Ctrl Pts',(10.1832051282067,-2.94681582966476,1.05034855944727));
#15259=CARTESIAN_POINT('Ctrl Pts',(10.1989102564133,-2.99620426616754,0.900527828411019));
#15260=CARTESIAN_POINT('Ctrl Pts',(10.2146153846183,-3.03402009771087,0.747818590164109));
#15261=CARTESIAN_POINT('Ctrl Pts',(10.2234102328711,-3.05519690668902,0.662301645657736));
#15262=CARTESIAN_POINT('Ctrl Pts',(10.2322050811233,-3.07274362189332,0.575877627491373));
#15263=CARTESIAN_POINT('Ctrl Pts',(10.2409999293756,-3.0865260643595,0.488857703250772));
#15264=CARTESIAN_POINT('Ctrl Pts',(10.2479102093275,-3.09735519217732,0.420484489677666));
#15265=CARTESIAN_POINT('Ctrl Pts',(10.2548204892794,-3.10586055333669,0.351743453374736));
#15266=CARTESIAN_POINT('Ctrl Pts',(10.2617307692317,-3.11205714799648,0.282798238157759));
#15267=CARTESIAN_POINT('Ctrl Pts',(10.2774358974367,-3.12614026969902,0.126105101036856));
#15268=CARTESIAN_POINT('Ctrl Pts',(10.2931410256434,-3.12830002883756,-0.0316368087400947));
#15269=CARTESIAN_POINT('Ctrl Pts',(10.3088461538485,-3.11873422241136,-0.188648419771246));
#15270=CARTESIAN_POINT('Ctrl Pts',(10.3245512820534,-3.10916841598527,-0.345660030800766));
#15271=CARTESIAN_POINT('Ctrl Pts',(10.3402564102566,-3.08787818772652,-0.50195613408048));
#15272=CARTESIAN_POINT('Ctrl Pts',(10.3559615384615,-3.05502438429765,-0.65579895275087));
#15273=CARTESIAN_POINT('Ctrl Pts',(10.3707243508191,-3.02414182613406,-0.800411122417126));
#15274=CARTESIAN_POINT('Ctrl Pts',(10.3854871631782,-2.98303392179023,-0.942866889012677));
#15275=CARTESIAN_POINT('Ctrl Pts',(10.4002499755359,-2.93184792475783,-1.08161580336685));
#15276=CARTESIAN_POINT('Ctrl Pts',(10.4011922913834,-2.92858070337733,-1.09047219858785));
#15277=CARTESIAN_POINT('Ctrl Pts',(10.4021346072309,-2.92527242968113,-1.0993134924454));
#15278=CARTESIAN_POINT('Ctrl Pts',(10.4030769230783,-2.92192333127634,-1.10813935100346));
#15279=CARTESIAN_POINT('Ctrl Pts',(10.4187820512833,-2.8661055076018,-1.25523572060092));
#15280=CARTESIAN_POINT('Ctrl Pts',(10.4344871794867,-2.79895807188958,-1.3980126906426));
#15281=CARTESIAN_POINT('Ctrl Pts',(10.4501923076917,-2.72154967470354,-1.53495847225753));
#15282=CARTESIAN_POINT('Ctrl Pts',(10.4658974358967,-2.6441412775175,-1.67190425387246));
#15283=CARTESIAN_POINT('Ctrl Pts',(10.4816025641033,-2.55646931412381,-1.80303404218782));
#15284=CARTESIAN_POINT('Ctrl Pts',(10.4973076923083,-2.45953351178131,-1.92692186650602));
#15285=CARTESIAN_POINT('Ctrl Pts',(10.5130128205133,-2.3625977094388,-2.05080969082422));
#15286=CARTESIAN_POINT('Ctrl Pts',(10.5287179487167,-2.25638664196914,-2.16746520831446));
#15287=CARTESIAN_POINT('Ctrl Pts',(10.5444230769217,-2.14191592065938,-2.27539299236912));
#15288=CARTESIAN_POINT('Ctrl Pts',(10.5494487728206,-2.10528488988284,-2.30993026036321));
#15289=CARTESIAN_POINT('Ctrl Pts',(10.5544744687196,-2.0678091870461,-2.34357256496936));
#15290=CARTESIAN_POINT('Ctrl Pts',(10.5595001646187,-2.02952515103173,-2.37626864249984));
#15291=CARTESIAN_POINT('Ctrl Pts',(10.5701795969254,-1.94817288076942,-2.44574669164748));
#15292=CARTESIAN_POINT('Ctrl Pts',(10.5808590292323,-1.86317013579029,-2.51095134091135));
#15293=CARTESIAN_POINT('Ctrl Pts',(10.5915384615385,-1.7750601494579,-2.57161807835228));
#15294=CARTESIAN_POINT('Ctrl Pts',(10.6072435897434,-1.64548597436975,-2.66083432711599));
#15295=CARTESIAN_POINT('Ctrl Pts',(10.6229487179466,-1.509186930649,-2.74024633660057));
#15296=CARTESIAN_POINT('Ctrl Pts',(10.6386538461515,-1.36775803719504,-2.80910392412142));
#15297=CARTESIAN_POINT('Ctrl Pts',(10.6543589743566,-1.22632914373961,-2.87796151164299));
#15298=CARTESIAN_POINT('Ctrl Pts',(10.6700641025633,-1.07975715593558,-2.9362712759061));
#15299=CARTESIAN_POINT('Ctrl Pts',(10.6857692307683,-0.929617596829541,
-2.98324879794393));
#15300=CARTESIAN_POINT('Ctrl Pts',(10.6967627558707,-0.82452052341797,-3.01613287001461));
#15301=CARTESIAN_POINT('Ctrl Pts',(10.7077562809724,-0.717669381189646,
-3.04346332885533));
#15302=CARTESIAN_POINT('Ctrl Pts',(10.718749806074,-0.609657256300376,-3.06495400126008));
#15303=CARTESIAN_POINT('Ctrl Pts',(10.7234614091763,-0.563365438343646,
-3.07416446995282));
#15304=CARTESIAN_POINT('Ctrl Pts',(10.7281730122785,-0.516860431844721,
-3.08230245321972));
#15305=CARTESIAN_POINT('Ctrl Pts',(10.7328846153808,-0.470193579471047,
-3.08937038670253));
#15306=CARTESIAN_POINT('Ctrl Pts',(10.748589743585,-0.31463953905291,-3.112929841749));
#15307=CARTESIAN_POINT('Ctrl Pts',(10.76429487179,-0.157306535044493,-3.12459764304402));
#15308=CARTESIAN_POINT('Ctrl Pts',(10.78,-3.21695909424879E-7,-3.12449703095644));
#15309=CARTESIAN_POINT('Ctrl Pts',(5.825978862952,0.9656781074217,2.972051613422));
#15310=CARTESIAN_POINT('Ctrl Pts',(5.879062196285,0.4599252670358,3.136380672689));
#15311=CARTESIAN_POINT('Ctrl Pts',(5.985228862952,-0.6366272854614,3.200971110614));
#15312=CARTESIAN_POINT('Ctrl Pts',(6.144478862952,-2.119635939241,2.481754111378));
#15313=CARTESIAN_POINT('Ctrl Pts',(6.303728862952,-3.061979863765,1.129624298873));
#15314=CARTESIAN_POINT('Ctrl Pts',(6.462978862952,-3.223532154246,-0.5105564866689));
#15315=CARTESIAN_POINT('Ctrl Pts',(6.622228862952,-2.563047905408,-2.020544571702));
#15316=CARTESIAN_POINT('Ctrl Pts',(6.781478862952,-1.248968678135,-3.015276776083));
#15317=CARTESIAN_POINT('Ctrl Pts',(6.940728862952,0.383608261101,-3.241089558554));
#15318=CARTESIAN_POINT('Ctrl Pts',(7.099978862952,1.918361836065,-2.640398557608));
#15319=CARTESIAN_POINT('Ctrl Pts',(7.259228862952,2.963917875123,-1.366384855545));
#15320=CARTESIAN_POINT('Ctrl Pts',(7.418478862952,3.253651172662,0.256067900963));
#15321=CARTESIAN_POINT('Ctrl Pts',(7.577728862952,2.713677441724,1.813221296591));
#15322=CARTESIAN_POINT('Ctrl Pts',(7.736978862952,1.481694291113,2.907988781792));
#15323=CARTESIAN_POINT('Ctrl Pts',(7.896228862952,-0.1281327360592,3.261195904774));
#15324=CARTESIAN_POINT('Ctrl Pts',(8.055478862952,-1.705284892359,2.782772028626));
#15325=CARTESIAN_POINT('Ctrl Pts',(8.214728862952,-2.84757578293,1.59471906236));
#15326=CARTESIAN_POINT('Ctrl Pts',(8.373978862952,-3.263712108535,0.));
#15327=CARTESIAN_POINT('Ctrl Pts',(8.533228862952,-2.84757578293,-1.59471906236));
#15328=CARTESIAN_POINT('Ctrl Pts',(8.692478862952,-1.705284892359,-2.782772028626));
#15329=CARTESIAN_POINT('Ctrl Pts',(8.851728862952,-0.1281327360592,-3.261195904774));
#15330=CARTESIAN_POINT('Ctrl Pts',(9.010978862952,1.481694291113,-2.907988781792));
#15331=CARTESIAN_POINT('Ctrl Pts',(9.170228862952,2.713677441724,-1.813221296591));
#15332=CARTESIAN_POINT('Ctrl Pts',(9.329478862952,3.253651172662,-0.256067900963));
#15333=CARTESIAN_POINT('Ctrl Pts',(9.488728862952,2.963917875123,1.366384855545));
#15334=CARTESIAN_POINT('Ctrl Pts',(9.647978862952,1.918361836065,2.640398557608));
#15335=CARTESIAN_POINT('Ctrl Pts',(9.807228862952,0.383608261101,3.241089558554));
#15336=CARTESIAN_POINT('Ctrl Pts',(9.966478862952,-1.248968678135,3.015276776083));
#15337=CARTESIAN_POINT('Ctrl Pts',(10.12572886295,-2.563047905408,2.020544571702));
#15338=CARTESIAN_POINT('Ctrl Pts',(10.28497886295,-3.223532154246,0.5105564866689));
#15339=CARTESIAN_POINT('Ctrl Pts',(10.44422886295,-3.061979863765,-1.129624298873));
#15340=CARTESIAN_POINT('Ctrl Pts',(10.60347886295,-2.119635939241,-2.481754111378));
#15341=CARTESIAN_POINT('Ctrl Pts',(10.76272886295,-0.6366272854614,-3.200971110614));
#15342=CARTESIAN_POINT('Ctrl Pts',(10.86889552962,0.4599252670358,-3.136380672689));
#15343=CARTESIAN_POINT('Ctrl Pts',(10.92197886295,0.9656781074217,-2.972051613422));
#15344=CARTESIAN_POINT('Ctrl Pts',(5.714992954317,0.9656781074217,2.972051613422));
#15345=CARTESIAN_POINT('Ctrl Pts',(5.768076287651,0.4599252670358,3.136380672689));
#15346=CARTESIAN_POINT('Ctrl Pts',(5.874242954317,-0.6366272854614,3.200971110614));
#15347=CARTESIAN_POINT('Ctrl Pts',(6.033492954317,-2.119635939241,2.481754111378));
#15348=CARTESIAN_POINT('Ctrl Pts',(6.192742954317,-3.061979863765,1.129624298873));
#15349=CARTESIAN_POINT('Ctrl Pts',(6.351992954317,-3.223532154246,-0.5105564866689));
#15350=CARTESIAN_POINT('Ctrl Pts',(6.511242954317,-2.563047905408,-2.020544571702));
#15351=CARTESIAN_POINT('Ctrl Pts',(6.670492954317,-1.248968678135,-3.015276776083));
#15352=CARTESIAN_POINT('Ctrl Pts',(6.829742954317,0.383608261101,-3.241089558554));
#15353=CARTESIAN_POINT('Ctrl Pts',(6.988992954317,1.918361836065,-2.640398557608));
#15354=CARTESIAN_POINT('Ctrl Pts',(7.148242954317,2.963917875123,-1.366384855545));
#15355=CARTESIAN_POINT('Ctrl Pts',(7.307492954317,3.253651172662,0.256067900963));
#15356=CARTESIAN_POINT('Ctrl Pts',(7.466742954317,2.713677441724,1.813221296591));
#15357=CARTESIAN_POINT('Ctrl Pts',(7.625992954317,1.481694291113,2.907988781792));
#15358=CARTESIAN_POINT('Ctrl Pts',(7.785242954317,-0.1281327360592,3.261195904774));
#15359=CARTESIAN_POINT('Ctrl Pts',(7.944492954317,-1.705284892359,2.782772028626));
#15360=CARTESIAN_POINT('Ctrl Pts',(8.103742954317,-2.84757578293,1.59471906236));
#15361=CARTESIAN_POINT('Ctrl Pts',(8.262992954317,-3.263712108535,0.));
#15362=CARTESIAN_POINT('Ctrl Pts',(8.422242954317,-2.84757578293,-1.59471906236));
#15363=CARTESIAN_POINT('Ctrl Pts',(8.581492954317,-1.705284892359,-2.782772028626));
#15364=CARTESIAN_POINT('Ctrl Pts',(8.740742954317,-0.1281327360592,-3.261195904774));
#15365=CARTESIAN_POINT('Ctrl Pts',(8.899992954317,1.481694291113,-2.907988781792));
#15366=CARTESIAN_POINT('Ctrl Pts',(9.059242954317,2.713677441724,-1.813221296591));
#15367=CARTESIAN_POINT('Ctrl Pts',(9.218492954317,3.253651172662,-0.256067900963));
#15368=CARTESIAN_POINT('Ctrl Pts',(9.377742954317,2.963917875123,1.366384855545));
#15369=CARTESIAN_POINT('Ctrl Pts',(9.536992954317,1.918361836065,2.640398557608));
#15370=CARTESIAN_POINT('Ctrl Pts',(9.696242954317,0.383608261101,3.241089558554));
#15371=CARTESIAN_POINT('Ctrl Pts',(9.855492954317,-1.248968678135,3.015276776083));
#15372=CARTESIAN_POINT('Ctrl Pts',(10.01474295432,-2.563047905408,2.020544571702));
#15373=CARTESIAN_POINT('Ctrl Pts',(10.17399295432,-3.223532154246,0.5105564866689));
#15374=CARTESIAN_POINT('Ctrl Pts',(10.33324295432,-3.061979863765,-1.129624298873));
#15375=CARTESIAN_POINT('Ctrl Pts',(10.49249295432,-2.119635939241,-2.481754111378));
#15376=CARTESIAN_POINT('Ctrl Pts',(10.65174295432,-0.6366272854614,-3.200971110614));
#15377=CARTESIAN_POINT('Ctrl Pts',(10.75790962098,0.4599252670358,-3.136380672689));
#15378=CARTESIAN_POINT('Ctrl Pts',(10.81099295432,0.9656781074217,-2.972051613422));
#15379=CARTESIAN_POINT('Ctrl Pts',(5.604007045683,0.9656781074217,2.972051613422));
#15380=CARTESIAN_POINT('Ctrl Pts',(5.657090379016,0.4599252670358,3.136380672689));
#15381=CARTESIAN_POINT('Ctrl Pts',(5.763257045683,-0.6366272854614,3.200971110614));
#15382=CARTESIAN_POINT('Ctrl Pts',(5.922507045683,-2.119635939241,2.481754111378));
#15383=CARTESIAN_POINT('Ctrl Pts',(6.081757045683,-3.061979863765,1.129624298873));
#15384=CARTESIAN_POINT('Ctrl Pts',(6.241007045683,-3.223532154246,-0.5105564866689));
#15385=CARTESIAN_POINT('Ctrl Pts',(6.400257045683,-2.563047905408,-2.020544571702));
#15386=CARTESIAN_POINT('Ctrl Pts',(6.559507045683,-1.248968678135,-3.015276776083));
#15387=CARTESIAN_POINT('Ctrl Pts',(6.718757045683,0.383608261101,-3.241089558554));
#15388=CARTESIAN_POINT('Ctrl Pts',(6.878007045683,1.918361836065,-2.640398557608));
#15389=CARTESIAN_POINT('Ctrl Pts',(7.037257045683,2.963917875123,-1.366384855545));
#15390=CARTESIAN_POINT('Ctrl Pts',(7.196507045683,3.253651172662,0.256067900963));
#15391=CARTESIAN_POINT('Ctrl Pts',(7.355757045683,2.713677441724,1.813221296591));
#15392=CARTESIAN_POINT('Ctrl Pts',(7.515007045683,1.481694291113,2.907988781792));
#15393=CARTESIAN_POINT('Ctrl Pts',(7.674257045683,-0.1281327360592,3.261195904774));
#15394=CARTESIAN_POINT('Ctrl Pts',(7.833507045683,-1.705284892359,2.782772028626));
#15395=CARTESIAN_POINT('Ctrl Pts',(7.992757045683,-2.84757578293,1.59471906236));
#15396=CARTESIAN_POINT('Ctrl Pts',(8.152007045683,-3.263712108535,0.));
#15397=CARTESIAN_POINT('Ctrl Pts',(8.311257045683,-2.84757578293,-1.59471906236));
#15398=CARTESIAN_POINT('Ctrl Pts',(8.470507045683,-1.705284892359,-2.782772028626));
#15399=CARTESIAN_POINT('Ctrl Pts',(8.629757045683,-0.1281327360592,-3.261195904774));
#15400=CARTESIAN_POINT('Ctrl Pts',(8.789007045683,1.481694291113,-2.907988781792));
#15401=CARTESIAN_POINT('Ctrl Pts',(8.948257045683,2.713677441724,-1.813221296591));
#15402=CARTESIAN_POINT('Ctrl Pts',(9.107507045683,3.253651172662,-0.256067900963));
#15403=CARTESIAN_POINT('Ctrl Pts',(9.266757045683,2.963917875123,1.366384855545));
#15404=CARTESIAN_POINT('Ctrl Pts',(9.426007045683,1.918361836065,2.640398557608));
#15405=CARTESIAN_POINT('Ctrl Pts',(9.585257045683,0.383608261101,3.241089558554));
#15406=CARTESIAN_POINT('Ctrl Pts',(9.744507045683,-1.248968678135,3.015276776083));
#15407=CARTESIAN_POINT('Ctrl Pts',(9.903757045683,-2.563047905408,2.020544571702));
#15408=CARTESIAN_POINT('Ctrl Pts',(10.06300704568,-3.223532154246,0.5105564866689));
#15409=CARTESIAN_POINT('Ctrl Pts',(10.22225704568,-3.061979863765,-1.129624298873));
#15410=CARTESIAN_POINT('Ctrl Pts',(10.38150704568,-2.119635939241,-2.481754111378));
#15411=CARTESIAN_POINT('Ctrl Pts',(10.54075704568,-0.6366272854614,-3.200971110614));
#15412=CARTESIAN_POINT('Ctrl Pts',(10.64692371235,0.4599252670358,-3.136380672689));
#15413=CARTESIAN_POINT('Ctrl Pts',(10.70000704568,0.9656781074217,-2.972051613422));
#15414=CARTESIAN_POINT('Ctrl Pts',(5.493021137048,0.9656781074217,2.972051613422));
#15415=CARTESIAN_POINT('Ctrl Pts',(5.546104470382,0.4599252670358,3.136380672689));
#15416=CARTESIAN_POINT('Ctrl Pts',(5.652271137048,-0.6366272854614,3.200971110614));
#15417=CARTESIAN_POINT('Ctrl Pts',(5.811521137048,-2.119635939241,2.481754111378));
#15418=CARTESIAN_POINT('Ctrl Pts',(5.970771137048,-3.061979863765,1.129624298873));
#15419=CARTESIAN_POINT('Ctrl Pts',(6.130021137048,-3.223532154246,-0.5105564866689));
#15420=CARTESIAN_POINT('Ctrl Pts',(6.289271137048,-2.563047905408,-2.020544571702));
#15421=CARTESIAN_POINT('Ctrl Pts',(6.448521137048,-1.248968678135,-3.015276776083));
#15422=CARTESIAN_POINT('Ctrl Pts',(6.607771137048,0.383608261101,-3.241089558554));
#15423=CARTESIAN_POINT('Ctrl Pts',(6.767021137048,1.918361836065,-2.640398557608));
#15424=CARTESIAN_POINT('Ctrl Pts',(6.926271137048,2.963917875123,-1.366384855545));
#15425=CARTESIAN_POINT('Ctrl Pts',(7.085521137048,3.253651172662,0.256067900963));
#15426=CARTESIAN_POINT('Ctrl Pts',(7.244771137048,2.713677441724,1.813221296591));
#15427=CARTESIAN_POINT('Ctrl Pts',(7.404021137048,1.481694291113,2.907988781792));
#15428=CARTESIAN_POINT('Ctrl Pts',(7.563271137048,-0.1281327360592,3.261195904774));
#15429=CARTESIAN_POINT('Ctrl Pts',(7.722521137048,-1.705284892359,2.782772028626));
#15430=CARTESIAN_POINT('Ctrl Pts',(7.881771137048,-2.84757578293,1.59471906236));
#15431=CARTESIAN_POINT('Ctrl Pts',(8.041021137048,-3.263712108535,0.));
#15432=CARTESIAN_POINT('Ctrl Pts',(8.200271137048,-2.84757578293,-1.59471906236));
#15433=CARTESIAN_POINT('Ctrl Pts',(8.359521137048,-1.705284892359,-2.782772028626));
#15434=CARTESIAN_POINT('Ctrl Pts',(8.518771137048,-0.1281327360592,-3.261195904774));
#15435=CARTESIAN_POINT('Ctrl Pts',(8.678021137048,1.481694291113,-2.907988781792));
#15436=CARTESIAN_POINT('Ctrl Pts',(8.837271137048,2.713677441724,-1.813221296591));
#15437=CARTESIAN_POINT('Ctrl Pts',(8.996521137048,3.253651172662,-0.256067900963));
#15438=CARTESIAN_POINT('Ctrl Pts',(9.155771137048,2.963917875123,1.366384855545));
#15439=CARTESIAN_POINT('Ctrl Pts',(9.315021137048,1.918361836065,2.640398557608));
#15440=CARTESIAN_POINT('Ctrl Pts',(9.474271137048,0.383608261101,3.241089558554));
#15441=CARTESIAN_POINT('Ctrl Pts',(9.633521137048,-1.248968678135,3.015276776083));
#15442=CARTESIAN_POINT('Ctrl Pts',(9.792771137048,-2.563047905408,2.020544571702));
#15443=CARTESIAN_POINT('Ctrl Pts',(9.952021137048,-3.223532154246,0.5105564866689));
#15444=CARTESIAN_POINT('Ctrl Pts',(10.11127113705,-3.061979863765,-1.129624298873));
#15445=CARTESIAN_POINT('Ctrl Pts',(10.27052113705,-2.119635939241,-2.481754111378));
#15446=CARTESIAN_POINT('Ctrl Pts',(10.42977113705,-0.6366272854614,-3.200971110614));
#15447=CARTESIAN_POINT('Ctrl Pts',(10.53593780372,0.4599252670358,-3.136380672689));
#15448=CARTESIAN_POINT('Ctrl Pts',(10.58902113705,0.9656781074217,-2.972051613422));
#15449=CARTESIAN_POINT('Origin',(32.48,0.,0.));
#15450=CARTESIAN_POINT('',(32.48,-1.1719681554584,0.434730540210171));
#15451=CARTESIAN_POINT('',(32.48,0.,-1.25));
#15452=CARTESIAN_POINT('Origin',(32.48,0.,0.));
#15453=CARTESIAN_POINT('',(32.48,-2.14581966314199E-13,-1.01129910075941));
#15454=CARTESIAN_POINT('',(32.48,0.,-1.25));
#15455=CARTESIAN_POINT('',(32.4802091864294,-1.17417484703353,0.42767483665679));
#15456=CARTESIAN_POINT('Ctrl Pts',(32.48,-1.17383720045579,0.427540834752428));
#15457=CARTESIAN_POINT('Ctrl Pts',(32.48,-1.20334957755843,0.312634815856706));
#15458=CARTESIAN_POINT('Ctrl Pts',(32.4800000000088,-1.21675226571292,0.19356365786419));
#15459=CARTESIAN_POINT('Ctrl Pts',(32.4800000000088,-1.20746725502762,-0.0403383382890132));
#15460=CARTESIAN_POINT('Ctrl Pts',(32.4800000000088,-1.18562847337316,-0.154733104489758));
#15461=CARTESIAN_POINT('Ctrl Pts',(32.4800000000088,-1.10111226718253,-0.400206118254704));
#15462=CARTESIAN_POINT('Ctrl Pts',(32.4800000000088,-1.02915837108193,-0.528561609151227));
#15463=CARTESIAN_POINT('Ctrl Pts',(32.4800000000088,-0.830791286197287,
-0.76065705947605));
#15464=CARTESIAN_POINT('Ctrl Pts',(32.4800000000088,-0.714027251240835,
-0.842690493865625));
#15465=CARTESIAN_POINT('Ctrl Pts',(32.4800000000088,-0.51664509754878,-0.946705547829938));
#15466=CARTESIAN_POINT('Ctrl Pts',(32.4800000000088,-0.414397116935866,
-0.982897616104408));
#15467=CARTESIAN_POINT('Ctrl Pts',(32.4800000000088,-0.20674106525062,-1.02124569796361));
#15468=CARTESIAN_POINT('Ctrl Pts',(32.48,-0.103645908104796,-1.02416362464409));
#15469=CARTESIAN_POINT('Ctrl Pts',(32.48,-2.15071016551605E-13,-1.0112991007594));
#15470=CARTESIAN_POINT('Ctrl Pts',(32.4802091864294,-1.17451603719175,0.427799109839404));
#15471=CARTESIAN_POINT('Ctrl Pts',(32.4801394576196,-1.17367357079685,0.430112088685898));
#15472=CARTESIAN_POINT('Ctrl Pts',(32.4800697288098,-1.17282427194519,0.43242257891675));
#15473=CARTESIAN_POINT('Ctrl Pts',(32.48,-1.1719681554584,0.434730540210171));
#15474=CARTESIAN_POINT('Origin',(32.48,0.,0.));
#15475=CARTESIAN_POINT('',(32.1675060170811,-9.34798452714434E-6,-1.24978906897538));
#15476=CARTESIAN_POINT('Ctrl Pts',(32.1676274246727,-1.60399786011158E-5,
-1.24999999989709));
#15477=CARTESIAN_POINT('Ctrl Pts',(32.173598380776,0.101438842794184,-1.25000130176441));
#15478=CARTESIAN_POINT('Ctrl Pts',(32.1795714326686,0.202526354544554,-1.2376506761652));
#15479=CARTESIAN_POINT('Ctrl Pts',(32.1896850767944,0.374326908675496,-1.19502535756305));
#15480=CARTESIAN_POINT('Ctrl Pts',(32.1938937983711,0.445845258510437,-1.1702260433228));
#15481=CARTESIAN_POINT('Ctrl Pts',(32.2022210789359,0.582164826348471,-1.10863277573242));
#15482=CARTESIAN_POINT('Ctrl Pts',(32.206334668102,0.646791699941685,-1.07221388529247));
#15483=CARTESIAN_POINT('Ctrl Pts',(32.2162391802242,0.787720814155092,-0.975394050833982));
#15484=CARTESIAN_POINT('Ctrl Pts',(32.2220182599191,0.860966724127556,-0.911391666503034));
#15485=CARTESIAN_POINT('Ctrl Pts',(32.2349867690631,1.01056382152689,-0.746379439126566));
#15486=CARTESIAN_POINT('Ctrl Pts',(32.2419708632708,1.08050014479524,-0.640970847678421));
#15487=CARTESIAN_POINT('Ctrl Pts',(32.2526890486056,1.16157362526215,-0.466556119290835));
#15488=CARTESIAN_POINT('Ctrl Pts',(32.256422258516,1.18475666984318,-0.40407812892699));
#15489=CARTESIAN_POINT('Ctrl Pts',(32.2659674336806,1.22941045910993,-0.246123517505284));
#15490=CARTESIAN_POINT('Ctrl Pts',(32.271780145632,1.24487129761986,-0.149410654725891));
#15491=CARTESIAN_POINT('Ctrl Pts',(32.2859186906479,1.25497749106622,0.0938655035164218));
#15492=CARTESIAN_POINT('Ctrl Pts',(32.2938682048,1.23547411642577,0.239545986671451));
#15493=CARTESIAN_POINT('Ctrl Pts',(32.3059208801052,1.17059722602897,0.44370420020077));
#15494=CARTESIAN_POINT('Ctrl Pts',(32.3098837877495,1.14459344270278,0.507025730539694));
#15495=CARTESIAN_POINT('Ctrl Pts',(32.3173248114395,1.08715439549203,0.619653609883257));
#15496=CARTESIAN_POINT('Ctrl Pts',(32.3207565858864,1.05718301811824,0.669506992419299));
#15497=CARTESIAN_POINT('Ctrl Pts',(32.3310964721333,0.955559897167941,0.814602243645237));
#15498=CARTESIAN_POINT('Ctrl Pts',(32.337764005247,0.873685600999364,0.901858257853645));
#15499=CARTESIAN_POINT('Ctrl Pts',(32.3492547954888,0.712478996094717,1.03077898081134));
#15500=CARTESIAN_POINT('Ctrl Pts',(32.354132063387,0.638731111457185,1.07803216370618));
#15501=CARTESIAN_POINT('Ctrl Pts',(32.3677278070184,0.430804719901573,1.18237689339029));
#15502=CARTESIAN_POINT('Ctrl Pts',(32.3763140626297,0.290556856108505,1.22441585209194));
#15503=CARTESIAN_POINT('Ctrl Pts',(32.3899887212276,0.0499212726420179,
1.25276221308346));
#15504=CARTESIAN_POINT('Ctrl Pts',(32.3952913518613,-0.0473830247951738,
1.25286037601624));
#15505=CARTESIAN_POINT('Ctrl Pts',(32.4046759695241,-0.212324572615296,
1.23377004596013));
#15506=CARTESIAN_POINT('Ctrl Pts',(32.4087137640163,-0.280149151477129,
1.22015755740893));
#15507=CARTESIAN_POINT('Ctrl Pts',(32.4201985488141,-0.4674169888626,1.16613067923734));
#15508=CARTESIAN_POINT('Ctrl Pts',(32.42752145001,-0.582393583035011,1.1131771414791));
#15509=CARTESIAN_POINT('Ctrl Pts',(32.4400656595717,-0.768674742918102,
0.990495494343983));
#15510=CARTESIAN_POINT('Ctrl Pts',(32.4453720504446,-0.843314336264057,
0.927772317335062));
#15511=CARTESIAN_POINT('Ctrl Pts',(32.4552603593318,-0.962519242690118,
0.801211161419528));
#15512=CARTESIAN_POINT('Ctrl Pts',(32.4597919513534,-1.00985081030901,0.740662982862584));
#15513=CARTESIAN_POINT('Ctrl Pts',(32.4696271054798,-1.10014034401452,0.600277310531608));
#15514=CARTESIAN_POINT('Ctrl Pts',(32.4748779535446,-1.14058809545123,0.519326462610753));
#15515=CARTESIAN_POINT('Ctrl Pts',(32.48,-1.1719681554584,0.434730540210171));
#15516=CARTESIAN_POINT('',(32.48,0.,-1.25));
#15517=CARTESIAN_POINT('Origin',(32.48,0.,-1.25));
#15518=CARTESIAN_POINT('',(32.3083865332472,-1.15233060718194E-10,-1.00548172098699));
#15519=CARTESIAN_POINT('Ctrl Pts',(32.3083865336658,6.75598583770804E-18,
-1.00548172122881));
#15520=CARTESIAN_POINT('Ctrl Pts',(32.2848226217472,2.79433020236803E-15,
-1.04627458705313));
#15521=CARTESIAN_POINT('Ctrl Pts',(32.2612587098288,2.84235642030823E-12,
-1.08706745287754));
#15522=CARTESIAN_POINT('Ctrl Pts',(32.2142255996871,2.84235642030823E-12,
-1.16848922011001));
#15523=CARTESIAN_POINT('Ctrl Pts',(32.1907564014637,1.40940692139627E-14,
-1.20911812151808));
#15524=CARTESIAN_POINT('Ctrl Pts',(32.1672872032404,4.46512479480176E-17,
-1.24974702292624));
#15525=CARTESIAN_POINT('',(32.4766396034691,1.02451809110596E-10,-1.00548172094448));
#15526=CARTESIAN_POINT('Ctrl Pts',(32.4766396034691,1.97433788701479E-19,
-1.00548172051374));
#15527=CARTESIAN_POINT('Ctrl Pts',(32.4485930689794,2.17707619891981E-17,
-1.00548172051374));
#15528=CARTESIAN_POINT('Ctrl Pts',(32.4205465344897,1.80411241501588E-15,
-1.00548172051374));
#15529=CARTESIAN_POINT('Ctrl Pts',(32.3644621777491,1.80411241501588E-15,
-1.00548172051374));
#15530=CARTESIAN_POINT('Ctrl Pts',(32.3364243554981,2.28527355790286E-17,
-1.00548172051374));
#15531=CARTESIAN_POINT('Ctrl Pts',(32.3083865332471,2.17567656864905E-19,
-1.00548172051374));
#15532=CARTESIAN_POINT('Ctrl Pts',(32.48,-4.28248633902167E-13,-1.01129910075941));
#15533=CARTESIAN_POINT('Ctrl Pts',(32.4795160656876,-1.34558093608641E-12,
-1.01046133377316));
#15534=CARTESIAN_POINT('Ctrl Pts',(32.4790321313751,-3.41777979044421E-12,
-1.00962356678695));
#15535=CARTESIAN_POINT('Ctrl Pts',(32.4779119990709,-3.41777979044421E-12,
-1.00768444025543));
#15536=CARTESIAN_POINT('Ctrl Pts',(32.4772758010794,-1.44173449374501E-13,
-1.00658308071008));
#15537=CARTESIAN_POINT('Ctrl Pts',(32.4766396030876,-4.57272161567443E-15,
-1.00548172116484));
#15538=CARTESIAN_POINT('Ctrl Pts',(32.66948943148,0.523912106125,-1.17672585665));
#15539=CARTESIAN_POINT('Ctrl Pts',(32.65323943148,0.2569214784303,-1.295597742809));
#15540=CARTESIAN_POINT('Ctrl Pts',(32.62073943148,-0.3599776781819,-1.343968209978));
#15541=CARTESIAN_POINT('Ctrl Pts',(32.57198943148,-1.125748737002,-0.8178925633062));
#15542=CARTESIAN_POINT('Ctrl Pts',(32.52323943148,-1.389532103288,0.07282787068193));
#15543=CARTESIAN_POINT('Ctrl Pts',(32.47448943148,-1.034052055861,0.9310606109295));
#15544=CARTESIAN_POINT('Ctrl Pts',(32.42573943148,-0.2176699703233,1.374319545129));
#15545=CARTESIAN_POINT('Ctrl Pts',(32.37698943148,0.6957249084782,1.205031167107));
#15546=CARTESIAN_POINT('Ctrl Pts',(32.32823943148,1.299030774048,0.4986511981073));
#15547=CARTESIAN_POINT('Ctrl Pts',(32.27948943148,1.323347810262,-0.4299817804464));
#15548=CARTESIAN_POINT('Ctrl Pts',(32.23073943148,0.7578381246551,-1.166968368163));
#15549=CARTESIAN_POINT('Ctrl Pts',(32.18198943148,-0.14544615728,-1.383827738746));
#15550=CARTESIAN_POINT('Ctrl Pts',(32.13323943148,-0.9839039059594,-0.9839039061246));
#15551=CARTESIAN_POINT('Ctrl Pts',(32.08448943148,-1.383827738331,-0.1454461562038));
#15552=CARTESIAN_POINT('Ctrl Pts',(32.03573943148,-1.166968369989,0.7578381205155));
#15553=CARTESIAN_POINT('Ctrl Pts',(31.98698943148,-0.4299817735579,1.323347825744));
#15554=CARTESIAN_POINT('Ctrl Pts',(31.93823943148,0.4986511723795,1.299030716259));
#15555=CARTESIAN_POINT('Ctrl Pts',(31.88948943148,1.20503126313,0.69572512415));
#15556=CARTESIAN_POINT('Ctrl Pts',(31.84073943148,1.374319186766,-0.217670775222));
#15557=CARTESIAN_POINT('Ctrl Pts',(31.79198943148,0.9310619483586,-1.034049051938));
#15558=CARTESIAN_POINT('Ctrl Pts',(31.74323943148,0.07282287932824,-1.389543314081));
#15559=CARTESIAN_POINT('Ctrl Pts',(31.69448943148,-0.8178739353206,-1.125706897754));
#15560=CARTESIAN_POINT('Ctrl Pts',(31.64573943148,-1.344037730566,-0.3601338243812));
#15561=CARTESIAN_POINT('Ctrl Pts',(31.59698943148,-1.271153054855,0.5659538022856));
#15562=CARTESIAN_POINT('Ctrl Pts',(31.54823943148,-0.6317051899145,1.239791251989));
#15563=CARTESIAN_POINT('Ctrl Pts',(31.49948943148,0.2892987601002,1.361043711953));
#15564=CARTESIAN_POINT('Ctrl Pts',(31.45073943148,1.081359992212,0.8756680515693));
#15565=CARTESIAN_POINT('Ctrl Pts',(31.40198943148,1.391450057306,-1.387658967178E-7));
#15566=CARTESIAN_POINT('Ctrl Pts',(31.35323943148,1.081360653838,-0.8756674965057));
#15567=CARTESIAN_POINT('Ctrl Pts',(31.30448943148,0.2892961135977,-1.361045654676));
#15568=CARTESIAN_POINT('Ctrl Pts',(31.25573943148,-0.6316952655301,-1.239784036163));
#15569=CARTESIAN_POINT('Ctrl Pts',(31.20698943148,-1.271190105891,-0.5659807228689));
#15570=CARTESIAN_POINT('Ctrl Pts',(31.15823943148,-1.34389945081,0.360234290888));
#15571=CARTESIAN_POINT('Ctrl Pts',(31.12573943148,-0.9935598191429,0.8702993985029));
#15572=CARTESIAN_POINT('Ctrl Pts',(31.10948943148,-0.7571184320868,1.04208412158));
#15573=CARTESIAN_POINT('Ctrl Pts',(32.6078719886,0.4805033243013,-1.079228136364));
#15574=CARTESIAN_POINT('Ctrl Pts',(32.5916219886,0.2356342276251,-1.18825088235));
#15575=CARTESIAN_POINT('Ctrl Pts',(32.5591219886,-0.330151697238,-1.232613610374));
#15576=CARTESIAN_POINT('Ctrl Pts',(32.5103719886,-1.032474730272,-0.7501260058613));
#15577=CARTESIAN_POINT('Ctrl Pts',(32.4616219886,-1.274402303455,0.06679371130261));
#15578=CARTESIAN_POINT('Ctrl Pts',(32.4128719886,-0.9483755853946,0.8539175053361));
#15579=CARTESIAN_POINT('Ctrl Pts',(32.3641219886,-0.199634906539,1.260450183087));
#15580=CARTESIAN_POINT('Ctrl Pts',(32.3153719886,0.6380805623973,1.105188207931));
#15581=CARTESIAN_POINT('Ctrl Pts',(32.2666219886,1.191399469495,0.457335410952));
#15582=CARTESIAN_POINT('Ctrl Pts',(32.2178719886,1.21370171562,-0.3943556036939));
#15583=CARTESIAN_POINT('Ctrl Pts',(32.1691219886,0.6950473827993,-1.07027910541));
#15584=CARTESIAN_POINT('Ctrl Pts',(32.1203719886,-0.1333952036284,-1.269170574518));
#15585=CARTESIAN_POINT('Ctrl Pts',(32.0716219886,-0.902382464691,-0.9023824648425));
#15586=CARTESIAN_POINT('Ctrl Pts',(32.0228719886,-1.269170574137,-0.1333952026413));
#15587=CARTESIAN_POINT('Ctrl Pts',(31.9741219886,-1.070279107084,0.6950473790027));
#15588=CARTESIAN_POINT('Ctrl Pts',(31.9253719886,-0.3943555973762,1.213701729819));
#15589=CARTESIAN_POINT('Ctrl Pts',(31.8766219886,0.4573353873559,1.191399416495));
#15590=CARTESIAN_POINT('Ctrl Pts',(31.8278719886,1.105188295998,0.6380807601996));
#15591=CARTESIAN_POINT('Ctrl Pts',(31.7791219886,1.260449854417,-0.1996356447478));
#15592=CARTESIAN_POINT('Ctrl Pts',(31.7303719886,0.8539187319524,-0.948372830362));
#15593=CARTESIAN_POINT('Ctrl Pts',(31.6816219886,0.06678913350795,-1.274412585376));
#15594=CARTESIAN_POINT('Ctrl Pts',(31.6328719886,-0.7501089212991,-1.032436357618));
#15595=CARTESIAN_POINT('Ctrl Pts',(31.5841219886,-1.232677370829,-0.3302949059307));
#15596=CARTESIAN_POINT('Ctrl Pts',(31.5353719886,-1.165831561083,0.519061652174));
#15597=CARTESIAN_POINT('Ctrl Pts',(31.4866219886,-0.5793652030249,1.137068243043));
#15598=CARTESIAN_POINT('Ctrl Pts',(31.4378719886,0.2653288868863,1.248274320191));
#15599=CARTESIAN_POINT('Ctrl Pts',(31.3891219886,0.9917638186823,0.8031145011624));
#15600=CARTESIAN_POINT('Ctrl Pts',(31.3403719886,1.27616134523,-1.272684365758E-7));
#15601=CARTESIAN_POINT('Ctrl Pts',(31.2916219886,0.9917644254889,-0.8031139920886));
#15602=CARTESIAN_POINT('Ctrl Pts',(31.2428719886,0.26532645966,-1.248276101949));
#15603=CARTESIAN_POINT('Ctrl Pts',(31.1941219886,-0.5793561009262,-1.137061625084));
#15604=CARTESIAN_POINT('Ctrl Pts',(31.1453719886,-1.165865542251,-0.5190863422501));
#15605=CARTESIAN_POINT('Ctrl Pts',(31.0966219886,-1.232550548254,0.3303870482766));
#15606=CARTESIAN_POINT('Ctrl Pts',(31.0641219886,-0.9112383363718,0.7981906682994));
#15607=CARTESIAN_POINT('Ctrl Pts',(31.0478719886,-0.6943873204195,0.9557421536299));
#15608=CARTESIAN_POINT('Ctrl Pts',(32.54625454572,0.4370945424777,-0.9817304160777));
#15609=CARTESIAN_POINT('Ctrl Pts',(32.53000454572,0.2143469768198,-1.080904021891));
#15610=CARTESIAN_POINT('Ctrl Pts',(32.49750454572,-0.300325716294,-1.121259010771));
#15611=CARTESIAN_POINT('Ctrl Pts',(32.44875454572,-0.9392007235413,-0.6823594484165));
#15612=CARTESIAN_POINT('Ctrl Pts',(32.40000454572,-1.159272503621,0.06075955192328));
#15613=CARTESIAN_POINT('Ctrl Pts',(32.35125454572,-0.8626991149286,0.7767743997427));
#15614=CARTESIAN_POINT('Ctrl Pts',(32.30250454572,-0.1815998427547,1.146580821045));
#15615=CARTESIAN_POINT('Ctrl Pts',(32.25375454572,0.5804362163164,1.005345248755));
#15616=CARTESIAN_POINT('Ctrl Pts',(32.20500454572,1.083768164943,0.4160196237966));
#15617=CARTESIAN_POINT('Ctrl Pts',(32.15625454572,1.104055620977,-0.3587294269415));
#15618=CARTESIAN_POINT('Ctrl Pts',(32.10750454572,0.6322566409435,-0.9735898426565));
#15619=CARTESIAN_POINT('Ctrl Pts',(32.05875454572,-0.1213442499767,-1.154513410291));
#15620=CARTESIAN_POINT('Ctrl Pts',(32.01000454572,-0.8208610234226,-0.8208610235605));
#15621=CARTESIAN_POINT('Ctrl Pts',(31.96125454572,-1.154513409944,-0.1213442490788));
#15622=CARTESIAN_POINT('Ctrl Pts',(31.91250454572,-0.9735898441798,0.6322566374899));
#15623=CARTESIAN_POINT('Ctrl Pts',(31.86375454572,-0.3587294211945,1.104055633894));
#15624=CARTESIAN_POINT('Ctrl Pts',(31.81500454572,0.4160196023322,1.083768116731));
#15625=CARTESIAN_POINT('Ctrl Pts',(31.76625454572,1.005345328866,0.5804363962492));
#15626=CARTESIAN_POINT('Ctrl Pts',(31.71750454572,1.146580522067,-0.1816005142735));
#15627=CARTESIAN_POINT('Ctrl Pts',(31.66875454572,0.7767755155462,-0.8626966087863));
#15628=CARTESIAN_POINT('Ctrl Pts',(31.62000454572,0.06075538768766,-1.159281856671));
#15629=CARTESIAN_POINT('Ctrl Pts',(31.57125454572,-0.6823439072776,-0.9391658174822));
#15630=CARTESIAN_POINT('Ctrl Pts',(31.52250454572,-1.121317011091,-0.3004559874802));
#15631=CARTESIAN_POINT('Ctrl Pts',(31.47375454572,-1.06051006731,0.4721695020624));
#15632=CARTESIAN_POINT('Ctrl Pts',(31.42500454572,-0.5270252161353,1.034345234097));
#15633=CARTESIAN_POINT('Ctrl Pts',(31.37625454572,0.2413590136724,1.135504928428));
#15634=CARTESIAN_POINT('Ctrl Pts',(31.32750454572,0.9021676451524,0.7305609507554));
#15635=CARTESIAN_POINT('Ctrl Pts',(31.27875454572,1.160872633154,-1.157709766638E-7));
#15636=CARTESIAN_POINT('Ctrl Pts',(31.23000454572,0.9021681971399,-0.7305604876715));
#15637=CARTESIAN_POINT('Ctrl Pts',(31.18125454572,0.2413568057222,-1.135506549222));
#15638=CARTESIAN_POINT('Ctrl Pts',(31.13250454572,-0.5270169363223,-1.034339214006));
#15639=CARTESIAN_POINT('Ctrl Pts',(31.08375454572,-1.060540978612,-0.4721919616313));
#15640=CARTESIAN_POINT('Ctrl Pts',(31.03500454572,-1.121201645697,0.3005398056652));
#15641=CARTESIAN_POINT('Ctrl Pts',(31.00250454572,-0.8289168536006,0.7260819380959));
#15642=CARTESIAN_POINT('Ctrl Pts',(30.98625454572,-0.6316562087523,0.86940018568));
#15643=CARTESIAN_POINT('Ctrl Pts',(32.48463710284,0.393685760654,-0.8842326957913));
#15644=CARTESIAN_POINT('Ctrl Pts',(32.46838710284,0.1930597260145,-0.9735571614325));
#15645=CARTESIAN_POINT('Ctrl Pts',(32.43588710284,-0.2704997353501,-1.009904411168));
#15646=CARTESIAN_POINT('Ctrl Pts',(32.38713710284,-0.845926716811,-0.6145928909716));
#15647=CARTESIAN_POINT('Ctrl Pts',(32.33838710284,-1.044142703787,0.05472539254396));
#15648=CARTESIAN_POINT('Ctrl Pts',(32.28963710284,-0.7770226444626,0.6996312941493));
#15649=CARTESIAN_POINT('Ctrl Pts',(32.24088710284,-0.1635647789704,1.032711459003));
#15650=CARTESIAN_POINT('Ctrl Pts',(32.19213710284,0.5227918702356,0.905502289579));
#15651=CARTESIAN_POINT('Ctrl Pts',(32.14338710284,0.9761368603912,0.3747038366413));
#15652=CARTESIAN_POINT('Ctrl Pts',(32.09463710284,0.994409526335,-0.323103250189));
#15653=CARTESIAN_POINT('Ctrl Pts',(32.04588710284,0.5694658990877,-0.8769005799032));
#15654=CARTESIAN_POINT('Ctrl Pts',(31.99713710284,-0.109293296325,-1.039856246063));
#15655=CARTESIAN_POINT('Ctrl Pts',(31.94838710284,-0.7393395821542,-0.7393395822784));
#15656=CARTESIAN_POINT('Ctrl Pts',(31.89963710284,-1.039856245751,-0.1092932955163));
#15657=CARTESIAN_POINT('Ctrl Pts',(31.85088710284,-0.8769005812753,0.5694658959771));
#15658=CARTESIAN_POINT('Ctrl Pts',(31.80213710284,-0.3231032450128,0.9944095379687));
#15659=CARTESIAN_POINT('Ctrl Pts',(31.75338710284,0.3747038173086,0.9761368169669));
#15660=CARTESIAN_POINT('Ctrl Pts',(31.70463710284,0.9055023617337,0.5227920322988));
#15661=CARTESIAN_POINT('Ctrl Pts',(31.65588710284,1.032711189717,-0.1635653837993));
#15662=CARTESIAN_POINT('Ctrl Pts',(31.60713710284,0.69963229914,-0.7770203872106));
#15663=CARTESIAN_POINT('Ctrl Pts',(31.55838710284,0.05472164186737,-1.044151127966));
#15664=CARTESIAN_POINT('Ctrl Pts',(31.50963710284,-0.614578893256,-0.8458952773463));
#15665=CARTESIAN_POINT('Ctrl Pts',(31.46088710284,-1.009956651354,-0.2706170690297));
#15666=CARTESIAN_POINT('Ctrl Pts',(31.41213710284,-0.9551885735371,0.4252773519508));
#15667=CARTESIAN_POINT('Ctrl Pts',(31.36338710284,-0.4746852292457,0.9316222251505));
#15668=CARTESIAN_POINT('Ctrl Pts',(31.31463710284,0.2173891404585,1.022735536666));
#15669=CARTESIAN_POINT('Ctrl Pts',(31.26588710284,0.8125714716225,0.6580074003485));
#15670=CARTESIAN_POINT('Ctrl Pts',(31.21713710284,1.045583921078,-1.042735165158E-7));
#15671=CARTESIAN_POINT('Ctrl Pts',(31.16838710284,0.8125719687909,-0.6580069832544));
#15672=CARTESIAN_POINT('Ctrl Pts',(31.11963710284,0.2173871517845,-1.022736996495));
#15673=CARTESIAN_POINT('Ctrl Pts',(31.07088710284,-0.4746777717184,-0.9316168029278));
#15674=CARTESIAN_POINT('Ctrl Pts',(31.02213710284,-0.9552164149722,-0.4252975810124));
#15675=CARTESIAN_POINT('Ctrl Pts',(30.97338710284,-1.00985274314,0.2706925630538));
#15676=CARTESIAN_POINT('Ctrl Pts',(30.94088710284,-0.7465953708295,0.6539732078925));
#15677=CARTESIAN_POINT('Ctrl Pts',(30.92463710284,-0.568925097085,0.7830582177302));
#15678=CARTESIAN_POINT('',(30.9766265277784,-0.871221485969368,0.50299995921493));
#15679=CARTESIAN_POINT('Ctrl Pts',(32.4766396027226,1.54919549294486E-10,
-1.0054817205135));
#15680=CARTESIAN_POINT('Ctrl Pts',(32.4691053139096,-0.10582508315099,-1.00564870419041));
#15681=CARTESIAN_POINT('Ctrl Pts',(32.4603459018315,-0.229977486211365,
-0.98986838296787));
#15682=CARTESIAN_POINT('Ctrl Pts',(32.4413683240352,-0.478121855944446,
-0.893142660574254));
#15683=CARTESIAN_POINT('Ctrl Pts',(32.4325422614636,-0.585319685046669,
-0.82656883687245));
#15684=CARTESIAN_POINT('Ctrl Pts',(32.4142572992228,-0.775641550295082,
-0.654100595091286));
#15685=CARTESIAN_POINT('Ctrl Pts',(32.4050118930799,-0.85418371112365,-0.547761809504575));
#15686=CARTESIAN_POINT('Ctrl Pts',(32.3863010258111,-0.965161319461717,
-0.309559370165476));
#15687=CARTESIAN_POINT('Ctrl Pts',(32.3770681843843,-0.997469062168772,
-0.181353499720047));
#15688=CARTESIAN_POINT('Ctrl Pts',(32.3568701808033,-1.01283629382345,0.101717750507541));
#15689=CARTESIAN_POINT('Ctrl Pts',(32.3475047473001,-0.984367566826271,
0.232947114591686));
#15690=CARTESIAN_POINT('Ctrl Pts',(32.3306589696044,-0.904804400397718,
0.45589393306715));
#15691=CARTESIAN_POINT('Ctrl Pts',(32.3216600150562,-0.840300871347811,
0.56722203459221));
#15692=CARTESIAN_POINT('Ctrl Pts',(32.3025520369028,-0.663919325666475,
0.769080055430503));
#15693=CARTESIAN_POINT('Ctrl Pts',(32.2930478380112,-0.553320416471912,
0.848600935605224));
#15694=CARTESIAN_POINT('Ctrl Pts',(32.2764607849827,-0.34391489168562,0.950970008765668));
#15695=CARTESIAN_POINT('Ctrl Pts',(32.267274142459,-0.219359775122067,0.993525782886256));
#15696=CARTESIAN_POINT('Ctrl Pts',(32.2471250024671,0.0627872995112071,
1.01225002509461));
#15697=CARTESIAN_POINT('Ctrl Pts',(32.2377136687343,0.196496573752308,0.994659351660526));
#15698=CARTESIAN_POINT('Ctrl Pts',(32.218820619244,0.448119147312156,0.910386233646112));
#15699=CARTESIAN_POINT('Ctrl Pts',(32.2095672963117,0.562777737133873,0.844344677318313));
#15700=CARTESIAN_POINT('Ctrl Pts',(32.190863687752,0.759894331709125,0.670695233562694));
#15701=CARTESIAN_POINT('Ctrl Pts',(32.1816445339917,0.840830374658885,0.566410881442963));
#15702=CARTESIAN_POINT('Ctrl Pts',(32.1614385161676,0.968593109628251,0.31323629661574));
#15703=CARTESIAN_POINT('Ctrl Pts',(32.152059805267,0.995103645636241,0.181385312576402));
#15704=CARTESIAN_POINT('Ctrl Pts',(32.1352540053896,1.01170308102003,-0.0541913934911884));
#15705=CARTESIAN_POINT('Ctrl Pts',(32.126269951113,0.997390470348591,-0.181830481509641));
#15706=CARTESIAN_POINT('Ctrl Pts',(32.1077447657716,0.919423226898876,-0.429745166292925));
#15707=CARTESIAN_POINT('Ctrl Pts',(32.0982393193792,0.852869094566033,-0.54854223882289));
#15708=CARTESIAN_POINT('Ctrl Pts',(32.0810552458601,0.696891195219596,-0.73288046123264));
#15709=CARTESIAN_POINT('Ctrl Pts',(32.0718646719204,0.599816161628677,-0.821842509043154));
#15710=CARTESIAN_POINT('Ctrl Pts',(32.0517249713863,0.349028087285563,-0.952204354992639));
#15711=CARTESIAN_POINT('Ctrl Pts',(32.0423217182128,0.219635000613399,-0.989799618535102));
#15712=CARTESIAN_POINT('Ctrl Pts',(32.0234223525948,-0.0447199889143717,
-1.01375940902337));
#15713=CARTESIAN_POINT('Ctrl Pts',(32.0141578837072,-0.176402393566581,
-0.99923740432607));
#15714=CARTESIAN_POINT('Ctrl Pts',(31.9954668431444,-0.426500714921258,
-0.919407894705325));
#15715=CARTESIAN_POINT('Ctrl Pts',(31.9862599642796,-0.542364539351686,
-0.856538059210492));
#15716=CARTESIAN_POINT('Ctrl Pts',(31.9660429991874,-0.761220467435554,
-0.675972386498989));
#15717=CARTESIAN_POINT('Ctrl Pts',(31.9566507719093,-0.838493771813703,
-0.565639342750785));
#15718=CARTESIAN_POINT('Ctrl Pts',(31.9398838938876,-0.948125656391315,
-0.357081831558934));
#15719=CARTESIAN_POINT('Ctrl Pts',(31.9309137064797,-0.986297530771061,
-0.234667590561075));
#15720=CARTESIAN_POINT('Ctrl Pts',(31.9124152715538,-1.01458386847578,0.023295661735757));
#15721=CARTESIAN_POINT('Ctrl Pts',(31.9029118555964,-1.00153559313095,0.158814096445736));
#15722=CARTESIAN_POINT('Ctrl Pts',(31.8856873106528,-0.932797546195448,
0.390887587624591));
#15723=CARTESIAN_POINT('Ctrl Pts',(31.8764931007021,-0.879593330129118,
0.511383216351955));
#15724=CARTESIAN_POINT('Ctrl Pts',(31.8563616071714,-0.70241886040258,0.731471621586331));
#15725=CARTESIAN_POINT('Ctrl Pts',(31.8469659290911,-0.599170684072269,
0.817877985664088));
#15726=CARTESIAN_POINT('Ctrl Pts',(31.8280621443435,-0.366747863090102,
0.946194878116315));
#15727=CARTESIAN_POINT('Ctrl Pts',(31.818786283051,-0.240163206787939,0.985835062226092));
#15728=CARTESIAN_POINT('Ctrl Pts',(31.8001078040911,0.0207603676706945,
1.01327765451514));
#15729=CARTESIAN_POINT('Ctrl Pts',(31.7909121905271,0.15195887892012,1.00235989692945));
#15730=CARTESIAN_POINT('Ctrl Pts',(31.7706842229678,0.425111210006055,0.925080808596332));
#15731=CARTESIAN_POINT('Ctrl Pts',(31.761279437479,0.540347644379315,0.854950472866657));
#15732=CARTESIAN_POINT('Ctrl Pts',(31.7445489336977,0.724235313103983,0.708453750739634));
#15733=CARTESIAN_POINT('Ctrl Pts',(31.7355913796315,0.808338952205113,0.611915865043628));
#15734=CARTESIAN_POINT('Ctrl Pts',(31.7176616890085,0.934104160209125,0.394084134956314));
#15735=CARTESIAN_POINT('Ctrl Pts',(31.7087041349354,0.975656602098998,0.272979304096005));
#15736=CARTESIAN_POINT('Ctrl Pts',(31.691973631154,1.01058265066987,0.0404795504744009));
#15737=CARTESIAN_POINT('Ctrl Pts',(31.6825688456652,1.01369908580113,-0.0943832969990357));
#15738=CARTESIAN_POINT('Ctrl Pts',(31.6623408781059,0.944048573936179,-0.369579698988473));
#15739=CARTESIAN_POINT('Ctrl Pts',(31.6531452645421,0.887904373733188,-0.488659821461777));
#15740=CARTESIAN_POINT('Ctrl Pts',(31.6344667855823,0.733676604436161,-0.700904969244626));
#15741=CARTESIAN_POINT('Ctrl Pts',(31.6251909242898,0.63605486983531,-0.790710405276932));
#15742=CARTESIAN_POINT('Ctrl Pts',(31.6062871395422,0.408717770745883,-0.927836026440967));
#15743=CARTESIAN_POINT('Ctrl Pts',(31.5968914614619,0.282263576240687,-0.974048387998723));
#15744=CARTESIAN_POINT('Ctrl Pts',(31.5767599679311,0.00307419136583881,
-1.01744177706707));
#15745=CARTESIAN_POINT('Ctrl Pts',(31.5675657579804,-0.127880192190321,
-1.00327016540539));
#15746=CARTESIAN_POINT('Ctrl Pts',(31.5503412130368,-0.363230754564002,
-0.946762314668816));
#15747=CARTESIAN_POINT('Ctrl Pts',(31.5408377970794,-0.487117299376366,
-0.890303235238142));
#15748=CARTESIAN_POINT('Ctrl Pts',(31.5223393621535,-0.696376860255655,
-0.736824922057749));
#15749=CARTESIAN_POINT('Ctrl Pts',(31.5133691747455,-0.783304765554694,
-0.642559988636202));
#15750=CARTESIAN_POINT('Ctrl Pts',(31.4966022967237,-0.909104926108206,
-0.443337235931506));
#15751=CARTESIAN_POINT('Ctrl Pts',(31.4872100694454,-0.966019492682179,
-0.321250069431272));
#15752=CARTESIAN_POINT('Ctrl Pts',(31.4669931043532,-1.01296598826022,-0.0414324395852803));
#15753=CARTESIAN_POINT('Ctrl Pts',(31.4577862254883,-1.00948095071539,0.0903434934989293));
#15754=CARTESIAN_POINT('Ctrl Pts',(31.4390951849256,-0.953566173341268,
0.346849748046573));
#15755=CARTESIAN_POINT('Ctrl Pts',(31.429830716038,-0.900301395996993,0.46815105805527));
#15756=CARTESIAN_POINT('Ctrl Pts',(31.4109313504202,-0.747374114001067,
0.685109299359023));
#15757=CARTESIAN_POINT('Ctrl Pts',(31.4015280972467,-0.650119117375387,
0.778369367719778));
#15758=CARTESIAN_POINT('Ctrl Pts',(31.3813883967126,-0.411828409927458,
0.930377288092368));
#15759=CARTESIAN_POINT('Ctrl Pts',(31.3721978227729,-0.286247499755309,
0.969965709350148));
#15760=CARTESIAN_POINT('Ctrl Pts',(31.3550137492538,-0.0486169665865881,
1.01287742140833));
#15761=CARTESIAN_POINT('Ctrl Pts',(31.3455083028614,0.0875413822861097,
1.01111645447045));
#15762=CARTESIAN_POINT('Ctrl Pts',(31.3269831175199,0.341225419004652,0.95468072556934));
#15763=CARTESIAN_POINT('Ctrl Pts',(31.3179990632433,0.458920417080284,0.903256265996064));
#15764=CARTESIAN_POINT('Ctrl Pts',(31.3011932633659,0.654636111382735,0.771092380231486));
#15765=CARTESIAN_POINT('Ctrl Pts',(31.2918145524653,0.755567145070677,0.682208090561066));
#15766=CARTESIAN_POINT('Ctrl Pts',(31.2716085346413,0.91094139963879,0.444975024007283));
#15767=CARTESIAN_POINT('Ctrl Pts',(31.2623893808811,0.960786276316755,0.322740178671269));
#15768=CARTESIAN_POINT('Ctrl Pts',(31.2436857723214,1.0126128086746,0.0652074783839398));
#15769=CARTESIAN_POINT('Ctrl Pts',(31.2344324493892,1.01247717924913,-0.0671105513276969));
#15770=CARTESIAN_POINT('Ctrl Pts',(31.2155393998991,0.959648553525894,-0.327158651203486));
#15771=CARTESIAN_POINT('Ctrl Pts',(31.2061280661664,0.908027886468966,-0.451749616134968));
#15772=CARTESIAN_POINT('Ctrl Pts',(31.1859789261745,0.750738679733246,-0.686734029267041));
#15773=CARTESIAN_POINT('Ctrl Pts',(31.1767922836507,0.651606739985219,-0.77332403732232));
#15774=CARTESIAN_POINT('Ctrl Pts',(31.1602052306222,0.458249759673342,-0.903490004899917));
#15775=CARTESIAN_POINT('Ctrl Pts',(31.1507010317304,0.334083202713468,-0.959511029806068));
#15776=CARTESIAN_POINT('Ctrl Pts',(31.1315930535769,0.0710782558689687,
-1.0113329187058));
#15777=CARTESIAN_POINT('Ctrl Pts',(31.1225940990287,-0.057586472731709,
-1.01153056273425));
#15778=CARTESIAN_POINT('Ctrl Pts',(31.1057483213329,-0.290445664438458,
-0.968960876829247));
#15779=CARTESIAN_POINT('Ctrl Pts',(31.0963828878297,-0.418327990956272,
-0.928000835580201));
#15780=CARTESIAN_POINT('Ctrl Pts',(31.0761848842486,-0.655791268906789,
-0.773156797467833));
#15781=CARTESIAN_POINT('Ctrl Pts',(31.0669520428219,-0.750666938273188,
-0.681074536322006));
#15782=CARTESIAN_POINT('Ctrl Pts',(31.0482411755532,-0.90146749781528,-0.465863888580594));
#15783=CARTESIAN_POINT('Ctrl Pts',(31.0389957694103,-0.954288507126772,
-0.344674989241539));
#15784=CARTESIAN_POINT('Ctrl Pts',(31.0207107777182,-1.0084895405317,-0.0936168937762394));
#15785=CARTESIAN_POINT('Ctrl Pts',(31.0118846856426,-1.01254518840658,0.0325064994311476));
#15786=CARTESIAN_POINT('Ctrl Pts',(30.9929071645996,-0.972239729359772,
0.295767848335958));
#15787=CARTESIAN_POINT('Ctrl Pts',(30.9841478114738,-0.923830150460078,
0.411176385780254));
#15788=CARTESIAN_POINT('Ctrl Pts',(30.9766135577662,-0.870773359785341,
0.502739744071684));
#15789=CARTESIAN_POINT('',(31.1173426729392,-1.08229570837348,0.624863720382711));
#15790=CARTESIAN_POINT('',(31.1175,-1.082531754731,0.625));
#15791=CARTESIAN_POINT('Ctrl Pts',(31.1176143539202,-1.0821587115325,0.624802327952216));
#15792=CARTESIAN_POINT('Ctrl Pts',(31.1240060784292,-1.13782712827631,0.52886389959531));
#15793=CARTESIAN_POINT('Ctrl Pts',(31.1300982973054,-1.18011004660292,0.426676775976404));
#15794=CARTESIAN_POINT('Ctrl Pts',(31.1424052132346,-1.23534331762511,0.21651293345668));
#15795=CARTESIAN_POINT('Ctrl Pts',(31.1486181844907,-1.2490007937033,0.109811579967974));
#15796=CARTESIAN_POINT('Ctrl Pts',(31.1603920217383,-1.24950055350359,-0.0923920289202056));
#15797=CARTESIAN_POINT('Ctrl Pts',(31.1659562556459,-1.23898620331907,-0.188034416053155));
#15798=CARTESIAN_POINT('Ctrl Pts',(31.1772172324692,-1.19486152256834,-0.380931227675896));
#15799=CARTESIAN_POINT('Ctrl Pts',(31.1828002272484,-1.15990323431092,-0.476842290221254));
#15800=CARTESIAN_POINT('Ctrl Pts',(31.1933799224953,-1.07536359567061,-0.641674010671896));
#15801=CARTESIAN_POINT('Ctrl Pts',(31.1982004972963,-1.03015647433166,-0.711636089145887));
#15802=CARTESIAN_POINT('Ctrl Pts',(31.2086891642593,-0.918145662538923,
-0.852744715825088));
#15803=CARTESIAN_POINT('Ctrl Pts',(31.2143622631548,-0.848874078215494,
-0.922071107489431));
#15804=CARTESIAN_POINT('Ctrl Pts',(31.2258599403578,-0.690519777314687,
-1.04711607636139));
#15805=CARTESIAN_POINT('Ctrl Pts',(31.2315605712696,-0.601200097977752,
-1.10079838963472));
#15806=CARTESIAN_POINT('Ctrl Pts',(31.2422685234014,-0.429696982034391,
-1.17621321895925));
#15807=CARTESIAN_POINT('Ctrl Pts',(31.2470893694738,-0.350510236428935,
-1.20198149126957));
#15808=CARTESIAN_POINT('Ctrl Pts',(31.257554879535,-0.174979519772436,-1.24075076547737));
#15809=CARTESIAN_POINT('Ctrl Pts',(31.2632039529516,-0.0778867945370573,
-1.25086298378607));
#15810=CARTESIAN_POINT('Ctrl Pts',(31.2746485393151,0.123010454844053,-1.24821216732933));
#15811=CARTESIAN_POINT('Ctrl Pts',(31.280322861262,0.225730991441402,-1.23375161025498));
#15812=CARTESIAN_POINT('Ctrl Pts',(31.2910025371402,0.406028058762192,-1.18459423747141));
#15813=CARTESIAN_POINT('Ctrl Pts',(31.2958233857599,0.483792934919275,-1.15480128143035));
#15814=CARTESIAN_POINT('Ctrl Pts',(31.306290559336,0.644644376904782,-1.07448615399174));
#15815=CARTESIAN_POINT('Ctrl Pts',(31.3119413766805,0.726493363522555,-1.02124287488531));
#15816=CARTESIAN_POINT('Ctrl Pts',(31.3233905059103,0.88102312030248,-0.892733274001985));
#15817=CARTESIAN_POINT('Ctrl Pts',(31.3290672187261,0.951788897338445,-0.816826100609883));
#15818=CARTESIAN_POINT('Ctrl Pts',(31.3397493385164,1.06100281479554,-0.665128305607395));
#15819=CARTESIAN_POINT('Ctrl Pts',(31.3445701692346,1.10269161128873,-0.593037192331211));
#15820=CARTESIAN_POINT('Ctrl Pts',(31.3550382895877,1.17716691157256,-0.429381154761996));
#15821=CARTESIAN_POINT('Ctrl Pts',(31.3606900786588,1.20727587186345,-0.336478776281032));
#15822=CARTESIAN_POINT('Ctrl Pts',(31.3721410948635,1.24650146600664,-0.139327470567408));
#15823=CARTESIAN_POINT('Ctrl Pts',(31.3778186949677,1.25372629203966,-0.035786170497328));
#15824=CARTESIAN_POINT('Ctrl Pts',(31.3885018209641,1.24312755487409,0.150850910489866));
#15825=CARTESIAN_POINT('Ctrl Pts',(31.3933226590061,1.23015474858233,0.233110994982595));
#15826=CARTESIAN_POINT('Ctrl Pts',(31.4037902649713,1.18503744542128,0.407154197277295));
#15827=CARTESIAN_POINT('Ctrl Pts',(31.4094415234133,1.14997227807196,0.498292066471131));
#15828=CARTESIAN_POINT('Ctrl Pts',(31.4208914267738,1.05639139383983,0.676175349247458));
#15829=CARTESIAN_POINT('Ctrl Pts',(31.4265684855878,0.996851073617742,0.761180763904621));
#15830=CARTESIAN_POINT('Ctrl Pts',(31.4372510169724,0.871167832851708,0.899549283902962));
#15831=CARTESIAN_POINT('Ctrl Pts',(31.4420718532523,0.809318617397264,0.955314077686334));
#15832=CARTESIAN_POINT('Ctrl Pts',(31.4525396054238,0.664726021980267,1.0621808370084));
#15833=CARTESIAN_POINT('Ctrl Pts',(31.4581910150401,0.580118583972387,1.11094290951632));
#15834=CARTESIAN_POINT('Ctrl Pts',(31.4696412461842,0.395442457324174,1.19029483163864));
#15835=CARTESIAN_POINT('Ctrl Pts',(31.4753184665817,0.295672522154359,1.21888744119676));
#15836=CARTESIAN_POINT('Ctrl Pts',(31.4860011732024,0.110917242357187,1.24732498968612));
#15837=CARTESIAN_POINT('Ctrl Pts',(31.4908220096922,0.0277574696957337,
1.25173922866526));
#15838=CARTESIAN_POINT('Ctrl Pts',(31.5012897379625,-0.15186508887469,1.24379488711698));
#15839=CARTESIAN_POINT('Ctrl Pts',(31.5069411227735,-0.248303974134931,
1.22844486123761));
#15840=CARTESIAN_POINT('Ctrl Pts',(31.5183912843764,-0.441760912948824,
1.17389252414083));
#15841=CARTESIAN_POINT('Ctrl Pts',(31.5240684642586,-0.537289934727339,
1.13332616886551));
#15842=CARTESIAN_POINT('Ctrl Pts',(31.5347511268285,-0.698767508389034,
1.0391565055413));
#15843=CARTESIAN_POINT('Ctrl Pts',(31.5395719634338,-0.766172796318229,
0.990252910469221));
#15844=CARTESIAN_POINT('Ctrl Pts',(31.5500396974053,-0.900766349841046,
0.871038877426934));
#15845=CARTESIAN_POINT('Ctrl Pts',(31.5556910879605,-0.966053452853213,
0.7984186752522));
#15846=CARTESIAN_POINT('Ctrl Pts',(31.5671400108157,-1.08205433820025,0.634294972400312));
#15847=CARTESIAN_POINT('Ctrl Pts',(31.5728160323226,-1.13075742314166,0.542671102597745));
#15848=CARTESIAN_POINT('Ctrl Pts',(31.5834973753672,-1.1969878201771,0.367889849781088));
#15849=CARTESIAN_POINT('Ctrl Pts',(31.5883182192493,-1.2185997646116,0.287465667522941));
#15850=CARTESIAN_POINT('Ctrl Pts',(31.598786552775,-1.24818537041361,0.110107752503061));
#15851=CARTESIAN_POINT('Ctrl Pts',(31.6044385452042,-1.25322589302514,0.0125749161587526));
#15852=CARTESIAN_POINT('Ctrl Pts',(31.6159555432532,-1.24001667228593,-0.189166648342859));
#15853=CARTESIAN_POINT('Ctrl Pts',(31.6216943443875,-1.21983388555358,-0.292146062416069));
#15854=CARTESIAN_POINT('Ctrl Pts',(31.6324470241272,-1.16044909634215,-0.470588581982704));
#15855=CARTESIAN_POINT('Ctrl Pts',(31.6372674296349,-1.12643871032578,-0.546572117435137));
#15856=CARTESIAN_POINT('Ctrl Pts',(31.6468960985306,-1.04454265279206,-0.690254795732879));
#15857=CARTESIAN_POINT('Ctrl Pts',(31.6517073727424,-0.996655408805599,
-0.758051863175031));
#15858=CARTESIAN_POINT('Ctrl Pts',(31.6627702280804,-0.870203186990777,
-0.903984876539052));
#15859=CARTESIAN_POINT('Ctrl Pts',(31.6687898996599,-0.787576654254936,
-0.976889895296161));
#15860=CARTESIAN_POINT('Ctrl Pts',(31.6807821982022,-0.612473709547305,
-1.09370200728453));
#15861=CARTESIAN_POINT('Ctrl Pts',(31.6866153652929,-0.522536100534752,
-1.13912678752826));
#15862=CARTESIAN_POINT('Ctrl Pts',(31.6972573121406,-0.350845141361402,
-1.20189911231689));
#15863=CARTESIAN_POINT('Ctrl Pts',(31.7020725410413,-0.270255071154068,
-1.22276105030124));
#15864=CARTESIAN_POINT('Ctrl Pts',(31.7124537496761,-0.0904768146807791,
-1.25056862608197));
#15865=CARTESIAN_POINT('Ctrl Pts',(31.7178677208251,0.00831050603654517,
-1.25382693514982));
#15866=CARTESIAN_POINT('Ctrl Pts',(31.729120122559,0.205231055039715,-1.23651351800787));
#15867=CARTESIAN_POINT('Ctrl Pts',(31.7348690777854,0.302474923897132,-1.21611008967196));
#15868=CARTESIAN_POINT('Ctrl Pts',(31.7454278233989,0.474492182767166,-1.1586462038913));
#15869=CARTESIAN_POINT('Ctrl Pts',(31.750242280751,0.550446956570973,-1.12477176898818));
#15870=CARTESIAN_POINT('Ctrl Pts',(31.7608499067484,0.711610456908466,-1.03269615084912));
#15871=CARTESIAN_POINT('Ctrl Pts',(31.7664634133186,0.793642254012398,-0.971112508038292));
#15872=CARTESIAN_POINT('Ctrl Pts',(31.7779463101776,0.938547998489703,-0.83081467824553));
#15873=CARTESIAN_POINT('Ctrl Pts',(31.7837105565754,1.00135228378256,-0.753492673524034));
#15874=CARTESIAN_POINT('Ctrl Pts',(31.7942844843864,1.09879427128859,-0.600219979330559));
#15875=CARTESIAN_POINT('Ctrl Pts',(31.7990991412107,1.13640400067532,-0.526026457330732));
#15876=CARTESIAN_POINT('Ctrl Pts',(31.8096636675788,1.2031922306065,-0.353603390264143));
#15877=CARTESIAN_POINT('Ctrl Pts',(31.8152390244176,1.22794792049913,-0.254795958429211));
#15878=CARTESIAN_POINT('Ctrl Pts',(31.8266767980405,1.25221837372775,-0.0553556296855275));
#15879=CARTESIAN_POINT('Ctrl Pts',(31.8324371127675,1.25239511254884,0.0441936568360541));
#15880=CARTESIAN_POINT('Ctrl Pts',(31.8430071391335,1.23173787374873,0.224571567295447));
#15881=CARTESIAN_POINT('Ctrl Pts',(31.8478217466123,1.21430563356015,0.305901969734969));
#15882=CARTESIAN_POINT('Ctrl Pts',(31.8583971447548,1.15771387015253,0.482122034532278));
#15883=CARTESIAN_POINT('Ctrl Pts',(31.8639821116929,1.11471121147059,0.574659728153018));
#15884=CARTESIAN_POINT('Ctrl Pts',(31.8754311002046,1.00794890665499,0.745088064977724));
#15885=CARTESIAN_POINT('Ctrl Pts',(31.8811922595378,0.945424033184498,0.822570520864649));
#15886=CARTESIAN_POINT('Ctrl Pts',(31.8917631287764,0.815834206434843,0.949750247331783));
#15887=CARTESIAN_POINT('Ctrl Pts',(31.8965777506294,0.751099014735883,1.00198063352227));
#15888=CARTESIAN_POINT('Ctrl Pts',(31.9071510987955,0.596239547185957,1.10328359862058));
#15889=CARTESIAN_POINT('Ctrl Pts',(31.9127342708902,0.504612837395904,1.14811746123603));
#15890=CARTESIAN_POINT('Ctrl Pts',(31.9241816068141,0.31441684083408,1.21336736868684));
#15891=CARTESIAN_POINT('Ctrl Pts',(31.9299430459614,0.217059917363251,1.23423457381753));
#15892=CARTESIAN_POINT('Ctrl Pts',(31.940514178841,0.0363079555188546,1.25151630287605));
#15893=CARTESIAN_POINT('Ctrl Pts',(31.9453287907012,-0.0468705932600383,
1.25136661001164));
#15894=CARTESIAN_POINT('Ctrl Pts',(31.9559012836347,-0.230957182723031,
1.23263628126962));
#15895=CARTESIAN_POINT('Ctrl Pts',(31.9614836845859,-0.330365926848818,
1.20981945349652));
#15896=CARTESIAN_POINT('Ctrl Pts',(31.9729289302278,-0.519206939191319,
1.14084976837166));
#15897=CARTESIAN_POINT('Ctrl Pts',(31.9786890867423,-0.607981980552158,
1.09581189621577));
#15898=CARTESIAN_POINT('Ctrl Pts',(31.989258961414,-0.759316621509383,0.995514496023265));
#15899=CARTESIAN_POINT('Ctrl Pts',(31.9940735831732,-0.823867341779562,
0.943057378399203));
#15900=CARTESIAN_POINT('Ctrl Pts',(32.0046456557463,-0.955144999347304,
0.812668022846102));
#15901=CARTESIAN_POINT('Ctrl Pts',(32.0102275063711,-1.01804215831405,0.732388520580651));
#15902=CARTESIAN_POINT('Ctrl Pts',(32.0216724868892,-1.12141355965134,0.559953017256065));
#15903=CARTESIAN_POINT('Ctrl Pts',(32.0274331903612,-1.16207374523845,0.469074231388383));
#15904=CARTESIAN_POINT('Ctrl Pts',(32.0380037184577,-1.21657777222981,0.295881156004739));
#15905=CARTESIAN_POINT('Ctrl Pts',(32.0428183840667,-1.23373564079806,0.214493035986958));
#15906=CARTESIAN_POINT('Ctrl Pts',(32.053413281656,-1.25375520199998,0.0301660896758291));
#15907=CARTESIAN_POINT('Ctrl Pts',(32.0590165684404,-1.25206833167091,-0.0721904279698692));
#15908=CARTESIAN_POINT('Ctrl Pts',(32.0705013141532,-1.22362856901582,-0.271848294976713));
#15909=CARTESIAN_POINT('Ctrl Pts',(32.0762777295109,-1.19786641608811,-0.368269230476531));
#15910=CARTESIAN_POINT('Ctrl Pts',(32.086862971512,-1.13089974332563,-0.537309623191031));
#15911=CARTESIAN_POINT('Ctrl Pts',(32.0916772316598,-1.09290030489865,-0.611319008202032));
#15912=CARTESIAN_POINT('Ctrl Pts',(32.1021452017923,-0.993359558816285,
-0.76525346609263));
#15913=CARTESIAN_POINT('Ctrl Pts',(32.1076315891951,-0.92906785585012,-0.842177783760152));
#15914=CARTESIAN_POINT('Ctrl Pts',(32.118894750487,-0.7844446704897,-0.977499920442658));
#15915=CARTESIAN_POINT('Ctrl Pts',(32.1245780698579,-0.705266920519248,
-1.03574779176174));
#15916=CARTESIAN_POINT('Ctrl Pts',(32.136451253582,-0.528303136599548,-1.13705498101773));
#15917=CARTESIAN_POINT('Ctrl Pts',(32.1426442566818,-0.429344998410457,
-1.17836741706458));
#15918=CARTESIAN_POINT('Ctrl Pts',(32.1549206773639,-0.22019628775875,-1.23538794982945));
#15919=CARTESIAN_POINT('Ctrl Pts',(32.1610033640657,-0.110740339667427,
-1.24981720394665));
#15920=CARTESIAN_POINT('Ctrl Pts',(32.1673846094894,-2.65599045317292E-6,
-1.24957813805368));
#15921=CARTESIAN_POINT('Ctrl Pts',(32.36036289716,0.393685760654,-0.8842326957913));
#15922=CARTESIAN_POINT('Ctrl Pts',(32.34411289716,0.1930597260145,-0.9735571614325));
#15923=CARTESIAN_POINT('Ctrl Pts',(32.31161289716,-0.27049973535,-1.009904411168));
#15924=CARTESIAN_POINT('Ctrl Pts',(32.26286289716,-0.845926716811,-0.6145928909716));
#15925=CARTESIAN_POINT('Ctrl Pts',(32.21411289716,-1.044142703787,0.05472539254397));
#15926=CARTESIAN_POINT('Ctrl Pts',(32.16536289716,-0.7770226444626,0.6996312941492));
#15927=CARTESIAN_POINT('Ctrl Pts',(32.11661289716,-0.1635647789704,1.032711459003));
#15928=CARTESIAN_POINT('Ctrl Pts',(32.06786289716,0.5227918702356,0.905502289579));
#15929=CARTESIAN_POINT('Ctrl Pts',(32.01911289716,0.9761368603912,0.3747038366413));
#15930=CARTESIAN_POINT('Ctrl Pts',(31.97036289716,0.994409526335,-0.323103250189));
#15931=CARTESIAN_POINT('Ctrl Pts',(31.92161289716,0.5694658990877,-0.8769005799032));
#15932=CARTESIAN_POINT('Ctrl Pts',(31.87286289716,-0.109293296325,-1.039856246063));
#15933=CARTESIAN_POINT('Ctrl Pts',(31.82411289716,-0.7393395821542,-0.7393395822784));
#15934=CARTESIAN_POINT('Ctrl Pts',(31.77536289716,-1.039856245751,-0.1092932955163));
#15935=CARTESIAN_POINT('Ctrl Pts',(31.72661289716,-0.8769005812753,0.5694658959771));
#15936=CARTESIAN_POINT('Ctrl Pts',(31.67786289716,-0.3231032450128,0.9944095379687));
#15937=CARTESIAN_POINT('Ctrl Pts',(31.62911289716,0.3747038173086,0.9761368169669));
#15938=CARTESIAN_POINT('Ctrl Pts',(31.58036289716,0.9055023617337,0.5227920322988));
#15939=CARTESIAN_POINT('Ctrl Pts',(31.53161289716,1.032711189717,-0.1635653837993));
#15940=CARTESIAN_POINT('Ctrl Pts',(31.48286289716,0.69963229914,-0.7770203872106));
#15941=CARTESIAN_POINT('Ctrl Pts',(31.43411289716,0.05472164186737,-1.044151127966));
#15942=CARTESIAN_POINT('Ctrl Pts',(31.38536289716,-0.614578893256,-0.8458952773463));
#15943=CARTESIAN_POINT('Ctrl Pts',(31.33661289716,-1.009956651354,-0.2706170690297));
#15944=CARTESIAN_POINT('Ctrl Pts',(31.28786289716,-0.9551885735371,0.4252773519508));
#15945=CARTESIAN_POINT('Ctrl Pts',(31.23911289716,-0.4746852292457,0.9316222251505));
#15946=CARTESIAN_POINT('Ctrl Pts',(31.19036289716,0.2173891404585,1.022735536666));
#15947=CARTESIAN_POINT('Ctrl Pts',(31.14161289716,0.8125714716225,0.6580074003485));
#15948=CARTESIAN_POINT('Ctrl Pts',(31.09286289716,1.045583921078,-1.042735165158E-7));
#15949=CARTESIAN_POINT('Ctrl Pts',(31.04411289716,0.8125719687909,-0.6580069832544));
#15950=CARTESIAN_POINT('Ctrl Pts',(30.99536289716,0.2173871517845,-1.022736996495));
#15951=CARTESIAN_POINT('Ctrl Pts',(30.94661289716,-0.4746777717184,-0.9316168029278));
#15952=CARTESIAN_POINT('Ctrl Pts',(30.89786289716,-0.9552164149722,-0.4252975810124));
#15953=CARTESIAN_POINT('Ctrl Pts',(30.84911289716,-1.00985274314,0.2706925630538));
#15954=CARTESIAN_POINT('Ctrl Pts',(30.81661289716,-0.7465953708295,0.6539732078925));
#15955=CARTESIAN_POINT('Ctrl Pts',(30.80036289716,-0.568925097085,0.7830582177302));
#15956=CARTESIAN_POINT('Ctrl Pts',(32.29874545428,0.4370945424777,-0.9817304160777));
#15957=CARTESIAN_POINT('Ctrl Pts',(32.28249545428,0.2143469768198,-1.080904021891));
#15958=CARTESIAN_POINT('Ctrl Pts',(32.24999545428,-0.300325716294,-1.121259010771));
#15959=CARTESIAN_POINT('Ctrl Pts',(32.20124545428,-0.9392007235413,-0.6823594484165));
#15960=CARTESIAN_POINT('Ctrl Pts',(32.15249545428,-1.159272503621,0.06075955192329));
#15961=CARTESIAN_POINT('Ctrl Pts',(32.10374545428,-0.8626991149286,0.7767743997427));
#15962=CARTESIAN_POINT('Ctrl Pts',(32.05499545428,-0.1815998427547,1.146580821045));
#15963=CARTESIAN_POINT('Ctrl Pts',(32.00624545428,0.5804362163164,1.005345248755));
#15964=CARTESIAN_POINT('Ctrl Pts',(31.95749545428,1.083768164943,0.4160196237966));
#15965=CARTESIAN_POINT('Ctrl Pts',(31.90874545428,1.104055620977,-0.3587294269415));
#15966=CARTESIAN_POINT('Ctrl Pts',(31.85999545428,0.6322566409435,-0.9735898426565));
#15967=CARTESIAN_POINT('Ctrl Pts',(31.81124545428,-0.1213442499767,-1.154513410291));
#15968=CARTESIAN_POINT('Ctrl Pts',(31.76249545428,-0.8208610234226,-0.8208610235605));
#15969=CARTESIAN_POINT('Ctrl Pts',(31.71374545428,-1.154513409944,-0.1213442490788));
#15970=CARTESIAN_POINT('Ctrl Pts',(31.66499545428,-0.9735898441798,0.6322566374899));
#15971=CARTESIAN_POINT('Ctrl Pts',(31.61624545428,-0.3587294211945,1.104055633894));
#15972=CARTESIAN_POINT('Ctrl Pts',(31.56749545428,0.4160196023322,1.083768116731));
#15973=CARTESIAN_POINT('Ctrl Pts',(31.51874545428,1.005345328866,0.5804363962492));
#15974=CARTESIAN_POINT('Ctrl Pts',(31.46999545428,1.146580522067,-0.1816005142735));
#15975=CARTESIAN_POINT('Ctrl Pts',(31.42124545428,0.7767755155462,-0.8626966087863));
#15976=CARTESIAN_POINT('Ctrl Pts',(31.37249545428,0.06075538768766,-1.159281856671));
#15977=CARTESIAN_POINT('Ctrl Pts',(31.32374545428,-0.6823439072776,-0.9391658174822));
#15978=CARTESIAN_POINT('Ctrl Pts',(31.27499545428,-1.121317011091,-0.3004559874802));
#15979=CARTESIAN_POINT('Ctrl Pts',(31.22624545428,-1.06051006731,0.4721695020624));
#15980=CARTESIAN_POINT('Ctrl Pts',(31.17749545428,-0.5270252161353,1.034345234097));
#15981=CARTESIAN_POINT('Ctrl Pts',(31.12874545428,0.2413590136724,1.135504928428));
#15982=CARTESIAN_POINT('Ctrl Pts',(31.07999545428,0.9021676451524,0.7305609507554));
#15983=CARTESIAN_POINT('Ctrl Pts',(31.03124545428,1.160872633154,-1.157709766729E-7));
#15984=CARTESIAN_POINT('Ctrl Pts',(30.98249545428,0.9021681971399,-0.7305604876715));
#15985=CARTESIAN_POINT('Ctrl Pts',(30.93374545428,0.2413568057222,-1.135506549222));
#15986=CARTESIAN_POINT('Ctrl Pts',(30.88499545428,-0.5270169363223,-1.034339214006));
#15987=CARTESIAN_POINT('Ctrl Pts',(30.83624545428,-1.060540978612,-0.4721919616312));
#15988=CARTESIAN_POINT('Ctrl Pts',(30.78749545428,-1.121201645697,0.3005398056652));
#15989=CARTESIAN_POINT('Ctrl Pts',(30.75499545428,-0.8289168536006,0.7260819380959));
#15990=CARTESIAN_POINT('Ctrl Pts',(30.73874545428,-0.6316562087523,0.86940018568));
#15991=CARTESIAN_POINT('Ctrl Pts',(32.2371280114,0.4805033243013,-1.079228136364));
#15992=CARTESIAN_POINT('Ctrl Pts',(32.2208780114,0.2356342276251,-1.18825088235));
#15993=CARTESIAN_POINT('Ctrl Pts',(32.1883780114,-0.330151697238,-1.232613610374));
#15994=CARTESIAN_POINT('Ctrl Pts',(32.1396280114,-1.032474730272,-0.7501260058613));
#15995=CARTESIAN_POINT('Ctrl Pts',(32.0908780114,-1.274402303455,0.06679371130262));
#15996=CARTESIAN_POINT('Ctrl Pts',(32.0421280114,-0.9483755853946,0.8539175053361));
#15997=CARTESIAN_POINT('Ctrl Pts',(31.9933780114,-0.199634906539,1.260450183087));
#15998=CARTESIAN_POINT('Ctrl Pts',(31.9446280114,0.6380805623973,1.105188207931));
#15999=CARTESIAN_POINT('Ctrl Pts',(31.8958780114,1.191399469495,0.457335410952));
#16000=CARTESIAN_POINT('Ctrl Pts',(31.8471280114,1.21370171562,-0.3943556036939));
#16001=CARTESIAN_POINT('Ctrl Pts',(31.7983780114,0.6950473827993,-1.07027910541));
#16002=CARTESIAN_POINT('Ctrl Pts',(31.7496280114,-0.1333952036284,-1.269170574518));
#16003=CARTESIAN_POINT('Ctrl Pts',(31.7008780114,-0.902382464691,-0.9023824648425));
#16004=CARTESIAN_POINT('Ctrl Pts',(31.6521280114,-1.269170574137,-0.1333952026413));
#16005=CARTESIAN_POINT('Ctrl Pts',(31.6033780114,-1.070279107084,0.6950473790027));
#16006=CARTESIAN_POINT('Ctrl Pts',(31.5546280114,-0.3943555973762,1.213701729819));
#16007=CARTESIAN_POINT('Ctrl Pts',(31.5058780114,0.4573353873559,1.191399416495));
#16008=CARTESIAN_POINT('Ctrl Pts',(31.4571280114,1.105188295998,0.6380807601996));
#16009=CARTESIAN_POINT('Ctrl Pts',(31.4083780114,1.260449854417,-0.1996356447478));
#16010=CARTESIAN_POINT('Ctrl Pts',(31.3596280114,0.8539187319524,-0.948372830362));
#16011=CARTESIAN_POINT('Ctrl Pts',(31.3108780114,0.06678913350795,-1.274412585376));
#16012=CARTESIAN_POINT('Ctrl Pts',(31.2621280114,-0.7501089212991,-1.032436357618));
#16013=CARTESIAN_POINT('Ctrl Pts',(31.2133780114,-1.232677370829,-0.3302949059307));
#16014=CARTESIAN_POINT('Ctrl Pts',(31.1646280114,-1.165831561083,0.519061652174));
#16015=CARTESIAN_POINT('Ctrl Pts',(31.1158780114,-0.5793652030249,1.137068243043));
#16016=CARTESIAN_POINT('Ctrl Pts',(31.0671280114,0.2653288868863,1.248274320191));
#16017=CARTESIAN_POINT('Ctrl Pts',(31.0183780114,0.9917638186823,0.8031145011624));
#16018=CARTESIAN_POINT('Ctrl Pts',(30.9696280114,1.27616134523,-1.272684367085E-7));
#16019=CARTESIAN_POINT('Ctrl Pts',(30.9208780114,0.9917644254889,-0.8031139920886));
#16020=CARTESIAN_POINT('Ctrl Pts',(30.8721280114,0.26532645966,-1.248276101949));
#16021=CARTESIAN_POINT('Ctrl Pts',(30.8233780114,-0.5793561009262,-1.137061625084));
#16022=CARTESIAN_POINT('Ctrl Pts',(30.7746280114,-1.165865542251,-0.5190863422501));
#16023=CARTESIAN_POINT('Ctrl Pts',(30.7258780114,-1.232550548254,0.3303870482766));
#16024=CARTESIAN_POINT('Ctrl Pts',(30.6933780114,-0.9112383363718,0.7981906682994));
#16025=CARTESIAN_POINT('Ctrl Pts',(30.6771280114,-0.6943873204195,0.9557421536299));
#16026=CARTESIAN_POINT('Ctrl Pts',(32.17551056852,0.523912106125,-1.17672585665));
#16027=CARTESIAN_POINT('Ctrl Pts',(32.15926056852,0.2569214784303,-1.295597742809));
#16028=CARTESIAN_POINT('Ctrl Pts',(32.12676056852,-0.3599776781819,-1.343968209978));
#16029=CARTESIAN_POINT('Ctrl Pts',(32.07801056852,-1.125748737002,-0.8178925633062));
#16030=CARTESIAN_POINT('Ctrl Pts',(32.02926056852,-1.389532103288,0.07282787068194));
#16031=CARTESIAN_POINT('Ctrl Pts',(31.98051056852,-1.034052055861,0.9310606109295));
#16032=CARTESIAN_POINT('Ctrl Pts',(31.93176056852,-0.2176699703234,1.374319545129));
#16033=CARTESIAN_POINT('Ctrl Pts',(31.88301056852,0.6957249084782,1.205031167107));
#16034=CARTESIAN_POINT('Ctrl Pts',(31.83426056852,1.299030774048,0.4986511981073));
#16035=CARTESIAN_POINT('Ctrl Pts',(31.78551056852,1.323347810262,-0.4299817804464));
#16036=CARTESIAN_POINT('Ctrl Pts',(31.73676056852,0.7578381246551,-1.166968368163));
#16037=CARTESIAN_POINT('Ctrl Pts',(31.68801056852,-0.14544615728,-1.383827738746));
#16038=CARTESIAN_POINT('Ctrl Pts',(31.63926056852,-0.9839039059594,-0.9839039061246));
#16039=CARTESIAN_POINT('Ctrl Pts',(31.59051056852,-1.383827738331,-0.1454461562038));
#16040=CARTESIAN_POINT('Ctrl Pts',(31.54176056852,-1.166968369989,0.7578381205155));
#16041=CARTESIAN_POINT('Ctrl Pts',(31.49301056852,-0.4299817735579,1.323347825744));
#16042=CARTESIAN_POINT('Ctrl Pts',(31.44426056852,0.4986511723795,1.299030716259));
#16043=CARTESIAN_POINT('Ctrl Pts',(31.39551056852,1.20503126313,0.69572512415));
#16044=CARTESIAN_POINT('Ctrl Pts',(31.34676056852,1.374319186766,-0.217670775222));
#16045=CARTESIAN_POINT('Ctrl Pts',(31.29801056852,0.9310619483586,-1.034049051938));
#16046=CARTESIAN_POINT('Ctrl Pts',(31.24926056852,0.07282287932824,-1.389543314081));
#16047=CARTESIAN_POINT('Ctrl Pts',(31.20051056852,-0.8178739353206,-1.125706897754));
#16048=CARTESIAN_POINT('Ctrl Pts',(31.15176056852,-1.344037730566,-0.3601338243812));
#16049=CARTESIAN_POINT('Ctrl Pts',(31.10301056852,-1.271153054855,0.5659538022856));
#16050=CARTESIAN_POINT('Ctrl Pts',(31.05426056852,-0.6317051899145,1.239791251989));
#16051=CARTESIAN_POINT('Ctrl Pts',(31.00551056852,0.2892987601002,1.361043711953));
#16052=CARTESIAN_POINT('Ctrl Pts',(30.95676056852,1.081359992212,0.8756680515693));
#16053=CARTESIAN_POINT('Ctrl Pts',(30.90801056852,1.391450057306,-1.387658968566E-7));
#16054=CARTESIAN_POINT('Ctrl Pts',(30.85926056852,1.081360653838,-0.8756674965057));
#16055=CARTESIAN_POINT('Ctrl Pts',(30.81051056852,0.2892961135977,-1.361045654676));
#16056=CARTESIAN_POINT('Ctrl Pts',(30.76176056852,-0.6316952655301,-1.239784036163));
#16057=CARTESIAN_POINT('Ctrl Pts',(30.71301056852,-1.271190105891,-0.5659807228689));
#16058=CARTESIAN_POINT('Ctrl Pts',(30.66426056852,-1.34389945081,0.360234290888));
#16059=CARTESIAN_POINT('Ctrl Pts',(30.63176056852,-0.9935598191429,0.8702993985029));
#16060=CARTESIAN_POINT('Ctrl Pts',(30.61551056852,-0.7571184320868,1.04208412158));
#16061=CARTESIAN_POINT('',(30.6676573270714,-1.08229570995281,0.624863717659191));
#16062=CARTESIAN_POINT('Ctrl Pts',(31.1176273419681,-1.08213858864712,0.62479197410143));
#16063=CARTESIAN_POINT('Ctrl Pts',(31.1107147429913,-1.02303331417979,0.727024583856292));
#16064=CARTESIAN_POINT('Ctrl Pts',(31.1036652880828,-0.949354002246978,
0.821167118675191));
#16065=CARTESIAN_POINT('Ctrl Pts',(31.0914707967952,-0.793986411015714,
0.96976959435426));
#16066=CARTESIAN_POINT('Ctrl Pts',(31.0861831561242,-0.716601260523713,
1.02825175920507));
#16067=CARTESIAN_POINT('Ctrl Pts',(31.074597198985,-0.539033774835006,1.1326861784073));
#16068=CARTESIAN_POINT('Ctrl Pts',(31.0681881308309,-0.437716166441462,
1.17534812713065));
#16069=CARTESIAN_POINT('Ctrl Pts',(31.0562672659825,-0.24255605393822,1.22931251285163));
#16070=CARTESIAN_POINT('Ctrl Pts',(31.0508051636701,-0.149571656505103,
1.24420676722394));
#16071=CARTESIAN_POINT('Ctrl Pts',(31.0418623888304,0.00919625518616045,
1.2512800440883));
#16072=CARTESIAN_POINT('Ctrl Pts',(31.0382746672938,0.0741691752309933,
1.24910986516245));
#16073=CARTESIAN_POINT('Ctrl Pts',(31.0251896685361,0.306806851999765,1.22316153355839));
#16074=CARTESIAN_POINT('Ctrl Pts',(31.016360185823,0.449029898248617,1.17281102777512));
#16075=CARTESIAN_POINT('Ctrl Pts',(30.99912749308,0.711896397089818,1.04065123262023));
#16076=CARTESIAN_POINT('Ctrl Pts',(30.9909450788194,0.82899352376291,0.944182238937826));
#16077=CARTESIAN_POINT('Ctrl Pts',(30.9774634344618,0.991793696766178,0.767975237832159));
#16078=CARTESIAN_POINT('Ctrl Pts',(30.9711100347715,1.05467900915692,0.678676212367285));
#16079=CARTESIAN_POINT('Ctrl Pts',(30.959202210651,1.14908717222668,0.499730244100428));
#16080=CARTESIAN_POINT('Ctrl Pts',(30.9537007807284,1.18369135429807,0.411566765861706));
#16081=CARTESIAN_POINT('Ctrl Pts',(30.9438229027414,1.22863151928554,0.242012696805622));
#16082=CARTESIAN_POINT('Ctrl Pts',(30.9393693749073,1.24172722685384,0.161905228300936));
#16083=CARTESIAN_POINT('Ctrl Pts',(30.928625116135,1.25416164465956,-0.028878966128762));
#16084=CARTESIAN_POINT('Ctrl Pts',(30.9221845557975,1.24653514576959,-0.139280723297152));
#16085=CARTESIAN_POINT('Ctrl Pts',(30.9104528390688,1.20718822105003,-0.33471427577669));
#16086=CARTESIAN_POINT('Ctrl Pts',(30.9052034580452,1.180076443489,-0.42084528229441));
#16087=CARTESIAN_POINT('Ctrl Pts',(30.897142254913,1.12250736390062,-0.551664921075211));
#16088=CARTESIAN_POINT('Ctrl Pts',(30.8942079540235,1.09821626001909,-0.598579294719281));
#16089=CARTESIAN_POINT('Ctrl Pts',(30.8870456269382,1.0319671908342,-0.708770188829124));
#16090=CARTESIAN_POINT('Ctrl Pts',(30.8828141613499,0.987150554639301,-0.769988214526295));
#16091=CARTESIAN_POINT('Ctrl Pts',(30.8740840162147,0.887207752238275,-0.883080681038765));
#16092=CARTESIAN_POINT('Ctrl Pts',(30.8696447196692,0.832425385282746,-0.934834990540918));
#16093=CARTESIAN_POINT('Ctrl Pts',(30.8549499340359,0.636142316174003,-1.08965651088435));
#16094=CARTESIAN_POINT('Ctrl Pts',(30.8460582886474,0.488207161417728,-1.15990237222862));
#16095=CARTESIAN_POINT('Ctrl Pts',(30.8310695387291,0.231609455004719,-1.23364856654246));
#16096=CARTESIAN_POINT('Ctrl Pts',(30.8241653576879,0.114175065965537,-1.24976891671705));
#16097=CARTESIAN_POINT('Ctrl Pts',(30.8117487577039,-0.0969174534092562,
-1.24928985471921));
#16098=CARTESIAN_POINT('Ctrl Pts',(30.8063060980654,-0.190566114444294,
-1.23860282577024));
#16099=CARTESIAN_POINT('Ctrl Pts',(30.7964788123334,-0.361099480681787,
-1.1990421161748));
#16100=CARTESIAN_POINT('Ctrl Pts',(30.7920242842892,-0.438035516948806,
-1.17312939535201));
#16101=CARTESIAN_POINT('Ctrl Pts',(30.7821347361325,-0.598054952684592,
-1.10128766414562));
#16102=CARTESIAN_POINT('Ctrl Pts',(30.7766219444153,-0.679463409247483,
-1.05282931385649));
#16103=CARTESIAN_POINT('Ctrl Pts',(30.7645953465248,-0.842366488971656,
-0.929432657525112));
#16104=CARTESIAN_POINT('Ctrl Pts',(30.7581474996506,-0.921522622038355,
-0.851300688675754));
#16105=CARTESIAN_POINT('Ctrl Pts',(30.7473757956398,-1.03884531089792,-0.699249054330331));
#16106=CARTESIAN_POINT('Ctrl Pts',(30.7429074217849,-1.08209144506206,-0.630271416060541));
#16107=CARTESIAN_POINT('Ctrl Pts',(30.7330205452947,-1.16020648864805,-0.473609586532843));
#16108=CARTESIAN_POINT('Ctrl Pts',(30.7275265553958,-1.19235173606669,-0.385071099146812));
#16109=CARTESIAN_POINT('Ctrl Pts',(30.7159283777517,-1.23871500251242,-0.193658268460273));
#16110=CARTESIAN_POINT('Ctrl Pts',(30.7098661712449,-1.25070029183962,-0.0900484640374073));
#16111=CARTESIAN_POINT('Ctrl Pts',(30.6953712902796,-1.24780339486507,0.167826800855185));
#16112=CARTESIAN_POINT('Ctrl Pts',(30.6862525691742,-1.21748631584923,0.333552517175049));
#16113=CARTESIAN_POINT('Ctrl Pts',(30.6729396636004,-1.12715505203218,0.541344630190737));
#16114=CARTESIAN_POINT('Ctrl Pts',(30.6701455790125,-1.10581562102616,0.58372568895839));
#16115=CARTESIAN_POINT('Ctrl Pts',(30.6673726659358,-1.08215508341737,0.62476340416037));
#16116=CARTESIAN_POINT('',(30.8083734681527,-0.871221485874862,0.502999959144598));
#16117=CARTESIAN_POINT('',(30.80837346568,-0.8712215562071,0.503));
#16118=CARTESIAN_POINT('Ctrl Pts',(32.3083865340664,-1.74310513141563E-10,
-1.00548172051402));
#16119=CARTESIAN_POINT('Ctrl Pts',(32.3008522416291,-0.105825134387246,
-1.00564870423719));
#16120=CARTESIAN_POINT('Ctrl Pts',(32.292092822766,-0.229977637746814,-0.989868369579392));
#16121=CARTESIAN_POINT('Ctrl Pts',(32.2731152412578,-0.478122027735569,
-0.89314255386251));
#16122=CARTESIAN_POINT('Ctrl Pts',(32.2642891857646,-0.585319758593422,
-0.82656877022494));
#16123=CARTESIAN_POINT('Ctrl Pts',(32.2460042305897,-0.775641550295093,
-0.654100595091272));
#16124=CARTESIAN_POINT('Ctrl Pts',(32.2367588244469,-0.854183711123656,
-0.547761809504565));
#16125=CARTESIAN_POINT('Ctrl Pts',(32.2180479571783,-0.96516131946172,-0.309559370165468));
#16126=CARTESIAN_POINT('Ctrl Pts',(32.2088151157516,-0.997469062168773,
-0.18135349972004));
#16127=CARTESIAN_POINT('Ctrl Pts',(32.1886171121706,-1.01283629382345,0.101717750507548));
#16128=CARTESIAN_POINT('Ctrl Pts',(32.1792516786673,-0.984367566826269,
0.232947114591695));
#16129=CARTESIAN_POINT('Ctrl Pts',(32.1624059009715,-0.904804400397712,
0.455893933067162));
#16130=CARTESIAN_POINT('Ctrl Pts',(32.1534069464232,-0.8403008713478,0.567222034592228));
#16131=CARTESIAN_POINT('Ctrl Pts',(32.1342989682696,-0.663919325666452,
0.769080055430524));
#16132=CARTESIAN_POINT('Ctrl Pts',(32.1247947693777,-0.553320416471879,
0.848600935605247));
#16133=CARTESIAN_POINT('Ctrl Pts',(32.1082077163491,-0.343914891685575,
0.950970008765684));
#16134=CARTESIAN_POINT('Ctrl Pts',(32.0990210738252,-0.219359775122022,
0.993525782886267));
#16135=CARTESIAN_POINT('Ctrl Pts',(32.0788719338334,0.0627872995112449,
1.01225002509461));
#16136=CARTESIAN_POINT('Ctrl Pts',(32.0694606001008,0.196496573752336,0.99465935166052));
#16137=CARTESIAN_POINT('Ctrl Pts',(32.0505675506108,0.448119147312173,0.910386233646103));
#16138=CARTESIAN_POINT('Ctrl Pts',(32.0413142276786,0.562777737133885,0.844344677318304));
#16139=CARTESIAN_POINT('Ctrl Pts',(32.022610619119,0.75989433170913,0.670695233562689));
#16140=CARTESIAN_POINT('Ctrl Pts',(32.0133914653588,0.840830374658887,0.566410881442958));
#16141=CARTESIAN_POINT('Ctrl Pts',(31.9931854475348,0.968593109628251,0.313236296615739));
#16142=CARTESIAN_POINT('Ctrl Pts',(31.9838067366341,0.995103645636241,0.181385312576401));
#16143=CARTESIAN_POINT('Ctrl Pts',(31.9670009367567,1.01170308102003,-0.0541913934911888));
#16144=CARTESIAN_POINT('Ctrl Pts',(31.9580168824801,0.997390470348591,-0.181830481509643));
#16145=CARTESIAN_POINT('Ctrl Pts',(31.9394916971386,0.919423226898875,-0.429745166292926));
#16146=CARTESIAN_POINT('Ctrl Pts',(31.9299862507461,0.852869094566032,-0.548542238822891));
#16147=CARTESIAN_POINT('Ctrl Pts',(31.9128021772271,0.696891195219597,-0.732880461232638));
#16148=CARTESIAN_POINT('Ctrl Pts',(31.9036116032874,0.599816161628682,-0.82184250904315));
#16149=CARTESIAN_POINT('Ctrl Pts',(31.8834719027534,0.349028087285575,-0.952204354992635));
#16150=CARTESIAN_POINT('Ctrl Pts',(31.87406864958,0.219635000613414,-0.989799618535099));
#16151=CARTESIAN_POINT('Ctrl Pts',(31.8551692839622,-0.0447199889143614,
-1.01375940902338));
#16152=CARTESIAN_POINT('Ctrl Pts',(31.8459048150744,-0.176402393566575,
-0.999237404326071));
#16153=CARTESIAN_POINT('Ctrl Pts',(31.8272137745116,-0.426500714921257,
-0.919407894705326));
#16154=CARTESIAN_POINT('Ctrl Pts',(31.8180068956466,-0.54236453935169,-0.856538059210491));
#16155=CARTESIAN_POINT('Ctrl Pts',(31.7977899305543,-0.76122046743556,-0.675972386498982));
#16156=CARTESIAN_POINT('Ctrl Pts',(31.7883977032762,-0.83849377181371,-0.565639342750775));
#16157=CARTESIAN_POINT('Ctrl Pts',(31.7716308252545,-0.948125656391319,
-0.357081831558923));
#16158=CARTESIAN_POINT('Ctrl Pts',(31.7626606378466,-0.986297530771064,
-0.234667590561064));
#16159=CARTESIAN_POINT('Ctrl Pts',(31.7441622029207,-1.01458386847578,0.023295661735769));
#16160=CARTESIAN_POINT('Ctrl Pts',(31.7346587869633,-1.00153559313095,0.158814096445749));
#16161=CARTESIAN_POINT('Ctrl Pts',(31.7174342420197,-0.932797546195441,
0.390887587624608));
#16162=CARTESIAN_POINT('Ctrl Pts',(31.7082400320689,-0.879593330129108,
0.511383216351974));
#16163=CARTESIAN_POINT('Ctrl Pts',(31.6881085385382,-0.702418860402563,
0.731471621586348));
#16164=CARTESIAN_POINT('Ctrl Pts',(31.6787128604578,-0.599170684072249,
0.817877985664102));
#16165=CARTESIAN_POINT('Ctrl Pts',(31.6598090757102,-0.366747863090086,
0.94619487811632));
#16166=CARTESIAN_POINT('Ctrl Pts',(31.6505332144177,-0.240163206787929,
0.985835062226094));
#16167=CARTESIAN_POINT('Ctrl Pts',(31.631854735458,0.0207603676707009,1.01327765451514));
#16168=CARTESIAN_POINT('Ctrl Pts',(31.6226591218942,0.151958878920123,1.00235989692945));
#16169=CARTESIAN_POINT('Ctrl Pts',(31.6024311543349,0.425111210006055,0.925080808596332));
#16170=CARTESIAN_POINT('Ctrl Pts',(31.5930263688461,0.540347644379315,0.854950472866657));
#16171=CARTESIAN_POINT('Ctrl Pts',(31.5762958650647,0.724235313103979,0.708453750739638));
#16172=CARTESIAN_POINT('Ctrl Pts',(31.5673383109915,0.808338952205112,0.61191586504363));
#16173=CARTESIAN_POINT('Ctrl Pts',(31.5494086203685,0.934104160209125,0.394084134956314));
#16174=CARTESIAN_POINT('Ctrl Pts',(31.5404510663023,0.975656602098998,0.272979304096006));
#16175=CARTESIAN_POINT('Ctrl Pts',(31.5237205625209,1.01058265066987,0.0404795504743948));
#16176=CARTESIAN_POINT('Ctrl Pts',(31.5143157770322,1.01369908580113,-0.0943832969990423));
#16177=CARTESIAN_POINT('Ctrl Pts',(31.4940878094729,0.944048573936176,-0.36957969898848));
#16178=CARTESIAN_POINT('Ctrl Pts',(31.484892195909,0.887904373733185,-0.488659821461784));
#16179=CARTESIAN_POINT('Ctrl Pts',(31.4662137169492,0.733676604436153,-0.700904969244634));
#16180=CARTESIAN_POINT('Ctrl Pts',(31.4569378556567,0.636054869835301,-0.790710405276939));
#16181=CARTESIAN_POINT('Ctrl Pts',(31.438034070909,0.408717770745871,-0.927836026440972));
#16182=CARTESIAN_POINT('Ctrl Pts',(31.4286383928287,0.282263576240673,-0.974048387998727));
#16183=CARTESIAN_POINT('Ctrl Pts',(31.408506899298,0.0030741913658229,-1.01744177706707));
#16184=CARTESIAN_POINT('Ctrl Pts',(31.3993126893472,-0.127880192190337,
-1.00327016540538));
#16185=CARTESIAN_POINT('Ctrl Pts',(31.3820881444036,-0.363230754564014,
-0.946762314668811));
#16186=CARTESIAN_POINT('Ctrl Pts',(31.3725847284462,-0.487117299376376,
-0.890303235238137));
#16187=CARTESIAN_POINT('Ctrl Pts',(31.3540862935205,-0.696376860255659,
-0.736824922057744));
#16188=CARTESIAN_POINT('Ctrl Pts',(31.3451161061127,-0.783304765554694,
-0.642559988636201));
#16189=CARTESIAN_POINT('Ctrl Pts',(31.328349228091,-0.909104926108205,-0.443337235931508));
#16190=CARTESIAN_POINT('Ctrl Pts',(31.318957000813,-0.966019492682176,-0.321250069431278));
#16191=CARTESIAN_POINT('Ctrl Pts',(31.2987400357208,-1.01296598826022,-0.0414324395852903));
#16192=CARTESIAN_POINT('Ctrl Pts',(31.2895331568557,-1.00948095071539,0.0903434934989204));
#16193=CARTESIAN_POINT('Ctrl Pts',(31.2708421162928,-0.953566173341271,
0.346849748046566));
#16194=CARTESIAN_POINT('Ctrl Pts',(31.261577647405,-0.900301395996995,0.468151058055271));
#16195=CARTESIAN_POINT('Ctrl Pts',(31.2426782817871,-0.74737411400106,0.685109299359031));
#16196=CARTESIAN_POINT('Ctrl Pts',(31.2332750286137,-0.650119117375376,
0.778369367719788));
#16197=CARTESIAN_POINT('Ctrl Pts',(31.2131353280796,-0.411828409927442,
0.930377288092374));
#16198=CARTESIAN_POINT('Ctrl Pts',(31.20394475414,-0.286247499755294,0.969965709350153));
#16199=CARTESIAN_POINT('Ctrl Pts',(31.1867606806209,-0.048616966586575,
1.01287742140833));
#16200=CARTESIAN_POINT('Ctrl Pts',(31.1772552342285,0.0875413822861211,
1.01111645447045));
#16201=CARTESIAN_POINT('Ctrl Pts',(31.158730048887,0.341225419004663,0.954680725569337));
#16202=CARTESIAN_POINT('Ctrl Pts',(31.1497459946104,0.458920417080296,0.903256265996058));
#16203=CARTESIAN_POINT('Ctrl Pts',(31.132940194733,0.654636111382746,0.771092380231476));
#16204=CARTESIAN_POINT('Ctrl Pts',(31.1235614838323,0.755567145070688,0.682208090561055));
#16205=CARTESIAN_POINT('Ctrl Pts',(31.1033554660083,0.910941399638799,0.444975024007267));
#16206=CARTESIAN_POINT('Ctrl Pts',(31.094136312248,0.960786276316762,0.322740178671249));
#16207=CARTESIAN_POINT('Ctrl Pts',(31.0754327036884,1.0126128086746,0.0652074783839158));
#16208=CARTESIAN_POINT('Ctrl Pts',(31.0661793807561,1.01247717924913,-0.0671105513277207));
#16209=CARTESIAN_POINT('Ctrl Pts',(31.0472863312659,0.959648553525886,-0.327158651203511));
#16210=CARTESIAN_POINT('Ctrl Pts',(31.0378749975333,0.908027886468954,-0.451749616134993));
#16211=CARTESIAN_POINT('Ctrl Pts',(31.0177258575413,0.750738679733226,-0.686734029267063));
#16212=CARTESIAN_POINT('Ctrl Pts',(31.0085392150175,0.651606739985195,-0.773324037322341));
#16213=CARTESIAN_POINT('Ctrl Pts',(30.9919521619889,0.458249759673328,-0.903490004899922));
#16214=CARTESIAN_POINT('Ctrl Pts',(30.9824479630971,0.334083202713453,-0.959511029806077));
#16215=CARTESIAN_POINT('Ctrl Pts',(30.9633399849436,0.0710782558689305,
-1.0113329187058));
#16216=CARTESIAN_POINT('Ctrl Pts',(30.9543410303954,-0.0575864727317485,
-1.01153056273425));
#16217=CARTESIAN_POINT('Ctrl Pts',(30.9374952526997,-0.290445664438498,
-0.968960876829235));
#16218=CARTESIAN_POINT('Ctrl Pts',(30.9281298191965,-0.418327990956307,
-0.928000835580185));
#16219=CARTESIAN_POINT('Ctrl Pts',(30.9079318156155,-0.655791268906815,
-0.773156797467811));
#16220=CARTESIAN_POINT('Ctrl Pts',(30.8986989741888,-0.750666938273209,
-0.681074536321982));
#16221=CARTESIAN_POINT('Ctrl Pts',(30.8799881069201,-0.901467497815293,
-0.465863888580567));
#16222=CARTESIAN_POINT('Ctrl Pts',(30.8707427007773,-0.954288507126781,
-0.344674989241513));
#16223=CARTESIAN_POINT('Ctrl Pts',(30.8524577090853,-1.00848954053165,-0.0936168937764534));
#16224=CARTESIAN_POINT('Ctrl Pts',(30.8436316170097,-1.01254518840657,0.0325064994306721));
#16225=CARTESIAN_POINT('Ctrl Pts',(30.8246540986637,-0.972239735087881,
0.295767810922606));
#16226=CARTESIAN_POINT('Ctrl Pts',(30.8158947475416,-0.923830175985573,
0.411176324318523));
#16227=CARTESIAN_POINT('Ctrl Pts',(30.8083604951405,-0.870773402088998,
0.502739671065661));
#16228=CARTESIAN_POINT('Ctrl Pts',(32.55060539727,0.4091770629343,-0.9190267303885));
#16229=CARTESIAN_POINT('Ctrl Pts',(32.53435539727,0.2006565122657,-1.011866061022));
#16230=CARTESIAN_POINT('Ctrl Pts',(32.50185539727,-0.2811437402541,-1.049643553578));
#16231=CARTESIAN_POINT('Ctrl Pts',(32.45310539727,-0.8792134337482,-0.6387767584235));
#16232=CARTESIAN_POINT('Ctrl Pts',(32.40435539727,-1.0852291028,0.05687880443496));
#16233=CARTESIAN_POINT('Ctrl Pts',(32.35560539727,-0.8075980268285,0.7271613725661));
#16234=CARTESIAN_POINT('Ctrl Pts',(32.30685539727,-0.170000956467,1.073348045283));
#16235=CARTESIAN_POINT('Ctrl Pts',(32.25810539727,0.5433634217137,0.9411332701358));
#16236=CARTESIAN_POINT('Ctrl Pts',(32.20935539727,1.014547269612,0.3894482114171));
#16237=CARTESIAN_POINT('Ctrl Pts',(32.16060539727,1.033538954174,-0.3358171723489));
#16238=CARTESIAN_POINT('Ctrl Pts',(32.11185539727,0.5918740460484,-0.9114061000685));
#16239=CARTESIAN_POINT('Ctrl Pts',(32.06310539727,-0.1135939230171,-1.080773975495));
#16240=CARTESIAN_POINT('Ctrl Pts',(32.01435539727,-0.7684321582634,-0.7684321583925));
#16241=CARTESIAN_POINT('Ctrl Pts',(31.96560539727,-1.080773975171,-0.1135939221766));
#16242=CARTESIAN_POINT('Ctrl Pts',(31.91685539727,-0.9114061014946,0.5918740428154));
#16243=CARTESIAN_POINT('Ctrl Pts',(31.86810539727,-0.3358171669691,1.033538966266));
#16244=CARTESIAN_POINT('Ctrl Pts',(31.81935539727,0.3894481913237,1.014547224479));
#16245=CARTESIAN_POINT('Ctrl Pts',(31.77060539727,0.9411333451298,0.543363590154));
#16246=CARTESIAN_POINT('Ctrl Pts',(31.72185539727,1.0733477654,-0.1700015850955));
#16247=CARTESIAN_POINT('Ctrl Pts',(31.67310539727,0.7271624171027,-0.807595680755));
#16248=CARTESIAN_POINT('Ctrl Pts',(31.62435539727,0.05687490617145,-1.085237858466));
#16249=CARTESIAN_POINT('Ctrl Pts',(31.57560539727,-0.6387622099061,-0.8791807571591));
#16250=CARTESIAN_POINT('Ctrl Pts',(31.52685539727,-1.049697849384,-0.2812656909448));
#16251=CARTESIAN_POINT('Ctrl Pts',(31.47810539727,-0.9927746800367,0.4420117646994));
#16252=CARTESIAN_POINT('Ctrl Pts',(31.42935539727,-0.4933638127992,0.9682810097529));
#16253=CARTESIAN_POINT('Ctrl Pts',(31.38060539727,0.2259432748059,1.06297957629));
#16254=CARTESIAN_POINT('Ctrl Pts',(31.33185539727,0.8445456793518,0.6838996031158));
#16255=CARTESIAN_POINT('Ctrl Pts',(31.28310539727,1.086727031141,-1.083766177912E-7));
#16256=CARTESIAN_POINT('Ctrl Pts',(31.23435539727,0.8445461960836,-0.6838991696094));
#16257=CARTESIAN_POINT('Ctrl Pts',(31.18560539727,0.2259412078788,-1.062981093563));
#16258=CARTESIAN_POINT('Ctrl Pts',(31.13685539727,-0.4933560618227,-0.9682753741689));
#16259=CARTESIAN_POINT('Ctrl Pts',(31.08810539727,-0.9928036170159,-0.4420327897627));
#16260=CARTESIAN_POINT('Ctrl Pts',(31.03935539727,-1.049589852444,0.2813441556141));
#16261=CARTESIAN_POINT('Ctrl Pts',(31.00685539727,-0.7759734579398,0.6797066675681));
#16262=CARTESIAN_POINT('Ctrl Pts',(30.99060539727,-0.5913119638062,0.8138710963412));
#16263=CARTESIAN_POINT('Ctrl Pts',(32.46520179909,0.4091770629343,-0.9190267303885));
#16264=CARTESIAN_POINT('Ctrl Pts',(32.44895179909,0.2006565122657,-1.011866061022));
#16265=CARTESIAN_POINT('Ctrl Pts',(32.41645179909,-0.2811437402541,-1.049643553578));
#16266=CARTESIAN_POINT('Ctrl Pts',(32.36770179909,-0.8792134337482,-0.6387767584235));
#16267=CARTESIAN_POINT('Ctrl Pts',(32.31895179909,-1.0852291028,0.05687880443496));
#16268=CARTESIAN_POINT('Ctrl Pts',(32.27020179909,-0.8075980268285,0.7271613725661));
#16269=CARTESIAN_POINT('Ctrl Pts',(32.22145179909,-0.170000956467,1.073348045283));
#16270=CARTESIAN_POINT('Ctrl Pts',(32.17270179909,0.5433634217137,0.9411332701358));
#16271=CARTESIAN_POINT('Ctrl Pts',(32.12395179909,1.014547269612,0.3894482114171));
#16272=CARTESIAN_POINT('Ctrl Pts',(32.07520179909,1.033538954174,-0.3358171723489));
#16273=CARTESIAN_POINT('Ctrl Pts',(32.02645179909,0.5918740460484,-0.9114061000685));
#16274=CARTESIAN_POINT('Ctrl Pts',(31.97770179909,-0.1135939230171,-1.080773975495));
#16275=CARTESIAN_POINT('Ctrl Pts',(31.92895179909,-0.7684321582634,-0.7684321583925));
#16276=CARTESIAN_POINT('Ctrl Pts',(31.88020179909,-1.080773975171,-0.1135939221766));
#16277=CARTESIAN_POINT('Ctrl Pts',(31.83145179909,-0.9114061014946,0.5918740428154));
#16278=CARTESIAN_POINT('Ctrl Pts',(31.78270179909,-0.3358171669691,1.033538966266));
#16279=CARTESIAN_POINT('Ctrl Pts',(31.73395179909,0.3894481913237,1.014547224479));
#16280=CARTESIAN_POINT('Ctrl Pts',(31.68520179909,0.9411333451298,0.543363590154));
#16281=CARTESIAN_POINT('Ctrl Pts',(31.63645179909,1.0733477654,-0.1700015850955));
#16282=CARTESIAN_POINT('Ctrl Pts',(31.58770179909,0.7271624171027,-0.807595680755));
#16283=CARTESIAN_POINT('Ctrl Pts',(31.53895179909,0.05687490617145,-1.085237858466));
#16284=CARTESIAN_POINT('Ctrl Pts',(31.49020179909,-0.6387622099061,-0.8791807571591));
#16285=CARTESIAN_POINT('Ctrl Pts',(31.44145179909,-1.049697849384,-0.2812656909448));
#16286=CARTESIAN_POINT('Ctrl Pts',(31.39270179909,-0.9927746800367,0.4420117646994));
#16287=CARTESIAN_POINT('Ctrl Pts',(31.34395179909,-0.4933638127992,0.9682810097529));
#16288=CARTESIAN_POINT('Ctrl Pts',(31.29520179909,0.2259432748059,1.06297957629));
#16289=CARTESIAN_POINT('Ctrl Pts',(31.24645179909,0.8445456793518,0.6838996031158));
#16290=CARTESIAN_POINT('Ctrl Pts',(31.19770179909,1.086727031141,-1.083766177912E-7));
#16291=CARTESIAN_POINT('Ctrl Pts',(31.14895179909,0.8445461960836,-0.6838991696094));
#16292=CARTESIAN_POINT('Ctrl Pts',(31.10020179909,0.2259412078788,-1.062981093563));
#16293=CARTESIAN_POINT('Ctrl Pts',(31.05145179909,-0.4933560618227,-0.9682753741689));
#16294=CARTESIAN_POINT('Ctrl Pts',(31.00270179909,-0.9928036170159,-0.4420327897627));
#16295=CARTESIAN_POINT('Ctrl Pts',(30.95395179909,-1.049589852444,0.2813441556141));
#16296=CARTESIAN_POINT('Ctrl Pts',(30.92145179909,-0.7759734579398,0.6797066675681));
#16297=CARTESIAN_POINT('Ctrl Pts',(30.90520179909,-0.5913119638062,0.8138710963412));
#16298=CARTESIAN_POINT('Ctrl Pts',(32.37979820091,0.4091770629343,-0.9190267303885));
#16299=CARTESIAN_POINT('Ctrl Pts',(32.36354820091,0.2006565122657,-1.011866061022));
#16300=CARTESIAN_POINT('Ctrl Pts',(32.33104820091,-0.2811437402541,-1.049643553578));
#16301=CARTESIAN_POINT('Ctrl Pts',(32.28229820091,-0.8792134337482,-0.6387767584235));
#16302=CARTESIAN_POINT('Ctrl Pts',(32.23354820091,-1.0852291028,0.05687880443496));
#16303=CARTESIAN_POINT('Ctrl Pts',(32.18479820091,-0.8075980268285,0.7271613725661));
#16304=CARTESIAN_POINT('Ctrl Pts',(32.13604820091,-0.170000956467,1.073348045283));
#16305=CARTESIAN_POINT('Ctrl Pts',(32.08729820091,0.5433634217137,0.9411332701358));
#16306=CARTESIAN_POINT('Ctrl Pts',(32.03854820091,1.014547269612,0.3894482114171));
#16307=CARTESIAN_POINT('Ctrl Pts',(31.98979820091,1.033538954174,-0.3358171723489));
#16308=CARTESIAN_POINT('Ctrl Pts',(31.94104820091,0.5918740460484,-0.9114061000685));
#16309=CARTESIAN_POINT('Ctrl Pts',(31.89229820091,-0.1135939230171,-1.080773975495));
#16310=CARTESIAN_POINT('Ctrl Pts',(31.84354820091,-0.7684321582634,-0.7684321583925));
#16311=CARTESIAN_POINT('Ctrl Pts',(31.79479820091,-1.080773975171,-0.1135939221766));
#16312=CARTESIAN_POINT('Ctrl Pts',(31.74604820091,-0.9114061014946,0.5918740428154));
#16313=CARTESIAN_POINT('Ctrl Pts',(31.69729820091,-0.3358171669691,1.033538966266));
#16314=CARTESIAN_POINT('Ctrl Pts',(31.64854820091,0.3894481913237,1.014547224479));
#16315=CARTESIAN_POINT('Ctrl Pts',(31.59979820091,0.9411333451298,0.543363590154));
#16316=CARTESIAN_POINT('Ctrl Pts',(31.55104820091,1.0733477654,-0.1700015850955));
#16317=CARTESIAN_POINT('Ctrl Pts',(31.50229820091,0.7271624171027,-0.807595680755));
#16318=CARTESIAN_POINT('Ctrl Pts',(31.45354820091,0.05687490617145,-1.085237858466));
#16319=CARTESIAN_POINT('Ctrl Pts',(31.40479820091,-0.6387622099061,-0.8791807571591));
#16320=CARTESIAN_POINT('Ctrl Pts',(31.35604820091,-1.049697849384,-0.2812656909448));
#16321=CARTESIAN_POINT('Ctrl Pts',(31.30729820091,-0.9927746800367,0.4420117646994));
#16322=CARTESIAN_POINT('Ctrl Pts',(31.25854820091,-0.4933638127992,0.9682810097529));
#16323=CARTESIAN_POINT('Ctrl Pts',(31.20979820091,0.2259432748059,1.06297957629));
#16324=CARTESIAN_POINT('Ctrl Pts',(31.16104820091,0.8445456793518,0.6838996031158));
#16325=CARTESIAN_POINT('Ctrl Pts',(31.11229820091,1.086727031141,-1.083766177912E-7));
#16326=CARTESIAN_POINT('Ctrl Pts',(31.06354820091,0.8445461960836,-0.6838991696094));
#16327=CARTESIAN_POINT('Ctrl Pts',(31.01479820091,0.2259412078788,-1.062981093563));
#16328=CARTESIAN_POINT('Ctrl Pts',(30.96604820091,-0.4933560618227,-0.9682753741689));
#16329=CARTESIAN_POINT('Ctrl Pts',(30.91729820091,-0.9928036170159,-0.4420327897627));
#16330=CARTESIAN_POINT('Ctrl Pts',(30.86854820091,-1.049589852444,0.2813441556141));
#16331=CARTESIAN_POINT('Ctrl Pts',(30.83604820091,-0.7759734579398,0.6797066675681));
#16332=CARTESIAN_POINT('Ctrl Pts',(30.81979820091,-0.5913119638062,0.8138710963412));
#16333=CARTESIAN_POINT('Ctrl Pts',(32.29439460273,0.4091770629343,-0.9190267303885));
#16334=CARTESIAN_POINT('Ctrl Pts',(32.27814460273,0.2006565122657,-1.011866061022));
#16335=CARTESIAN_POINT('Ctrl Pts',(32.24564460273,-0.2811437402541,-1.049643553578));
#16336=CARTESIAN_POINT('Ctrl Pts',(32.19689460273,-0.8792134337482,-0.6387767584235));
#16337=CARTESIAN_POINT('Ctrl Pts',(32.14814460273,-1.0852291028,0.05687880443496));
#16338=CARTESIAN_POINT('Ctrl Pts',(32.09939460273,-0.8075980268285,0.7271613725661));
#16339=CARTESIAN_POINT('Ctrl Pts',(32.05064460273,-0.170000956467,1.073348045283));
#16340=CARTESIAN_POINT('Ctrl Pts',(32.00189460273,0.5433634217137,0.9411332701358));
#16341=CARTESIAN_POINT('Ctrl Pts',(31.95314460273,1.014547269612,0.3894482114171));
#16342=CARTESIAN_POINT('Ctrl Pts',(31.90439460273,1.033538954174,-0.3358171723489));
#16343=CARTESIAN_POINT('Ctrl Pts',(31.85564460273,0.5918740460484,-0.9114061000685));
#16344=CARTESIAN_POINT('Ctrl Pts',(31.80689460273,-0.1135939230171,-1.080773975495));
#16345=CARTESIAN_POINT('Ctrl Pts',(31.75814460273,-0.7684321582634,-0.7684321583925));
#16346=CARTESIAN_POINT('Ctrl Pts',(31.70939460273,-1.080773975171,-0.1135939221766));
#16347=CARTESIAN_POINT('Ctrl Pts',(31.66064460273,-0.9114061014946,0.5918740428154));
#16348=CARTESIAN_POINT('Ctrl Pts',(31.61189460273,-0.3358171669691,1.033538966266));
#16349=CARTESIAN_POINT('Ctrl Pts',(31.56314460273,0.3894481913237,1.014547224479));
#16350=CARTESIAN_POINT('Ctrl Pts',(31.51439460273,0.9411333451298,0.543363590154));
#16351=CARTESIAN_POINT('Ctrl Pts',(31.46564460273,1.0733477654,-0.1700015850955));
#16352=CARTESIAN_POINT('Ctrl Pts',(31.41689460273,0.7271624171027,-0.807595680755));
#16353=CARTESIAN_POINT('Ctrl Pts',(31.36814460273,0.05687490617145,-1.085237858466));
#16354=CARTESIAN_POINT('Ctrl Pts',(31.31939460273,-0.6387622099061,-0.8791807571591));
#16355=CARTESIAN_POINT('Ctrl Pts',(31.27064460273,-1.049697849384,-0.2812656909448));
#16356=CARTESIAN_POINT('Ctrl Pts',(31.22189460273,-0.9927746800367,0.4420117646994));
#16357=CARTESIAN_POINT('Ctrl Pts',(31.17314460273,-0.4933638127992,0.9682810097529));
#16358=CARTESIAN_POINT('Ctrl Pts',(31.12439460273,0.2259432748059,1.06297957629));
#16359=CARTESIAN_POINT('Ctrl Pts',(31.07564460273,0.8445456793518,0.6838996031158));
#16360=CARTESIAN_POINT('Ctrl Pts',(31.02689460273,1.086727031141,-1.083766177912E-7));
#16361=CARTESIAN_POINT('Ctrl Pts',(30.97814460273,0.8445461960836,-0.6838991696094));
#16362=CARTESIAN_POINT('Ctrl Pts',(30.92939460273,0.2259412078788,-1.062981093563));
#16363=CARTESIAN_POINT('Ctrl Pts',(30.88064460273,-0.4933560618227,-0.9682753741689));
#16364=CARTESIAN_POINT('Ctrl Pts',(30.83189460273,-0.9928036170159,-0.4420327897627));
#16365=CARTESIAN_POINT('Ctrl Pts',(30.78314460273,-1.049589852444,0.2813441556141));
#16366=CARTESIAN_POINT('Ctrl Pts',(30.75064460273,-0.7759734579398,0.6797066675681));
#16367=CARTESIAN_POINT('Ctrl Pts',(30.73439460273,-0.5913119638062,0.8138710963412));
#16368=CARTESIAN_POINT('',(30.97662653432,-0.8712215562071,0.503));
#16369=CARTESIAN_POINT('Ctrl Pts',(31.05060539727,-1.00048902674,0.1051556340473));
#16370=CARTESIAN_POINT('Ctrl Pts',(31.03435539727,-0.9766299702056,0.3321593934543));
#16371=CARTESIAN_POINT('Ctrl Pts',(31.00185539727,-0.7684461121902,0.7682993979641));
#16372=CARTESIAN_POINT('Ctrl Pts',(30.95310539727,-0.1135901832678,1.080809548186));
#16373=CARTESIAN_POINT('Ctrl Pts',(30.90435539727,0.5918730409778,0.9113965697339));
#16374=CARTESIAN_POINT('Ctrl Pts',(30.85560539727,1.033539234707,0.3358197209966));
#16375=CARTESIAN_POINT('Ctrl Pts',(30.80685539727,1.014547152551,-0.3894488756732));
#16376=CARTESIAN_POINT('Ctrl Pts',(30.75810539727,0.5433636094275,-0.9411331617592));
#16377=CARTESIAN_POINT('Ctrl Pts',(30.70935539727,-0.1700015902605,-1.073347814533));
#16378=CARTESIAN_POINT('Ctrl Pts',(30.66060539727,-0.8075956793684,-0.7271624039412));
#16379=CARTESIAN_POINT('Ctrl Pts',(30.61185539727,-1.085237858848,-0.05687490968431));
#16380=CARTESIAN_POINT('Ctrl Pts',(30.56310539727,-0.8791807570196,0.6387622107961));
#16381=CARTESIAN_POINT('Ctrl Pts',(30.51435539727,-0.2812656911211,1.049697849337));
#16382=CARTESIAN_POINT('Ctrl Pts',(30.46560539727,0.4420117652652,0.9927746793357));
#16383=CARTESIAN_POINT('Ctrl Pts',(30.41685539727,0.968281007666,0.4933638156507));
#16384=CARTESIAN_POINT('Ctrl Pts',(30.36810539727,1.062979584072,-0.2259432855107));
#16385=CARTESIAN_POINT('Ctrl Pts',(30.31935539727,0.6838995740763,-0.8445456393839));
#16386=CARTESIAN_POINT('Ctrl Pts',(30.27060539727,-1.795785742331E-14,-1.086727180308));
#16387=CARTESIAN_POINT('Ctrl Pts',(30.22185539727,-0.6838995740763,-0.8445456393839));
#16388=CARTESIAN_POINT('Ctrl Pts',(30.17310539727,-1.062979584072,-0.2259432855107));
#16389=CARTESIAN_POINT('Ctrl Pts',(30.12435539727,-0.968281007666,0.4933638156508));
#16390=CARTESIAN_POINT('Ctrl Pts',(30.07560539727,-0.4420117652651,0.9927746793357));
#16391=CARTESIAN_POINT('Ctrl Pts',(30.02685539727,0.2812656911211,1.049697849337));
#16392=CARTESIAN_POINT('Ctrl Pts',(29.97810539727,0.8791807570196,0.6387622107961));
#16393=CARTESIAN_POINT('Ctrl Pts',(29.92935539727,1.085237858848,-0.05687490968435));
#16394=CARTESIAN_POINT('Ctrl Pts',(29.88060539727,0.8075956793683,-0.7271624039412));
#16395=CARTESIAN_POINT('Ctrl Pts',(29.83185539727,0.1700015902605,-1.073347814533));
#16396=CARTESIAN_POINT('Ctrl Pts',(29.78310539727,-0.5433636094275,-0.9411331617592));
#16397=CARTESIAN_POINT('Ctrl Pts',(29.73435539727,-1.014547152551,-0.3894488756732));
#16398=CARTESIAN_POINT('Ctrl Pts',(29.68560539727,-1.033539234707,0.3358197209966));
#16399=CARTESIAN_POINT('Ctrl Pts',(29.63685539727,-0.5918730409778,0.9113965697339));
#16400=CARTESIAN_POINT('Ctrl Pts',(29.58810539727,0.1135901832678,1.080809548186));
#16401=CARTESIAN_POINT('Ctrl Pts',(29.53935539727,0.7684461121903,0.7682993979641));
#16402=CARTESIAN_POINT('Ctrl Pts',(29.50685539727,0.9766299702056,0.3321593934543));
#16403=CARTESIAN_POINT('Ctrl Pts',(29.49060539727,1.00048902674,0.1051556340472));
#16404=CARTESIAN_POINT('Ctrl Pts',(30.96520179909,-1.00048902674,0.1051556340473));
#16405=CARTESIAN_POINT('Ctrl Pts',(30.94895179909,-0.9766299702056,0.3321593934543));
#16406=CARTESIAN_POINT('Ctrl Pts',(30.91645179909,-0.7684461121902,0.7682993979641));
#16407=CARTESIAN_POINT('Ctrl Pts',(30.86770179909,-0.1135901832678,1.080809548186));
#16408=CARTESIAN_POINT('Ctrl Pts',(30.81895179909,0.5918730409778,0.9113965697339));
#16409=CARTESIAN_POINT('Ctrl Pts',(30.77020179909,1.033539234707,0.3358197209966));
#16410=CARTESIAN_POINT('Ctrl Pts',(30.72145179909,1.014547152551,-0.3894488756732));
#16411=CARTESIAN_POINT('Ctrl Pts',(30.67270179909,0.5433636094275,-0.9411331617592));
#16412=CARTESIAN_POINT('Ctrl Pts',(30.62395179909,-0.1700015902605,-1.073347814533));
#16413=CARTESIAN_POINT('Ctrl Pts',(30.57520179909,-0.8075956793684,-0.7271624039412));
#16414=CARTESIAN_POINT('Ctrl Pts',(30.52645179909,-1.085237858848,-0.05687490968431));
#16415=CARTESIAN_POINT('Ctrl Pts',(30.47770179909,-0.8791807570196,0.6387622107961));
#16416=CARTESIAN_POINT('Ctrl Pts',(30.42895179909,-0.2812656911211,1.049697849337));
#16417=CARTESIAN_POINT('Ctrl Pts',(30.38020179909,0.4420117652652,0.9927746793357));
#16418=CARTESIAN_POINT('Ctrl Pts',(30.33145179909,0.968281007666,0.4933638156507));
#16419=CARTESIAN_POINT('Ctrl Pts',(30.28270179909,1.062979584072,-0.2259432855107));
#16420=CARTESIAN_POINT('Ctrl Pts',(30.23395179909,0.6838995740763,-0.8445456393839));
#16421=CARTESIAN_POINT('Ctrl Pts',(30.18520179909,-1.795785742331E-14,-1.086727180308));
#16422=CARTESIAN_POINT('Ctrl Pts',(30.13645179909,-0.6838995740763,-0.8445456393839));
#16423=CARTESIAN_POINT('Ctrl Pts',(30.08770179909,-1.062979584072,-0.2259432855107));
#16424=CARTESIAN_POINT('Ctrl Pts',(30.03895179909,-0.968281007666,0.4933638156508));
#16425=CARTESIAN_POINT('Ctrl Pts',(29.99020179909,-0.4420117652651,0.9927746793357));
#16426=CARTESIAN_POINT('Ctrl Pts',(29.94145179909,0.2812656911211,1.049697849337));
#16427=CARTESIAN_POINT('Ctrl Pts',(29.89270179909,0.8791807570196,0.6387622107961));
#16428=CARTESIAN_POINT('Ctrl Pts',(29.84395179909,1.085237858848,-0.05687490968435));
#16429=CARTESIAN_POINT('Ctrl Pts',(29.79520179909,0.8075956793683,-0.7271624039412));
#16430=CARTESIAN_POINT('Ctrl Pts',(29.74645179909,0.1700015902605,-1.073347814533));
#16431=CARTESIAN_POINT('Ctrl Pts',(29.69770179909,-0.5433636094275,-0.9411331617592));
#16432=CARTESIAN_POINT('Ctrl Pts',(29.64895179909,-1.014547152551,-0.3894488756732));
#16433=CARTESIAN_POINT('Ctrl Pts',(29.60020179909,-1.033539234707,0.3358197209966));
#16434=CARTESIAN_POINT('Ctrl Pts',(29.55145179909,-0.5918730409778,0.9113965697339));
#16435=CARTESIAN_POINT('Ctrl Pts',(29.50270179909,0.1135901832678,1.080809548186));
#16436=CARTESIAN_POINT('Ctrl Pts',(29.45395179909,0.7684461121903,0.7682993979641));
#16437=CARTESIAN_POINT('Ctrl Pts',(29.42145179909,0.9766299702056,0.3321593934543));
#16438=CARTESIAN_POINT('Ctrl Pts',(29.40520179909,1.00048902674,0.1051556340472));
#16439=CARTESIAN_POINT('Ctrl Pts',(30.87979820091,-1.00048902674,0.1051556340473));
#16440=CARTESIAN_POINT('Ctrl Pts',(30.86354820091,-0.9766299702056,0.3321593934543));
#16441=CARTESIAN_POINT('Ctrl Pts',(30.83104820091,-0.7684461121902,0.7682993979641));
#16442=CARTESIAN_POINT('Ctrl Pts',(30.78229820091,-0.1135901832678,1.080809548186));
#16443=CARTESIAN_POINT('Ctrl Pts',(30.73354820091,0.5918730409778,0.9113965697339));
#16444=CARTESIAN_POINT('Ctrl Pts',(30.68479820091,1.033539234707,0.3358197209966));
#16445=CARTESIAN_POINT('Ctrl Pts',(30.63604820091,1.014547152551,-0.3894488756732));
#16446=CARTESIAN_POINT('Ctrl Pts',(30.58729820091,0.5433636094275,-0.9411331617592));
#16447=CARTESIAN_POINT('Ctrl Pts',(30.53854820091,-0.1700015902605,-1.073347814533));
#16448=CARTESIAN_POINT('Ctrl Pts',(30.48979820091,-0.8075956793684,-0.7271624039412));
#16449=CARTESIAN_POINT('Ctrl Pts',(30.44104820091,-1.085237858848,-0.05687490968431));
#16450=CARTESIAN_POINT('Ctrl Pts',(30.39229820091,-0.8791807570196,0.6387622107961));
#16451=CARTESIAN_POINT('Ctrl Pts',(30.34354820091,-0.2812656911211,1.049697849337));
#16452=CARTESIAN_POINT('Ctrl Pts',(30.29479820091,0.4420117652652,0.9927746793357));
#16453=CARTESIAN_POINT('Ctrl Pts',(30.24604820091,0.968281007666,0.4933638156507));
#16454=CARTESIAN_POINT('Ctrl Pts',(30.19729820091,1.062979584072,-0.2259432855107));
#16455=CARTESIAN_POINT('Ctrl Pts',(30.14854820091,0.6838995740763,-0.8445456393839));
#16456=CARTESIAN_POINT('Ctrl Pts',(30.09979820091,-1.795785742331E-14,-1.086727180308));
#16457=CARTESIAN_POINT('Ctrl Pts',(30.05104820091,-0.6838995740763,-0.8445456393839));
#16458=CARTESIAN_POINT('Ctrl Pts',(30.00229820091,-1.062979584072,-0.2259432855107));
#16459=CARTESIAN_POINT('Ctrl Pts',(29.95354820091,-0.968281007666,0.4933638156508));
#16460=CARTESIAN_POINT('Ctrl Pts',(29.90479820091,-0.4420117652651,0.9927746793357));
#16461=CARTESIAN_POINT('Ctrl Pts',(29.85604820091,0.2812656911211,1.049697849337));
#16462=CARTESIAN_POINT('Ctrl Pts',(29.80729820091,0.8791807570196,0.6387622107961));
#16463=CARTESIAN_POINT('Ctrl Pts',(29.75854820091,1.085237858848,-0.05687490968435));
#16464=CARTESIAN_POINT('Ctrl Pts',(29.70979820091,0.8075956793683,-0.7271624039412));
#16465=CARTESIAN_POINT('Ctrl Pts',(29.66104820091,0.1700015902605,-1.073347814533));
#16466=CARTESIAN_POINT('Ctrl Pts',(29.61229820091,-0.5433636094275,-0.9411331617592));
#16467=CARTESIAN_POINT('Ctrl Pts',(29.56354820091,-1.014547152551,-0.3894488756732));
#16468=CARTESIAN_POINT('Ctrl Pts',(29.51479820091,-1.033539234707,0.3358197209966));
#16469=CARTESIAN_POINT('Ctrl Pts',(29.46604820091,-0.5918730409778,0.9113965697339));
#16470=CARTESIAN_POINT('Ctrl Pts',(29.41729820091,0.1135901832678,1.080809548186));
#16471=CARTESIAN_POINT('Ctrl Pts',(29.36854820091,0.7684461121903,0.7682993979641));
#16472=CARTESIAN_POINT('Ctrl Pts',(29.33604820091,0.9766299702056,0.3321593934543));
#16473=CARTESIAN_POINT('Ctrl Pts',(29.31979820091,1.00048902674,0.1051556340472));
#16474=CARTESIAN_POINT('Ctrl Pts',(30.79439460273,-1.00048902674,0.1051556340473));
#16475=CARTESIAN_POINT('Ctrl Pts',(30.77814460273,-0.9766299702056,0.3321593934543));
#16476=CARTESIAN_POINT('Ctrl Pts',(30.74564460273,-0.7684461121902,0.7682993979641));
#16477=CARTESIAN_POINT('Ctrl Pts',(30.69689460273,-0.1135901832678,1.080809548186));
#16478=CARTESIAN_POINT('Ctrl Pts',(30.64814460273,0.5918730409778,0.9113965697339));
#16479=CARTESIAN_POINT('Ctrl Pts',(30.59939460273,1.033539234707,0.3358197209966));
#16480=CARTESIAN_POINT('Ctrl Pts',(30.55064460273,1.014547152551,-0.3894488756732));
#16481=CARTESIAN_POINT('Ctrl Pts',(30.50189460273,0.5433636094275,-0.9411331617592));
#16482=CARTESIAN_POINT('Ctrl Pts',(30.45314460273,-0.1700015902605,-1.073347814533));
#16483=CARTESIAN_POINT('Ctrl Pts',(30.40439460273,-0.8075956793684,-0.7271624039412));
#16484=CARTESIAN_POINT('Ctrl Pts',(30.35564460273,-1.085237858848,-0.05687490968431));
#16485=CARTESIAN_POINT('Ctrl Pts',(30.30689460273,-0.8791807570196,0.6387622107961));
#16486=CARTESIAN_POINT('Ctrl Pts',(30.25814460273,-0.2812656911211,1.049697849337));
#16487=CARTESIAN_POINT('Ctrl Pts',(30.20939460273,0.4420117652652,0.9927746793357));
#16488=CARTESIAN_POINT('Ctrl Pts',(30.16064460273,0.968281007666,0.4933638156507));
#16489=CARTESIAN_POINT('Ctrl Pts',(30.11189460273,1.062979584072,-0.2259432855107));
#16490=CARTESIAN_POINT('Ctrl Pts',(30.06314460273,0.6838995740763,-0.8445456393839));
#16491=CARTESIAN_POINT('Ctrl Pts',(30.01439460273,-1.795785742331E-14,-1.086727180308));
#16492=CARTESIAN_POINT('Ctrl Pts',(29.96564460273,-0.6838995740763,-0.8445456393839));
#16493=CARTESIAN_POINT('Ctrl Pts',(29.91689460273,-1.062979584072,-0.2259432855107));
#16494=CARTESIAN_POINT('Ctrl Pts',(29.86814460273,-0.968281007666,0.4933638156508));
#16495=CARTESIAN_POINT('Ctrl Pts',(29.81939460273,-0.4420117652651,0.9927746793357));
#16496=CARTESIAN_POINT('Ctrl Pts',(29.77064460273,0.2812656911211,1.049697849337));
#16497=CARTESIAN_POINT('Ctrl Pts',(29.72189460273,0.8791807570196,0.6387622107961));
#16498=CARTESIAN_POINT('Ctrl Pts',(29.67314460273,1.085237858848,-0.05687490968435));
#16499=CARTESIAN_POINT('Ctrl Pts',(29.62439460273,0.8075956793683,-0.7271624039412));
#16500=CARTESIAN_POINT('Ctrl Pts',(29.57564460273,0.1700015902605,-1.073347814533));
#16501=CARTESIAN_POINT('Ctrl Pts',(29.52689460273,-0.5433636094275,-0.9411331617592));
#16502=CARTESIAN_POINT('Ctrl Pts',(29.47814460273,-1.014547152551,-0.3894488756732));
#16503=CARTESIAN_POINT('Ctrl Pts',(29.42939460273,-1.033539234707,0.3358197209966));
#16504=CARTESIAN_POINT('Ctrl Pts',(29.38064460273,-0.5918730409778,0.9113965697339));
#16505=CARTESIAN_POINT('Ctrl Pts',(29.33189460273,0.1135901832678,1.080809548186));
#16506=CARTESIAN_POINT('Ctrl Pts',(29.28314460273,0.7684461121903,0.7682993979641));
#16507=CARTESIAN_POINT('Ctrl Pts',(29.25064460273,0.9766299702056,0.3321593934543));
#16508=CARTESIAN_POINT('Ctrl Pts',(29.23439460273,1.00048902674,0.1051556340472));
#16509=CARTESIAN_POINT('',(29.308373466651,0.871221485691904,0.502999959536925));
#16510=CARTESIAN_POINT('Ctrl Pts',(30.8083864422337,-0.870772069750912,
0.502741978477052));
#16511=CARTESIAN_POINT('Ctrl Pts',(30.8008521885261,-0.818004270752092,
0.594472186190461));
#16512=CARTESIAN_POINT('Ctrl Pts',(30.7920928354003,-0.74226233496147,0.694100380026428));
#16513=CARTESIAN_POINT('Ctrl Pts',(30.7731153143573,-0.534424048498561,
0.860636605924475));
#16514=CARTESIAN_POINT('Ctrl Pts',(30.7642892222818,-0.423170162032183,
0.920186008439541));
#16515=CARTESIAN_POINT('Ctrl Pts',(30.7460042305897,-0.178646956831074,
0.998775584332035));
#16516=CARTESIAN_POINT('Ctrl Pts',(30.7367588244469,-0.0472837866908757,
1.01362569808423));
#16517=CARTESIAN_POINT('Ctrl Pts',(30.7180479571781,0.214494381189115,0.990633906486489));
#16518=CARTESIAN_POINT('Ctrl Pts',(30.7088151157514,0.341677793262393,0.954510297187085));
#16519=CARTESIAN_POINT('Ctrl Pts',(30.6886171121704,0.594508302867244,0.826283085072341));
#16520=CARTESIAN_POINT('Ctrl Pts',(30.6792516786672,0.693921902387751,0.736013762237494));
#16521=CARTESIAN_POINT('Ctrl Pts',(30.6624059009715,0.847217927666136,0.555636629667067));
#16522=CARTESIAN_POINT('Ctrl Pts',(30.6534069464233,0.911379127217043,0.4441108841133));
#16523=CARTESIAN_POINT('Ctrl Pts',(30.6342989682698,0.998002528379833,0.190430974375329));
#16524=CARTESIAN_POINT('Ctrl Pts',(30.6247947693779,1.01157017614526,0.0548890692946352));
#16525=CARTESIAN_POINT('Ctrl Pts',(30.6082077163493,0.995521631670858,-0.17764597144364));
#16526=CARTESIAN_POINT('Ctrl Pts',(30.5990210738254,0.970098454855203,-0.306791753619249));
#16527=CARTESIAN_POINT('Ctrl Pts',(30.5788719338335,0.845240586957547,-0.560500408959282));
#16528=CARTESIAN_POINT('Ctrl Pts',(30.5694606001009,0.763151979773334,-0.667500700456631));
#16529=CARTESIAN_POINT('Ctrl Pts',(30.5505675506108,0.564358031936664,-0.843275682317893));
#16530=CARTESIAN_POINT('Ctrl Pts',(30.5413142276786,0.449835071540398,-0.909552155701698));
#16531=CARTESIAN_POINT('Ctrl Pts',(30.5226106191189,0.200891944607366,-0.993435412233473));
#16532=CARTESIAN_POINT('Ctrl Pts',(30.5133914653587,0.0701110249796663,
-1.01138590544987));
#16533=CARTESIAN_POINT('Ctrl Pts',(30.4931854475347,-0.213025964557814,
-0.995444387176705));
#16534=CARTESIAN_POINT('Ctrl Pts',(30.483806736634,-0.34046753425378,-0.952477692807911));
#16535=CARTESIAN_POINT('Ctrl Pts',(30.4670009367566,-0.552782663940084,
-0.84906487250493));
#16536=CARTESIAN_POINT('Ctrl Pts',(30.45801688248,-0.656165051344275,-0.772850244059696));
#16537=CARTESIAN_POINT('Ctrl Pts',(30.4394916971384,-0.831881844613014,
-0.581371288177416));
#16538=CARTESIAN_POINT('Ctrl Pts',(30.4299862507459,-0.901486061152791,
-0.464335182585286));
#16539=CARTESIAN_POINT('Ctrl Pts',(30.4128021772268,-0.983138694974887,
-0.237085248117362));
#16540=CARTESIAN_POINT('Ctrl Pts',(30.4036116032871,-1.01164457155601,-0.108534779049115));
#16541=CARTESIAN_POINT('Ctrl Pts',(30.3834719027531,-0.99914720466093,0.17383498727286));
#16542=CARTESIAN_POINT('Ctrl Pts',(30.3740686495797,-0.967009114614636,
0.304690319176165));
#16543=CARTESIAN_POINT('Ctrl Pts',(30.3551692839619,-0.855581407083058,
0.545608350968359));
#16544=CARTESIAN_POINT('Ctrl Pts',(30.3459048150743,-0.777163779775291,
0.652387656279846));
#16545=CARTESIAN_POINT('Ctrl Pts',(30.3272137745115,-0.582980235794567,
0.829064401206589));
#16546=CARTESIAN_POINT('Ctrl Pts',(30.3180068956466,-0.470601448908796,
0.897970498795624));
#16547=CARTESIAN_POINT('Ctrl Pts',(30.2977899305544,-0.204799025246617,
0.997222455929395));
#16548=CARTESIAN_POINT('Ctrl Pts',(30.2883977032763,-0.07061115429442,1.0089765786811));
#16549=CARTESIAN_POINT('Ctrl Pts',(30.2716308252545,0.164820890836547,0.999641820194012));
#16550=CARTESIAN_POINT('Ctrl Pts',(30.2626606378465,0.289920670515312,0.971492512618052));
#16551=CARTESIAN_POINT('Ctrl Pts',(30.2441622029206,0.527466569099338,0.867007573502011));
#16552=CARTESIAN_POINT('Ctrl Pts',(30.2346587869632,0.638304838566819,0.787948218222781));
#16553=CARTESIAN_POINT('Ctrl Pts',(30.2174342420197,0.804917354004863,0.612382577780543));
#16554=CARTESIAN_POINT('Ctrl Pts',(30.2082400320689,0.882667521494572,0.506058560714851));
#16555=CARTESIAN_POINT('Ctrl Pts',(30.1881085385381,0.984682436642582,0.242576766412211));
#16556=CARTESIAN_POINT('Ctrl Pts',(30.1787128604578,1.00788845481734,0.109958040776812));
#16557=CARTESIAN_POINT('Ctrl Pts',(30.1598090757102,1.00280273292441,-0.155484472839208));
#16558=CARTESIAN_POINT('Ctrl Pts',(30.1505332144177,0.973839811222991,-0.284930092981155));
#16559=CARTESIAN_POINT('Ctrl Pts',(30.1318547354579,0.867144006061644,-0.524617833052899));
#16560=CARTESIAN_POINT('Ctrl Pts',(30.1226591218941,0.792089695015471,-0.632780197940589));
#16561=CARTESIAN_POINT('Ctrl Pts',(30.1024311543348,0.588587875794969,-0.830697511597098));
#16562=CARTESIAN_POINT('Ctrl Pts',(30.093026368846,0.470235006290618,-0.895430023340954));
#16563=CARTESIAN_POINT('Ctrl Pts',(30.0762958650647,0.251421288995113,-0.981433054835685));
#16564=CARTESIAN_POINT('Ctrl Pts',(30.0673383109915,0.12576520800403,-1.00599999999997));
#16565=CARTESIAN_POINT('Ctrl Pts',(30.0494086203685,-0.125765208004121,
-1.00599999999996));
#16566=CARTESIAN_POINT('Ctrl Pts',(30.0404510663023,-0.251421288995195,
-0.98143305483567));
#16567=CARTESIAN_POINT('Ctrl Pts',(30.0237205625209,-0.470235006290693,
-0.895430023340922));
#16568=CARTESIAN_POINT('Ctrl Pts',(30.0143157770321,-0.588587875795033,
-0.830697511597058));
#16569=CARTESIAN_POINT('Ctrl Pts',(29.9940878094728,-0.79208969501552,-0.63278019794053));
#16570=CARTESIAN_POINT('Ctrl Pts',(29.984892195909,-0.867144006061687,-0.524617833052829));
#16571=CARTESIAN_POINT('Ctrl Pts',(29.9662137169491,-0.973839811223016,
-0.28493009298106));
#16572=CARTESIAN_POINT('Ctrl Pts',(29.9569378556566,-1.00280273292442,-0.155484472839104));
#16573=CARTESIAN_POINT('Ctrl Pts',(29.938034070909,-1.00788845481734,0.109958040776938));
#16574=CARTESIAN_POINT('Ctrl Pts',(29.9286383928286,-0.984682436642559,
0.242576766412358));
#16575=CARTESIAN_POINT('Ctrl Pts',(29.9085068992979,-0.882667521494521,
0.506058560714965));
#16576=CARTESIAN_POINT('Ctrl Pts',(29.8993126893471,-0.804917354004816,
0.61238257778062));
#16577=CARTESIAN_POINT('Ctrl Pts',(29.8820881444036,-0.638304838566773,
0.787948218222813));
#16578=CARTESIAN_POINT('Ctrl Pts',(29.8725847284462,-0.527466569099291,
0.867007573502023));
#16579=CARTESIAN_POINT('Ctrl Pts',(29.8540862935204,-0.289920670515246,
0.971492512618064));
#16580=CARTESIAN_POINT('Ctrl Pts',(29.8451161061125,-0.164820890836453,
0.999641820194026));
#16581=CARTESIAN_POINT('Ctrl Pts',(29.8283492280908,0.0706111542945384,
1.00897657868109));
#16582=CARTESIAN_POINT('Ctrl Pts',(29.8189570008127,0.204799025246714,0.997222455929378));
#16583=CARTESIAN_POINT('Ctrl Pts',(29.7987400357205,0.470601448908869,0.897970498795589));
#16584=CARTESIAN_POINT('Ctrl Pts',(29.7895331568555,0.582980235794636,0.829064401206542));
#16585=CARTESIAN_POINT('Ctrl Pts',(29.7708421162926,0.777163779775349,0.652387656279774));
#16586=CARTESIAN_POINT('Ctrl Pts',(29.7615776474049,0.855581407083106,0.545608350968274));
#16587=CARTESIAN_POINT('Ctrl Pts',(29.7426782817869,0.967009114614662,0.30469031917606));
#16588=CARTESIAN_POINT('Ctrl Pts',(29.7332750286134,0.999147204660943,0.173834987272742));
#16589=CARTESIAN_POINT('Ctrl Pts',(29.7131353280793,1.01164457155598,-0.108534779049213));
#16590=CARTESIAN_POINT('Ctrl Pts',(29.7039447541397,0.983138694974841,-0.237085248117433));
#16591=CARTESIAN_POINT('Ctrl Pts',(29.6867606806207,0.901486061152719,-0.464335182585334));
#16592=CARTESIAN_POINT('Ctrl Pts',(29.6772552342284,0.831881844612926,-0.581371288177457));
#16593=CARTESIAN_POINT('Ctrl Pts',(29.6587300488869,0.656165051344154,-0.772850244059751));
#16594=CARTESIAN_POINT('Ctrl Pts',(29.6497459946103,0.552782663939933,-0.849064872504999));
#16595=CARTESIAN_POINT('Ctrl Pts',(29.6329401947329,0.340467534253599,-0.952477692807964));
#16596=CARTESIAN_POINT('Ctrl Pts',(29.6235614838323,0.213025964557654,-0.995444387176732));
#16597=CARTESIAN_POINT('Ctrl Pts',(29.6033554660083,-0.0701110249797902,
-1.01138590544986));
#16598=CARTESIAN_POINT('Ctrl Pts',(29.594136312248,-0.20089194460748,-0.993435412233449));
#16599=CARTESIAN_POINT('Ctrl Pts',(29.5754327036883,-0.449835071540499,
-0.909552155701649));
#16600=CARTESIAN_POINT('Ctrl Pts',(29.5661793807561,-0.564358031936759,
-0.843275682317829));
#16601=CARTESIAN_POINT('Ctrl Pts',(29.5472863312659,-0.763151979773412,
-0.667500700456543));
#16602=CARTESIAN_POINT('Ctrl Pts',(29.5378749975332,-0.845240586957616,
-0.560500408959181));
#16603=CARTESIAN_POINT('Ctrl Pts',(29.5177258575413,-0.970098454855238,
-0.306791753619133));
#16604=CARTESIAN_POINT('Ctrl Pts',(29.5085392150175,-0.995521631670878,
-0.177645971443525));
#16605=CARTESIAN_POINT('Ctrl Pts',(29.491952161989,-1.01157017614525,0.0548890692947026));
#16606=CARTESIAN_POINT('Ctrl Pts',(29.4824479630973,-0.998002528379827,
0.190430974375389));
#16607=CARTESIAN_POINT('Ctrl Pts',(29.4633399849439,-0.911379127216999,
0.444110884113391));
#16608=CARTESIAN_POINT('Ctrl Pts',(29.4543410303956,-0.847217927666079,
0.555636629667153));
#16609=CARTESIAN_POINT('Ctrl Pts',(29.4374952526998,-0.693921902387677,
0.736013762237563));
#16610=CARTESIAN_POINT('Ctrl Pts',(29.4281298191965,-0.594508302867161,
0.8262830850724));
#16611=CARTESIAN_POINT('Ctrl Pts',(29.4079318156156,-0.341677793262293,
0.954510297187121));
#16612=CARTESIAN_POINT('Ctrl Pts',(29.3986989741889,-0.214494381189009,
0.990633906486512));
#16613=CARTESIAN_POINT('Ctrl Pts',(29.3799881069202,0.0472837866910012,
1.01362569808423));
#16614=CARTESIAN_POINT('Ctrl Pts',(29.3707427007773,0.178646956831211,0.998775584332013));
#16615=CARTESIAN_POINT('Ctrl Pts',(29.3524577090853,0.42317016203226,0.920186008439517));
#16616=CARTESIAN_POINT('Ctrl Pts',(29.3436316170096,0.534424048498588,0.860636605924485));
#16617=CARTESIAN_POINT('Ctrl Pts',(29.3246540986636,0.742262305424851,0.694100403693534));
#16618=CARTESIAN_POINT('Ctrl Pts',(29.3158947475415,0.818004230287513,0.59447223902697));
#16619=CARTESIAN_POINT('Ctrl Pts',(29.3083604951404,0.8707720276777,0.502742051616109));
#16620=CARTESIAN_POINT('',(29.4766265292794,0.871221485734819,0.502999959546298));
#16621=CARTESIAN_POINT('',(29.47662653432,0.8712215562072,0.503));
#16622=CARTESIAN_POINT('Ctrl Pts',(30.9766395048596,-0.870772027677664,
0.502742051616115));
#16623=CARTESIAN_POINT('Ctrl Pts',(30.9691052524585,-0.818004230287503,
0.594472239026902));
#16624=CARTESIAN_POINT('Ctrl Pts',(30.9603459013364,-0.742262305424921,
0.694100403693345));
#16625=CARTESIAN_POINT('Ctrl Pts',(30.9413683829904,-0.534424048498782,
0.860636605924357));
#16626=CARTESIAN_POINT('Ctrl Pts',(30.9325422909147,-0.423170162032304,
0.920186008439501));
#16627=CARTESIAN_POINT('Ctrl Pts',(30.9142572992227,-0.178646956831084,
0.998775584332033));
#16628=CARTESIAN_POINT('Ctrl Pts',(30.9050118930798,-0.0472837866908874,
1.01362569808423));
#16629=CARTESIAN_POINT('Ctrl Pts',(30.8863010258111,0.214494381189104,0.990633906486492));
#16630=CARTESIAN_POINT('Ctrl Pts',(30.8770681843844,0.341677793262382,0.954510297187089));
#16631=CARTESIAN_POINT('Ctrl Pts',(30.8568701808035,0.594508302867236,0.826283085072347));
#16632=CARTESIAN_POINT('Ctrl Pts',(30.8475047473002,0.693921902387745,0.7360137622375));
#16633=CARTESIAN_POINT('Ctrl Pts',(30.8306589696044,0.847217927666129,0.555636629667076));
#16634=CARTESIAN_POINT('Ctrl Pts',(30.8216600150561,0.911379127217037,0.444110884113312));
#16635=CARTESIAN_POINT('Ctrl Pts',(30.8025520369027,0.998002528379825,0.190430974375358));
#16636=CARTESIAN_POINT('Ctrl Pts',(30.793047838011,1.01157017614526,0.0548890692946727));
#16637=CARTESIAN_POINT('Ctrl Pts',(30.7764607849825,0.995521631670864,-0.17764597144361));
#16638=CARTESIAN_POINT('Ctrl Pts',(30.7672741424587,0.970098454855212,-0.306791753619219));
#16639=CARTESIAN_POINT('Ctrl Pts',(30.7471250024668,0.845240586957565,-0.560500408959257));
#16640=CARTESIAN_POINT('Ctrl Pts',(30.7377136687341,0.763151979773352,-0.667500700456611));
#16641=CARTESIAN_POINT('Ctrl Pts',(30.7188206192439,0.564358031936684,-0.84327568231788));
#16642=CARTESIAN_POINT('Ctrl Pts',(30.7095672963117,0.449835071540419,-0.909552155701688));
#16643=CARTESIAN_POINT('Ctrl Pts',(30.690863687752,0.200891944607386,-0.993435412233469));
#16644=CARTESIAN_POINT('Ctrl Pts',(30.6816445339917,0.0701110249796861,
-1.01138590544987));
#16645=CARTESIAN_POINT('Ctrl Pts',(30.6614385161677,-0.213025964557793,
-0.995444387176709));
#16646=CARTESIAN_POINT('Ctrl Pts',(30.6520598052671,-0.34046753425376,-0.952477692807918));
#16647=CARTESIAN_POINT('Ctrl Pts',(30.6352540053897,-0.552782663940063,
-0.849064872504943));
#16648=CARTESIAN_POINT('Ctrl Pts',(30.6262699511131,-0.656165051344254,
-0.772850244059713));
#16649=CARTESIAN_POINT('Ctrl Pts',(30.6077447657717,-0.831881844612995,
-0.581371288177443));
#16650=CARTESIAN_POINT('Ctrl Pts',(30.5982393193793,-0.901486061152773,
-0.46433518258532));
#16651=CARTESIAN_POINT('Ctrl Pts',(30.5810552458603,-0.983138694974879,
-0.237085248117399));
#16652=CARTESIAN_POINT('Ctrl Pts',(30.5718646719207,-1.01164457155601,-0.108534779049151));
#16653=CARTESIAN_POINT('Ctrl Pts',(30.5517249713866,-0.999147204660936,
0.173834987272831));
#16654=CARTESIAN_POINT('Ctrl Pts',(30.542321718213,-0.967009114614643,0.304690319176143));
#16655=CARTESIAN_POINT('Ctrl Pts',(30.5234223525951,-0.855581407083066,
0.545608350968346));
#16656=CARTESIAN_POINT('Ctrl Pts',(30.5141578837074,-0.777163779775299,
0.652387656279837));
#16657=CARTESIAN_POINT('Ctrl Pts',(30.4954668431445,-0.582980235794573,
0.829064401206585));
#16658=CARTESIAN_POINT('Ctrl Pts',(30.4862599642795,-0.470601448908801,
0.897970498795622));
#16659=CARTESIAN_POINT('Ctrl Pts',(30.4660429991873,-0.204799025246621,
0.997222455929394));
#16660=CARTESIAN_POINT('Ctrl Pts',(30.4566507719092,-0.0706111542944245,
1.0089765786811));
#16661=CARTESIAN_POINT('Ctrl Pts',(30.4398838938875,0.164820890836542,0.999641820194012));
#16662=CARTESIAN_POINT('Ctrl Pts',(30.4309137064796,0.289920670515305,0.971492512618054));
#16663=CARTESIAN_POINT('Ctrl Pts',(30.4124152715538,0.527466569099329,0.867007573502016));
#16664=CARTESIAN_POINT('Ctrl Pts',(30.4029118555964,0.63830483856681,0.787948218222788));
#16665=CARTESIAN_POINT('Ctrl Pts',(30.3856873106528,0.804917354004856,0.612382577780553));
#16666=CARTESIAN_POINT('Ctrl Pts',(30.3764931007021,0.882667521494565,0.506058560714863));
#16667=CARTESIAN_POINT('Ctrl Pts',(30.3563616071713,0.984682436642579,0.242576766412225));
#16668=CARTESIAN_POINT('Ctrl Pts',(30.346965929091,1.00788845481734,0.109958040776825));
#16669=CARTESIAN_POINT('Ctrl Pts',(30.3280621443434,1.00280273292441,-0.155484472839195));
#16670=CARTESIAN_POINT('Ctrl Pts',(30.3187862830509,0.973839811222994,-0.284930092981143));
#16671=CARTESIAN_POINT('Ctrl Pts',(30.300107804091,0.86714400606165,-0.524617833052891));
#16672=CARTESIAN_POINT('Ctrl Pts',(30.2909121905272,0.792089695015476,-0.632780197940582));
#16673=CARTESIAN_POINT('Ctrl Pts',(30.2706842229679,0.588587875794973,-0.830697511597097));
#16674=CARTESIAN_POINT('Ctrl Pts',(30.2612794374791,0.470235006290619,-0.895430023340954));
#16675=CARTESIAN_POINT('Ctrl Pts',(30.2445489336977,0.251421288995111,-0.981433054835686));
#16676=CARTESIAN_POINT('Ctrl Pts',(30.2355913796315,0.12576520800403,-1.00599999999997));
#16677=CARTESIAN_POINT('Ctrl Pts',(30.2176616890085,-0.12576520800412,-1.00599999999996));
#16678=CARTESIAN_POINT('Ctrl Pts',(30.2087041349353,-0.251421288995197,
-0.981433054835669));
#16679=CARTESIAN_POINT('Ctrl Pts',(30.191973631154,-0.470235006290692,-0.895430023340922));
#16680=CARTESIAN_POINT('Ctrl Pts',(30.1825688456652,-0.588587875795032,
-0.830697511597059));
#16681=CARTESIAN_POINT('Ctrl Pts',(30.1623408781059,-0.792089695015518,
-0.632780197940532));
#16682=CARTESIAN_POINT('Ctrl Pts',(30.1531452645421,-0.867144006061684,
-0.524617833052833));
#16683=CARTESIAN_POINT('Ctrl Pts',(30.1344667855823,-0.973839811223013,
-0.284930092981069));
#16684=CARTESIAN_POINT('Ctrl Pts',(30.1251909242898,-1.00280273292442,-0.155484472839113));
#16685=CARTESIAN_POINT('Ctrl Pts',(30.1062871395422,-1.00788845481734,0.109958040776927));
#16686=CARTESIAN_POINT('Ctrl Pts',(30.0968914614619,-0.984682436642562,
0.242576766412345));
#16687=CARTESIAN_POINT('Ctrl Pts',(30.0767599679312,-0.882667521494528,
0.506058560714953));
#16688=CARTESIAN_POINT('Ctrl Pts',(30.0675657579804,-0.804917354004824,
0.61238257778061));
#16689=CARTESIAN_POINT('Ctrl Pts',(30.0503412130368,-0.63830483856678,0.787948218222807));
#16690=CARTESIAN_POINT('Ctrl Pts',(30.0408377970794,-0.527466569099297,
0.867007573502019));
#16691=CARTESIAN_POINT('Ctrl Pts',(30.0223393621535,-0.289920670515251,
0.971492512618062));
#16692=CARTESIAN_POINT('Ctrl Pts',(30.0133691747455,-0.164820890836456,
0.999641820194026));
#16693=CARTESIAN_POINT('Ctrl Pts',(29.9966022967237,0.0706111542945367,
1.00897657868109));
#16694=CARTESIAN_POINT('Ctrl Pts',(29.9872100694456,0.204799025246713,0.997222455929378));
#16695=CARTESIAN_POINT('Ctrl Pts',(29.9669931043534,0.470601448908866,0.89797049879559));
#16696=CARTESIAN_POINT('Ctrl Pts',(29.9577862254885,0.582980235794632,0.829064401206544));
#16697=CARTESIAN_POINT('Ctrl Pts',(29.9390951849257,0.777163779775341,0.652387656279782));
#16698=CARTESIAN_POINT('Ctrl Pts',(29.9298307160381,0.855581407083098,0.545608350968287));
#16699=CARTESIAN_POINT('Ctrl Pts',(29.9109313504203,0.967009114614655,0.304690319176081));
#16700=CARTESIAN_POINT('Ctrl Pts',(29.9015280972469,0.999147204660938,0.173834987272769));
#16701=CARTESIAN_POINT('Ctrl Pts',(29.8813883967129,1.01164457155599,-0.10853477904918));
#16702=CARTESIAN_POINT('Ctrl Pts',(29.8721978227732,0.983138694974849,-0.2370852481174));
#16703=CARTESIAN_POINT('Ctrl Pts',(29.8550137492541,0.901486061152735,-0.464335182585305));
#16704=CARTESIAN_POINT('Ctrl Pts',(29.8455083028615,0.831881844612943,-0.581371288177433));
#16705=CARTESIAN_POINT('Ctrl Pts',(29.82698311752,0.656165051344171,-0.772850244059737));
#16706=CARTESIAN_POINT('Ctrl Pts',(29.8179990632434,0.552782663939949,-0.849064872504989));
#16707=CARTESIAN_POINT('Ctrl Pts',(29.801193263366,0.340467534253614,-0.952477692807958));
#16708=CARTESIAN_POINT('Ctrl Pts',(29.7918145524654,0.21302596455767,-0.995444387176729));
#16709=CARTESIAN_POINT('Ctrl Pts',(29.7716085346413,-0.0701110249797728,
-1.01138590544987));
#16710=CARTESIAN_POINT('Ctrl Pts',(29.7623893808811,-0.200891944607462,
-0.993435412233453));
#16711=CARTESIAN_POINT('Ctrl Pts',(29.7436857723215,-0.44983507154048,-0.909552155701658));
#16712=CARTESIAN_POINT('Ctrl Pts',(29.7344324493892,-0.56435803193674,-0.843275682317841));
#16713=CARTESIAN_POINT('Ctrl Pts',(29.7155393998991,-0.763151979773394,
-0.667500700456562));
#16714=CARTESIAN_POINT('Ctrl Pts',(29.7061280661665,-0.845240586957599,
-0.560500408959205));
#16715=CARTESIAN_POINT('Ctrl Pts',(29.6859789261746,-0.97009845485523,-0.306791753619162));
#16716=CARTESIAN_POINT('Ctrl Pts',(29.6767922836507,-0.995521631670873,
-0.177645971443554));
#16717=CARTESIAN_POINT('Ctrl Pts',(29.6602052306221,-1.01157017614525,0.0548890692946818));
#16718=CARTESIAN_POINT('Ctrl Pts',(29.6507010317302,-0.99800252837983,0.190430974375375));
#16719=CARTESIAN_POINT('Ctrl Pts',(29.6315930535767,-0.911379127217004,
0.444110884113379));
#16720=CARTESIAN_POINT('Ctrl Pts',(29.6225940990285,-0.847217927666085,
0.555636629667144));
#16721=CARTESIAN_POINT('Ctrl Pts',(29.6057483213328,-0.693921902387682,
0.73601376223756));
#16722=CARTESIAN_POINT('Ctrl Pts',(29.5963828878296,-0.594508302867167,
0.826283085072396));
#16723=CARTESIAN_POINT('Ctrl Pts',(29.5761848842486,-0.341677793262302,
0.954510297187118));
#16724=CARTESIAN_POINT('Ctrl Pts',(29.5669520428219,-0.214494381189018,
0.99063390648651));
#16725=CARTESIAN_POINT('Ctrl Pts',(29.5482411755531,0.0472837866909914,
1.01362569808423));
#16726=CARTESIAN_POINT('Ctrl Pts',(29.5389957694103,0.178646956831203,0.998775584332015));
#16727=CARTESIAN_POINT('Ctrl Pts',(29.5207107777183,0.423170162032483,0.920186008439446));
#16728=CARTESIAN_POINT('Ctrl Pts',(29.5118846856427,0.534424048499014,0.860636605924257));
#16729=CARTESIAN_POINT('Ctrl Pts',(29.4929071645997,0.742262334961756,0.694100380026134));
#16730=CARTESIAN_POINT('Ctrl Pts',(29.4841478114739,0.818004270752247,0.594472186190298));
#16731=CARTESIAN_POINT('Ctrl Pts',(29.4766135577663,0.870772069751002,0.502741978476952));
#16732=CARTESIAN_POINT('Ctrl Pts',(31.16948943148,-1.281030538212,0.1346417350707));
#16733=CARTESIAN_POINT('Ctrl Pts',(31.15323943148,-1.250481297573,0.4252983443058));
#16734=CARTESIAN_POINT('Ctrl Pts',(31.12073943148,-0.9839217726285,0.9837339190898));
#16735=CARTESIAN_POINT('Ctrl Pts',(31.07198943148,-0.1454413688885,1.383873286175));
#16736=CARTESIAN_POINT('Ctrl Pts',(31.02323943148,0.7578368377583,1.166956165481));
#16737=CARTESIAN_POINT('Ctrl Pts',(30.97448943148,1.323348169458,0.429985043746));
#16738=CARTESIAN_POINT('Ctrl Pts',(30.92573943148,1.299030624161,-0.4986520486237));
#16739=CARTESIAN_POINT('Ctrl Pts',(30.87698943148,0.6957251488278,-1.205031028341));
#16740=CARTESIAN_POINT('Ctrl Pts',(30.82823943148,-0.2176707818353,-1.374319249677));
#16741=CARTESIAN_POINT('Ctrl Pts',(30.77948943148,-1.034049050162,-0.9310619315066));
#16742=CARTESIAN_POINT('Ctrl Pts',(30.73073943148,-1.38954331457,-0.07282288382614));
#16743=CARTESIAN_POINT('Ctrl Pts',(30.68198943148,-1.125706897575,0.8178739364602));
#16744=CARTESIAN_POINT('Ctrl Pts',(30.63323943148,-0.360133824607,1.344037730506));
#16745=CARTESIAN_POINT('Ctrl Pts',(30.58448943148,0.56595380301,1.271153053958));
#16746=CARTESIAN_POINT('Ctrl Pts',(30.53573943148,1.239791249317,0.6317051935655));
#16747=CARTESIAN_POINT('Ctrl Pts',(30.48698943148,1.361043721917,-0.2892987738068));
#16748=CARTESIAN_POINT('Ctrl Pts',(30.43823943148,0.8756680143869,-1.081359941037));
#16749=CARTESIAN_POINT('Ctrl Pts',(30.38948943148,-2.281508315605E-14,-1.3914502483));
#16750=CARTESIAN_POINT('Ctrl Pts',(30.34073943148,-0.8756680143869,-1.081359941037));
#16751=CARTESIAN_POINT('Ctrl Pts',(30.29198943148,-1.361043721917,-0.2892987738067));
#16752=CARTESIAN_POINT('Ctrl Pts',(30.24323943148,-1.239791249317,0.6317051935656));
#16753=CARTESIAN_POINT('Ctrl Pts',(30.19448943148,-0.56595380301,1.271153053958));
#16754=CARTESIAN_POINT('Ctrl Pts',(30.14573943148,0.360133824607,1.344037730506));
#16755=CARTESIAN_POINT('Ctrl Pts',(30.09698943148,1.125706897575,0.8178739364602));
#16756=CARTESIAN_POINT('Ctrl Pts',(30.04823943148,1.38954331457,-0.07282288382618));
#16757=CARTESIAN_POINT('Ctrl Pts',(29.99948943148,1.034049050162,-0.9310619315066));
#16758=CARTESIAN_POINT('Ctrl Pts',(29.95073943148,0.2176707818353,-1.374319249677));
#16759=CARTESIAN_POINT('Ctrl Pts',(29.90198943148,-0.6957251488278,-1.205031028341));
#16760=CARTESIAN_POINT('Ctrl Pts',(29.85323943148,-1.299030624161,-0.4986520486236));
#16761=CARTESIAN_POINT('Ctrl Pts',(29.80448943148,-1.323348169458,0.4299850437461));
#16762=CARTESIAN_POINT('Ctrl Pts',(29.75573943148,-0.7578368377582,1.166956165481));
#16763=CARTESIAN_POINT('Ctrl Pts',(29.70698943148,0.1454413688886,1.383873286175));
#16764=CARTESIAN_POINT('Ctrl Pts',(29.65823943148,0.9839217726285,0.9837339190898));
#16765=CARTESIAN_POINT('Ctrl Pts',(29.62573943148,1.250481297573,0.4252983443058));
#16766=CARTESIAN_POINT('Ctrl Pts',(29.60948943148,1.281030538212,0.1346417350707));
#16767=CARTESIAN_POINT('Ctrl Pts',(31.1078719886,-1.174890644721,0.1234859827342));
#16768=CARTESIAN_POINT('Ctrl Pts',(31.0916219886,-1.146872563997,0.3900602140506));
#16769=CARTESIAN_POINT('Ctrl Pts',(31.0591219886,-0.9023988510157,0.9022265620979));
#16770=CARTESIAN_POINT('Ctrl Pts',(31.0103719886,-0.1333908119794,1.269212348111));
#16771=CARTESIAN_POINT('Ctrl Pts',(30.9616219886,0.6950462025284,1.070267913782));
#16772=CARTESIAN_POINT('Ctrl Pts',(30.9128719886,1.213702045055,0.3943585966126));
#16773=CARTESIAN_POINT('Ctrl Pts',(30.8641219886,1.191399332028,-0.4573361909988));
#16774=CARTESIAN_POINT('Ctrl Pts',(30.8153719886,0.6380807828327,-1.105188080663));
#16775=CARTESIAN_POINT('Ctrl Pts',(30.7666219886,-0.1996356508131,-1.260449912114));
#16776=CARTESIAN_POINT('Ctrl Pts',(30.7178719886,-0.9483728287337,-0.8539187164967));
#16777=CARTESIAN_POINT('Ctrl Pts',(30.6691219886,-1.274412585824,-0.06678913763317));
#16778=CARTESIAN_POINT('Ctrl Pts',(30.6203719886,-1.032436357454,0.7501089223443));
#16779=CARTESIAN_POINT('Ctrl Pts',(30.5716219886,-0.3302949061378,1.232677370773));
#16780=CARTESIAN_POINT('Ctrl Pts',(30.5228719886,0.5190616528384,1.165831560259));
#16781=CARTESIAN_POINT('Ctrl Pts',(30.4741219886,1.137068240592,0.5793652063734));
#16782=CARTESIAN_POINT('Ctrl Pts',(30.4253719886,1.248274329329,-0.2653288994572));
#16783=CARTESIAN_POINT('Ctrl Pts',(30.3766219886,0.8031144670607,-0.9917637717473));
#16784=CARTESIAN_POINT('Ctrl Pts',(30.3278719886,-2.057218704603E-14,-1.276161520399));
#16785=CARTESIAN_POINT('Ctrl Pts',(30.2791219886,-0.8031144670608,-0.9917637717473));
#16786=CARTESIAN_POINT('Ctrl Pts',(30.2303719886,-1.248274329329,-0.2653288994572));
#16787=CARTESIAN_POINT('Ctrl Pts',(30.1816219886,-1.137068240592,0.5793652063734));
#16788=CARTESIAN_POINT('Ctrl Pts',(30.1328719886,-0.5190616528384,1.165831560259));
#16789=CARTESIAN_POINT('Ctrl Pts',(30.0841219886,0.3302949061378,1.232677370773));
#16790=CARTESIAN_POINT('Ctrl Pts',(30.0353719886,1.032436357454,0.7501089223443));
#16791=CARTESIAN_POINT('Ctrl Pts',(29.9866219886,1.274412585824,-0.06678913763321));
#16792=CARTESIAN_POINT('Ctrl Pts',(29.9378719886,0.9483728287337,-0.8539187164967));
#16793=CARTESIAN_POINT('Ctrl Pts',(29.8891219886,0.1996356508131,-1.260449912114));
#16794=CARTESIAN_POINT('Ctrl Pts',(29.8403719886,-0.6380807828327,-1.105188080663));
#16795=CARTESIAN_POINT('Ctrl Pts',(29.7916219886,-1.191399332028,-0.4573361909987));
#16796=CARTESIAN_POINT('Ctrl Pts',(29.7428719886,-1.213702045055,0.3943585966126));
#16797=CARTESIAN_POINT('Ctrl Pts',(29.6941219886,-0.6950462025284,1.070267913782));
#16798=CARTESIAN_POINT('Ctrl Pts',(29.6453719886,0.1333908119795,1.269212348111));
#16799=CARTESIAN_POINT('Ctrl Pts',(29.5966219886,0.9023988510157,0.9022265620978));
#16800=CARTESIAN_POINT('Ctrl Pts',(29.5641219886,1.146872563997,0.3900602140505));
#16801=CARTESIAN_POINT('Ctrl Pts',(29.5478719886,1.174890644721,0.1234859827342));
#16802=CARTESIAN_POINT('Ctrl Pts',(31.04625454572,-1.06875075123,0.1123302303977));
#16803=CARTESIAN_POINT('Ctrl Pts',(31.03000454572,-1.04326383042,0.3548220837953));
#16804=CARTESIAN_POINT('Ctrl Pts',(30.99750454572,-0.820875929403,0.8207192051059));
#16805=CARTESIAN_POINT('Ctrl Pts',(30.94875454572,-0.1213402550703,1.154551410048));
#16806=CARTESIAN_POINT('Ctrl Pts',(30.90000454572,0.6322555672986,0.9735796620828));
#16807=CARTESIAN_POINT('Ctrl Pts',(30.85125454572,1.104055920651,0.3587321494792));
#16808=CARTESIAN_POINT('Ctrl Pts',(30.80250454572,1.083768039895,-0.4160203333738));
#16809=CARTESIAN_POINT('Ctrl Pts',(30.75375454572,0.5804364168376,-1.005345132984));
#16810=CARTESIAN_POINT('Ctrl Pts',(30.70500454572,-0.1816005197909,-1.146580574552));
#16811=CARTESIAN_POINT('Ctrl Pts',(30.65625454572,-0.8626966073051,-0.7767755014867));
#16812=CARTESIAN_POINT('Ctrl Pts',(30.60750454572,-1.159281857079,-0.06075539144021));
#16813=CARTESIAN_POINT('Ctrl Pts',(30.55875454572,-0.9391658173332,0.6823439082283));
#16814=CARTESIAN_POINT('Ctrl Pts',(30.51000454572,-0.3004559876685,1.121317011041));
#16815=CARTESIAN_POINT('Ctrl Pts',(30.46125454572,0.4721695026668,1.060510066561));
#16816=CARTESIAN_POINT('Ctrl Pts',(30.41250454572,1.034345231867,0.5270252191813));
#16817=CARTESIAN_POINT('Ctrl Pts',(30.36375454572,1.135504936741,-0.2413590251076));
#16818=CARTESIAN_POINT('Ctrl Pts',(30.31500454572,0.7305609197345,-0.9021676024575));
#16819=CARTESIAN_POINT('Ctrl Pts',(30.26625454572,-1.95289898311E-14,-1.160872792498));
#16820=CARTESIAN_POINT('Ctrl Pts',(30.21750454572,-0.7305609197346,-0.9021676024575));
#16821=CARTESIAN_POINT('Ctrl Pts',(30.16875454572,-1.135504936741,-0.2413590251076));
#16822=CARTESIAN_POINT('Ctrl Pts',(30.12000454572,-1.034345231867,0.5270252191813));
#16823=CARTESIAN_POINT('Ctrl Pts',(30.07125454572,-0.4721695026667,1.060510066561));
#16824=CARTESIAN_POINT('Ctrl Pts',(30.02250454572,0.3004559876686,1.121317011041));
#16825=CARTESIAN_POINT('Ctrl Pts',(29.97375454572,0.9391658173332,0.6823439082283));
#16826=CARTESIAN_POINT('Ctrl Pts',(29.92500454572,1.159281857079,-0.06075539144025));
#16827=CARTESIAN_POINT('Ctrl Pts',(29.87625454572,0.8626966073051,-0.7767755014868));
#16828=CARTESIAN_POINT('Ctrl Pts',(29.82750454572,0.1816005197909,-1.146580574552));
#16829=CARTESIAN_POINT('Ctrl Pts',(29.77875454572,-0.5804364168377,-1.005345132984));
#16830=CARTESIAN_POINT('Ctrl Pts',(29.73000454572,-1.083768039895,-0.4160203333738));
#16831=CARTESIAN_POINT('Ctrl Pts',(29.68125454572,-1.104055920651,0.3587321494792));
#16832=CARTESIAN_POINT('Ctrl Pts',(29.63250454572,-0.6322555672985,0.9735796620828));
#16833=CARTESIAN_POINT('Ctrl Pts',(29.58375454572,0.1213402550704,1.154551410048));
#16834=CARTESIAN_POINT('Ctrl Pts',(29.53500454572,0.820875929403,0.8207192051059));
#16835=CARTESIAN_POINT('Ctrl Pts',(29.50250454572,1.04326383042,0.3548220837952));
#16836=CARTESIAN_POINT('Ctrl Pts',(29.48625454572,1.06875075123,0.1123302303976));
#16837=CARTESIAN_POINT('Ctrl Pts',(30.98463710284,-0.962610857739,0.1011744780611));
#16838=CARTESIAN_POINT('Ctrl Pts',(30.96838710284,-0.939655096844,0.31958395354));
#16839=CARTESIAN_POINT('Ctrl Pts',(30.93588710284,-0.7393530077902,0.739211848114));
#16840=CARTESIAN_POINT('Ctrl Pts',(30.88713710284,-0.1092896981613,1.039890471984));
#16841=CARTESIAN_POINT('Ctrl Pts',(30.83838710284,0.5694649320687,0.8768914103838));
#16842=CARTESIAN_POINT('Ctrl Pts',(30.78963710284,0.9944097962472,0.3231057023458));
#16843=CARTESIAN_POINT('Ctrl Pts',(30.74088710284,0.9761367477614,-0.3747044757489));
#16844=CARTESIAN_POINT('Ctrl Pts',(30.69213710284,0.5227920508426,-0.9055021853055));
#16845=CARTESIAN_POINT('Ctrl Pts',(30.64338710284,-0.1635653887687,-1.03271123699));
#16846=CARTESIAN_POINT('Ctrl Pts',(30.59463710284,-0.7770203858765,-0.6996322864768));
#16847=CARTESIAN_POINT('Ctrl Pts',(30.54588710284,-1.044151128333,-0.05472164524724));
#16848=CARTESIAN_POINT('Ctrl Pts',(30.49713710284,-0.8458952772121,0.6145788941124));
#16849=CARTESIAN_POINT('Ctrl Pts',(30.44838710284,-0.2706170691993,1.009956651308));
#16850=CARTESIAN_POINT('Ctrl Pts',(30.39963710284,0.4252773524951,0.9551885728626));
#16851=CARTESIAN_POINT('Ctrl Pts',(30.35088710284,0.9316222231427,0.4746852319892));
#16852=CARTESIAN_POINT('Ctrl Pts',(30.30213710284,1.022735544153,-0.2173891507581));
#16853=CARTESIAN_POINT('Ctrl Pts',(30.25338710284,0.6580073724084,-0.8125714331677));
#16854=CARTESIAN_POINT('Ctrl Pts',(30.20463710284,-1.731947918415E-14,-1.045584064598));
#16855=CARTESIAN_POINT('Ctrl Pts',(30.15588710284,-0.6580073724084,-0.8125714331677));
#16856=CARTESIAN_POINT('Ctrl Pts',(30.10713710284,-1.022735544153,-0.217389150758));
#16857=CARTESIAN_POINT('Ctrl Pts',(30.05838710284,-0.9316222231426,0.4746852319892));
#16858=CARTESIAN_POINT('Ctrl Pts',(30.00963710284,-0.4252773524951,0.9551885728626));
#16859=CARTESIAN_POINT('Ctrl Pts',(29.96088710284,0.2706170691994,1.009956651308));
#16860=CARTESIAN_POINT('Ctrl Pts',(29.91213710284,0.8458952772121,0.6145788941123));
#16861=CARTESIAN_POINT('Ctrl Pts',(29.86338710284,1.044151128333,-0.05472164524727));
#16862=CARTESIAN_POINT('Ctrl Pts',(29.81463710284,0.7770203858765,-0.6996322864768));
#16863=CARTESIAN_POINT('Ctrl Pts',(29.76588710284,0.1635653887687,-1.03271123699));
#16864=CARTESIAN_POINT('Ctrl Pts',(29.71713710284,-0.5227920508426,-0.9055021853054));
#16865=CARTESIAN_POINT('Ctrl Pts',(29.66838710284,-0.9761367477614,-0.3747044757489));
#16866=CARTESIAN_POINT('Ctrl Pts',(29.61963710284,-0.9944097962471,0.3231057023458));
#16867=CARTESIAN_POINT('Ctrl Pts',(29.57088710284,-0.5694649320687,0.8768914103838));
#16868=CARTESIAN_POINT('Ctrl Pts',(29.52213710284,0.1092896981613,1.039890471984));
#16869=CARTESIAN_POINT('Ctrl Pts',(29.47338710284,0.7393530077902,0.739211848114));
#16870=CARTESIAN_POINT('Ctrl Pts',(29.44088710284,0.939655096844,0.31958395354));
#16871=CARTESIAN_POINT('Ctrl Pts',(29.42463710284,0.962610857739,0.1011744780611));
#16872=CARTESIAN_POINT('',(29.6173426729392,1.08229570994162,0.624863717666542));
#16873=CARTESIAN_POINT('Ctrl Pts',(29.6176143539202,1.08217404411672,0.62477577113726));
#16874=CARTESIAN_POINT('Ctrl Pts',(29.624006078429,1.02692313633376,0.72095524840202));
#16875=CARTESIAN_POINT('Ctrl Pts',(29.6300982973051,0.959567950505402,0.80866689162659));
#16876=CARTESIAN_POINT('Ctrl Pts',(29.642405213234,0.805177359442618,0.961582228722831));
#16877=CARTESIAN_POINT('Ctrl Pts',(29.6486181844899,0.719600014745411,1.02676062670149));
#16878=CARTESIAN_POINT('Ctrl Pts',(29.6603920217373,0.544736432615982,1.12829523582901));
#16879=CARTESIAN_POINT('Ctrl Pts',(29.6659562556449,0.456650520588996,1.16701073503247));
#16880=CARTESIAN_POINT('Ctrl Pts',(29.677217232469,0.26753464102805,1.22524604638644));
#16881=CARTESIAN_POINT('Ctrl Pts',(29.6828002272489,0.166994080218219,1.24292681195758));
#16882=CARTESIAN_POINT('Ctrl Pts',(29.6933799224966,-0.0180241963746623,
1.25212919749128));
#16883=CARTESIAN_POINT('Ctrl Pts',(29.6982004972975,-0.101216694303839,
1.24795972121552));
#16884=CARTESIAN_POINT('Ctrl Pts',(29.7086891642604,-0.27942575559589,1.22150982604158));
#16885=CARTESIAN_POINT('Ctrl Pts',(29.7143622631559,-0.374099964090084,
1.19618207008826));
#16886=CARTESIAN_POINT('Ctrl Pts',(29.7258599403583,-0.56156923419032,1.1215657071463));
#16887=CARTESIAN_POINT('Ctrl Pts',(29.7315605712698,-0.652719320880998,
1.07105375242234));
#16888=CARTESIAN_POINT('Ctrl Pts',(29.7422685234012,-0.80378203686466,0.960235111854163));
#16889=CARTESIAN_POINT('Ctrl Pts',(29.7470893694736,-0.865691388100042,
0.904541514672143));
#16890=CARTESIAN_POINT('Ctrl Pts',(29.7575548795348,-0.987031922779028,
0.771912092007434));
#16891=CARTESIAN_POINT('Ctrl Pts',(29.7632039529513,-1.04433572334087,0.692883434585601));
#16892=CARTESIAN_POINT('Ctrl Pts',(29.7746485393149,-1.14248867363917,0.51757590484434));
#16893=CARTESIAN_POINT('Ctrl Pts',(29.7803228612616,-1.18132573215868,0.421387032124818));
#16894=CARTESIAN_POINT('Ctrl Pts',(29.7910025371398,-1.22890273220619,0.240666505206899));
#16895=CARTESIAN_POINT('Ctrl Pts',(29.7958233857595,-1.24198371349995,0.15842366891221));
#16896=CARTESIAN_POINT('Ctrl Pts',(29.8062905593356,-1.25285449382397,-0.0210353298026874));
#16897=CARTESIAN_POINT('Ctrl Pts',(29.8119413766803,-1.24766895484646,-0.118540271041648));
#16898=CARTESIAN_POINT('Ctrl Pts',(29.8233905058994,-1.21364125427389,-0.316621766311773));
#16899=CARTESIAN_POINT('Ctrl Pts',(29.8290672187053,-1.1832866023825,-0.415860313469128));
#16900=CARTESIAN_POINT('Ctrl Pts',(29.8397493384842,-1.10651941709313,-0.586291237802933));
#16901=CARTESIAN_POINT('Ctrl Pts',(29.8445701692025,-1.06493107988469,-0.65844035127944));
#16902=CARTESIAN_POINT('Ctrl Pts',(29.8550382895607,-0.960438444020922,
-0.804765872180896));
#16903=CARTESIAN_POINT('Ctrl Pts',(29.8606900786369,-0.895037104296968,
-0.877292185999977));
#16904=CARTESIAN_POINT('Ctrl Pts',(29.8721410937214,-0.743911877053629,
-1.00983818692771));
#16905=CARTESIAN_POINT('Ctrl Pts',(29.8778186927784,-0.657854911540548,
-1.0678657110005));
#16906=CARTESIAN_POINT('Ctrl Pts',(29.8885018175822,-0.490923110762975,
-1.15200547510011));
#16907=CARTESIAN_POINT('Ctrl Pts',(29.8933226556308,-0.413197385639256,
-1.18190074127503));
#16908=CARTESIAN_POINT('Ctrl Pts',(29.9037902621361,-0.239912892682437,
-1.22984962205128));
#16909=CARTESIAN_POINT('Ctrl Pts',(29.9094415211202,-0.143452590634435,
-1.24505123570626));
#16910=CARTESIAN_POINT('Ctrl Pts',(29.9208913119615,0.0573873184303584,
-1.2529493814113));
#16911=CARTESIAN_POINT('Ctrl Pts',(29.9265682655615,0.160772387954986,-1.2438890857129));
#16912=CARTESIAN_POINT('Ctrl Pts',(29.9372506771216,0.343442956077328,-1.20422974934481));
#16913=CARTESIAN_POINT('Ctrl Pts',(29.9420715140664,0.422661457005336,-1.17854950375753));
#16914=CARTESIAN_POINT('Ctrl Pts',(29.9525393204991,0.587508268981554,-1.10676239626014));
#16915=CARTESIAN_POINT('Ctrl Pts',(29.9581907845802,0.672042139416098,-1.05787108303544));
#16916=CARTESIAN_POINT('Ctrl Pts',(29.9696327050032,0.832984309871719,-0.937700574032089));
#16917=CARTESIAN_POINT('Ctrl Pts',(29.975302140758,0.907539604845622,-0.865708448776034));
#16918=CARTESIAN_POINT('Ctrl Pts',(29.9859759790889,1.02450658945619,-0.720077726497188));
#16919=CARTESIAN_POINT('Ctrl Pts',(29.9907968641008,1.06993512467627,-0.650278802855199));
#16920=CARTESIAN_POINT('Ctrl Pts',(30.0012686163419,1.15295219073745,-0.490715127389166));
#16921=CARTESIAN_POINT('Ctrl Pts',(30.0069240412507,1.18792592563569,-0.399467717681269));
#16922=CARTESIAN_POINT('Ctrl Pts',(30.0182537292321,1.23692421017922,-0.206718632695365));
#16923=CARTESIAN_POINT('Ctrl Pts',(30.0238150291331,1.2495831573343,-0.105894062156999));
#16924=CARTESIAN_POINT('Ctrl Pts',(30.0343650719903,1.24978013102473,0.0788946968053972));
#16925=CARTESIAN_POINT('Ctrl Pts',(30.03918647532,1.24155914322836,0.161818966878246));
#16926=CARTESIAN_POINT('Ctrl Pts',(30.049716193534,1.20631400859158,0.339223774572963));
#16927=CARTESIAN_POINT('Ctrl Pts',(30.0554300523819,1.17611645123081,0.433186524248501));
#16928=CARTESIAN_POINT('Ctrl Pts',(30.0675374387705,1.08773783421796,0.626353450277986));
#16929=CARTESIAN_POINT('Ctrl Pts',(30.0737661544201,1.02629079132724,0.722514395481912));
#16930=CARTESIAN_POINT('Ctrl Pts',(30.0850677301825,0.898311720065109,0.872323797899091));
#16931=CARTESIAN_POINT('Ctrl Pts',(30.0898826047594,0.838420345371865,0.929811830416312));
#16932=CARTESIAN_POINT('Ctrl Pts',(30.1001063454557,0.700551180287231,1.03858986657383));
#16933=CARTESIAN_POINT('Ctrl Pts',(30.1055166619412,0.621156618871846,1.08824415113204));
#16934=CARTESIAN_POINT('Ctrl Pts',(30.1155732472167,0.461535574094524,1.16461119456429));
#16935=CARTESIAN_POINT('Ctrl Pts',(30.1201846224814,0.382630077285512,1.19286944412205));
#16936=CARTESIAN_POINT('Ctrl Pts',(30.1303201759706,0.209221629354947,1.23560306157392));
#16937=CARTESIAN_POINT('Ctrl Pts',(30.1358277672504,0.114600498425028,1.24765599318599));
#16938=CARTESIAN_POINT('Ctrl Pts',(30.1461423243216,-0.0625593640511048,
1.2504209271504));
#16939=CARTESIAN_POINT('Ctrl Pts',(30.1509499487298,-0.145158645335778,
1.24370209826895));
#16940=CARTESIAN_POINT('Ctrl Pts',(30.1623960154908,-0.34138856704879,1.20803039925062));
#16941=CARTESIAN_POINT('Ctrl Pts',(30.1687600206973,-0.452098250127229,
1.17119579309478));
#16942=CARTESIAN_POINT('Ctrl Pts',(30.1812232769964,-0.6475609189281,1.0734199677459));
#16943=CARTESIAN_POINT('Ctrl Pts',(30.1871507413653,-0.732808811270244,
1.01681968518547));
#16944=CARTESIAN_POINT('Ctrl Pts',(30.1978846820031,-0.873249736341285,
0.897298777762955));
#16945=CARTESIAN_POINT('Ctrl Pts',(30.2026998467177,-0.931156847168942,
0.837385858829736));
#16946=CARTESIAN_POINT('Ctrl Pts',(30.2128560269344,-1.04160926343471,0.697460755129515));
#16947=CARTESIAN_POINT('Ctrl Pts',(30.2180744566332,-1.09152962316664,0.616422806085973));
#16948=CARTESIAN_POINT('Ctrl Pts',(30.2291153833449,-1.17343776603598,0.440598243640985));
#16949=CARTESIAN_POINT('Ctrl Pts',(30.2348633917994,-1.20439161560408,0.346197958887923));
#16950=CARTESIAN_POINT('Ctrl Pts',(30.2454211962973,-1.24064756275581,0.168513870520372));
#16951=CARTESIAN_POINT('Ctrl Pts',(30.2502356404206,-1.24929616484977,0.0857996286522642));
#16952=CARTESIAN_POINT('Ctrl Pts',(30.260845968283,-1.25015559790857,-0.0998540057624514));
#16953=CARTESIAN_POINT('Ctrl Pts',(30.2664618688018,-1.23783723726391,-0.201732441524374));
#16954=CARTESIAN_POINT('Ctrl Pts',(30.2779476142182,-1.18877368950535,-0.397420656303737));
#16955=CARTESIAN_POINT('Ctrl Pts',(30.2837121233972,-1.15320964302152,-0.490475139093015));
#16956=CARTESIAN_POINT('Ctrl Pts',(30.2942863118249,-1.069186562366,-0.651500670982716));
#16957=CARTESIAN_POINT('Ctrl Pts',(30.2991009718451,-1.02373608151537,-0.721167505274727));
#16958=CARTESIAN_POINT('Ctrl Pts',(30.3096647652641,-0.907811249820588,
-0.865207026839823));
#16959=CARTESIAN_POINT('Ctrl Pts',(30.3152394739193,-0.834627259119606,
-0.936040525954595));
#16960=CARTESIAN_POINT('Ctrl Pts',(30.3266764849137,-0.674053122419932,
-1.05677212531789));
#16961=CARTESIAN_POINT('Ctrl Pts',(30.3324367366807,-0.587930416894772,
-1.10669970892292));
#16962=CARTESIAN_POINT('Ctrl Pts',(30.3430067005688,-0.421391361778247,
-1.17899951718269));
#16963=CARTESIAN_POINT('Ctrl Pts',(30.3478213072528,-0.342241259312169,
-1.20456840716749));
#16964=CARTESIAN_POINT('Ctrl Pts',(30.3583968820281,-0.161331742712564,
-1.24367026121187));
#16965=CARTESIAN_POINT('Ctrl Pts',(30.3639820052499,-0.0596875303654986,
-1.25269824867541));
#16966=CARTESIAN_POINT('Ctrl Pts',(30.3754311781681,0.141292087509596,-1.24545325484622));
#16967=CARTESIAN_POINT('Ctrl Pts',(30.3811923531843,0.239656538131442,-1.23004619913465));
#16968=CARTESIAN_POINT('Ctrl Pts',(30.3917632379838,0.414592514073174,-1.18140765243432));
#16969=CARTESIAN_POINT('Ctrl Pts',(30.3965778600333,0.492192921487782,-1.15146040435034));
#16970=CARTESIAN_POINT('Ctrl Pts',(30.4071511642511,0.657352826866551,-1.06799972437164));
#16971=CARTESIAN_POINT('Ctrl Pts',(30.4127342974649,0.741992803185985,-1.01106594613429));
#16972=CARTESIAN_POINT('Ctrl Pts',(30.4241815875351,0.893598307086217,-0.878976891974612));
#16973=CARTESIAN_POINT('Ctrl Pts',(30.4299430228036,0.960348276783893,-0.805096992503565));
#16974=CARTESIAN_POINT('Ctrl Pts',(30.4405141518347,1.06569068887403,-0.657202158667046));
#16975=CARTESIAN_POINT('Ctrl Pts',(30.4453287636464,1.10715034993008,-0.585092594502051));
#16976=CARTESIAN_POINT('Ctrl Pts',(30.4559012674437,1.18297284107288,-0.416303633918732));
#16977=CARTESIAN_POINT('Ctrl Pts',(30.4614836780058,1.21291732983988,-0.318804555305318));
#16978=CARTESIAN_POINT('Ctrl Pts',(30.4729289349782,1.24760835985574,-0.12077840292281));
#16979=CARTESIAN_POINT('Ctrl Pts',(30.4786890924477,1.25299193291298,-0.0213780096235605));
#16980=CARTESIAN_POINT('Ctrl Pts',(30.4892589680672,1.24179913974343,0.159830349400949));
#16981=CARTESIAN_POINT('Ctrl Pts',(30.4940735898383,1.22864529584052,0.241961471557666));
#16982=CARTESIAN_POINT('Ctrl Pts',(30.5046456597338,1.18136362477796,0.420845888978654));
#16983=CARTESIAN_POINT('Ctrl Pts',(30.5102275079894,1.14328812854245,0.515456134887667));
#16984=CARTESIAN_POINT('Ctrl Pts',(30.5216724857142,1.04564032875421,0.691196105002304));
#16985=CARTESIAN_POINT('Ctrl Pts',(30.5274331889503,0.987267088029638,0.771848249436175));
#16986=CARTESIAN_POINT('Ctrl Pts',(30.5380037168126,0.86452950417065,0.905646658825268));
#16987=CARTESIAN_POINT('Ctrl Pts',(30.5428183824186,0.802624260369341,0.961199870112804));
#16988=CARTESIAN_POINT('Ctrl Pts',(30.5534132806734,0.653002216612035,1.07070080173363));
#16989=CARTESIAN_POINT('Ctrl Pts',(30.5590165680466,0.563515427790726,1.12041819426113));
#16990=CARTESIAN_POINT('Ctrl Pts',(30.5705013144578,0.376386750052923,1.19561757470478));
#16991=CARTESIAN_POINT('Ctrl Pts',(30.5762777298779,0.28000269287151,1.22151736339223));
#16992=CARTESIAN_POINT('Ctrl Pts',(30.5868629719407,0.100126080921217,1.24804271905387));
#16993=CARTESIAN_POINT('Ctrl Pts',(30.5916772320891,0.0170323540855195,
1.25213893207139));
#16994=CARTESIAN_POINT('Ctrl Pts',(30.6021452020552,-0.166049167240009,
1.24290134522974));
#16995=CARTESIAN_POINT('Ctrl Pts',(30.6076315893111,-0.264813429237742,
1.22568525623814));
#16996=CARTESIAN_POINT('Ctrl Pts',(30.6188947504349,-0.454317427207725,
1.16809897304761));
#16997=CARTESIAN_POINT('Ctrl Pts',(30.6245780697958,-0.544350438350243,
1.12865296595475));
#16998=CARTESIAN_POINT('Ctrl Pts',(30.6364550006192,-0.720622542665699,
1.02601904795267));
#16999=CARTESIAN_POINT('Ctrl Pts',(30.6426517477027,-0.805926829170602,
0.96092863891174));
#17000=CARTESIAN_POINT('Ctrl Pts',(30.6549281010291,-0.959862670245003,
0.808282316275064));
#17001=CARTESIAN_POINT('Ctrl Pts',(30.661007903792,-1.02704403086579,0.720744863512174));
#17002=CARTESIAN_POINT('Ctrl Pts',(30.6673856673726,-1.08217422817382,0.6247754507349));
#17003=CARTESIAN_POINT('',(29.6175,1.082531754731,0.625));
#17004=CARTESIAN_POINT('Ctrl Pts',(30.86036289716,-0.962610857739,0.1011744780611));
#17005=CARTESIAN_POINT('Ctrl Pts',(30.84411289716,-0.939655096844,0.31958395354));
#17006=CARTESIAN_POINT('Ctrl Pts',(30.81161289716,-0.7393530077902,0.739211848114));
#17007=CARTESIAN_POINT('Ctrl Pts',(30.76286289716,-0.1092896981613,1.039890471984));
#17008=CARTESIAN_POINT('Ctrl Pts',(30.71411289716,0.5694649320687,0.8768914103838));
#17009=CARTESIAN_POINT('Ctrl Pts',(30.66536289716,0.9944097962472,0.3231057023458));
#17010=CARTESIAN_POINT('Ctrl Pts',(30.61661289716,0.9761367477614,-0.3747044757489));
#17011=CARTESIAN_POINT('Ctrl Pts',(30.56786289716,0.5227920508426,-0.9055021853055));
#17012=CARTESIAN_POINT('Ctrl Pts',(30.51911289716,-0.1635653887687,-1.03271123699));
#17013=CARTESIAN_POINT('Ctrl Pts',(30.47036289716,-0.7770203858765,-0.6996322864768));
#17014=CARTESIAN_POINT('Ctrl Pts',(30.42161289716,-1.044151128333,-0.05472164524724));
#17015=CARTESIAN_POINT('Ctrl Pts',(30.37286289716,-0.8458952772121,0.6145788941124));
#17016=CARTESIAN_POINT('Ctrl Pts',(30.32411289716,-0.2706170691993,1.009956651308));
#17017=CARTESIAN_POINT('Ctrl Pts',(30.27536289716,0.4252773524951,0.9551885728626));
#17018=CARTESIAN_POINT('Ctrl Pts',(30.22661289716,0.9316222231427,0.4746852319892));
#17019=CARTESIAN_POINT('Ctrl Pts',(30.17786289716,1.022735544153,-0.2173891507581));
#17020=CARTESIAN_POINT('Ctrl Pts',(30.12911289716,0.6580073724084,-0.8125714331677));
#17021=CARTESIAN_POINT('Ctrl Pts',(30.08036289716,-1.726396803292E-14,-1.045584064598));
#17022=CARTESIAN_POINT('Ctrl Pts',(30.03161289716,-0.6580073724084,-0.8125714331677));
#17023=CARTESIAN_POINT('Ctrl Pts',(29.98286289716,-1.022735544153,-0.217389150758));
#17024=CARTESIAN_POINT('Ctrl Pts',(29.93411289716,-0.9316222231426,0.4746852319892));
#17025=CARTESIAN_POINT('Ctrl Pts',(29.88536289716,-0.4252773524951,0.9551885728626));
#17026=CARTESIAN_POINT('Ctrl Pts',(29.83661289716,0.2706170691994,1.009956651308));
#17027=CARTESIAN_POINT('Ctrl Pts',(29.78786289716,0.8458952772121,0.6145788941123));
#17028=CARTESIAN_POINT('Ctrl Pts',(29.73911289716,1.044151128333,-0.05472164524727));
#17029=CARTESIAN_POINT('Ctrl Pts',(29.69036289716,0.7770203858765,-0.6996322864768));
#17030=CARTESIAN_POINT('Ctrl Pts',(29.64161289716,0.1635653887687,-1.03271123699));
#17031=CARTESIAN_POINT('Ctrl Pts',(29.59286289716,-0.5227920508426,-0.9055021853054));
#17032=CARTESIAN_POINT('Ctrl Pts',(29.54411289716,-0.9761367477614,-0.3747044757489));
#17033=CARTESIAN_POINT('Ctrl Pts',(29.49536289716,-0.9944097962471,0.3231057023458));
#17034=CARTESIAN_POINT('Ctrl Pts',(29.44661289716,-0.5694649320687,0.8768914103838));
#17035=CARTESIAN_POINT('Ctrl Pts',(29.39786289716,0.1092896981613,1.039890471984));
#17036=CARTESIAN_POINT('Ctrl Pts',(29.34911289716,0.7393530077902,0.739211848114));
#17037=CARTESIAN_POINT('Ctrl Pts',(29.31661289716,0.939655096844,0.31958395354));
#17038=CARTESIAN_POINT('Ctrl Pts',(29.30036289716,0.962610857739,0.1011744780611));
#17039=CARTESIAN_POINT('Ctrl Pts',(30.79874545428,-1.06875075123,0.1123302303977));
#17040=CARTESIAN_POINT('Ctrl Pts',(30.78249545428,-1.04326383042,0.3548220837953));
#17041=CARTESIAN_POINT('Ctrl Pts',(30.74999545428,-0.820875929403,0.8207192051059));
#17042=CARTESIAN_POINT('Ctrl Pts',(30.70124545428,-0.1213402550703,1.154551410048));
#17043=CARTESIAN_POINT('Ctrl Pts',(30.65249545428,0.6322555672986,0.9735796620828));
#17044=CARTESIAN_POINT('Ctrl Pts',(30.60374545428,1.104055920651,0.3587321494792));
#17045=CARTESIAN_POINT('Ctrl Pts',(30.55499545428,1.083768039895,-0.4160203333738));
#17046=CARTESIAN_POINT('Ctrl Pts',(30.50624545428,0.5804364168376,-1.005345132984));
#17047=CARTESIAN_POINT('Ctrl Pts',(30.45749545428,-0.1816005197909,-1.146580574552));
#17048=CARTESIAN_POINT('Ctrl Pts',(30.40874545428,-0.8626966073051,-0.7767755014867));
#17049=CARTESIAN_POINT('Ctrl Pts',(30.35999545428,-1.159281857079,-0.0607553914402));
#17050=CARTESIAN_POINT('Ctrl Pts',(30.31124545428,-0.9391658173332,0.6823439082283));
#17051=CARTESIAN_POINT('Ctrl Pts',(30.26249545428,-0.3004559876685,1.121317011041));
#17052=CARTESIAN_POINT('Ctrl Pts',(30.21374545428,0.4721695026668,1.060510066561));
#17053=CARTESIAN_POINT('Ctrl Pts',(30.16499545428,1.034345231867,0.5270252191813));
#17054=CARTESIAN_POINT('Ctrl Pts',(30.11624545428,1.135504936741,-0.2413590251076));
#17055=CARTESIAN_POINT('Ctrl Pts',(30.06749545428,0.7305609197345,-0.9021676024575));
#17056=CARTESIAN_POINT('Ctrl Pts',(30.01874545428,-1.947954876406E-14,-1.160872792498));
#17057=CARTESIAN_POINT('Ctrl Pts',(29.96999545428,-0.7305609197346,-0.9021676024575));
#17058=CARTESIAN_POINT('Ctrl Pts',(29.92124545428,-1.135504936741,-0.2413590251076));
#17059=CARTESIAN_POINT('Ctrl Pts',(29.87249545428,-1.034345231867,0.5270252191813));
#17060=CARTESIAN_POINT('Ctrl Pts',(29.82374545428,-0.4721695026667,1.060510066561));
#17061=CARTESIAN_POINT('Ctrl Pts',(29.77499545428,0.3004559876686,1.121317011041));
#17062=CARTESIAN_POINT('Ctrl Pts',(29.72624545428,0.9391658173332,0.6823439082283));
#17063=CARTESIAN_POINT('Ctrl Pts',(29.67749545428,1.159281857079,-0.06075539144024));
#17064=CARTESIAN_POINT('Ctrl Pts',(29.62874545428,0.8626966073051,-0.7767755014868));
#17065=CARTESIAN_POINT('Ctrl Pts',(29.57999545428,0.1816005197909,-1.146580574552));
#17066=CARTESIAN_POINT('Ctrl Pts',(29.53124545428,-0.5804364168377,-1.005345132984));
#17067=CARTESIAN_POINT('Ctrl Pts',(29.48249545428,-1.083768039895,-0.4160203333738));
#17068=CARTESIAN_POINT('Ctrl Pts',(29.43374545428,-1.104055920651,0.3587321494792));
#17069=CARTESIAN_POINT('Ctrl Pts',(29.38499545428,-0.6322555672985,0.9735796620828));
#17070=CARTESIAN_POINT('Ctrl Pts',(29.33624545428,0.1213402550704,1.154551410048));
#17071=CARTESIAN_POINT('Ctrl Pts',(29.28749545428,0.820875929403,0.8207192051059));
#17072=CARTESIAN_POINT('Ctrl Pts',(29.25499545428,1.04326383042,0.3548220837952));
#17073=CARTESIAN_POINT('Ctrl Pts',(29.23874545428,1.06875075123,0.1123302303976));
#17074=CARTESIAN_POINT('Ctrl Pts',(30.7371280114,-1.174890644721,0.1234859827342));
#17075=CARTESIAN_POINT('Ctrl Pts',(30.7208780114,-1.146872563997,0.3900602140506));
#17076=CARTESIAN_POINT('Ctrl Pts',(30.6883780114,-0.9023988510157,0.9022265620979));
#17077=CARTESIAN_POINT('Ctrl Pts',(30.6396280114,-0.1333908119794,1.269212348111));
#17078=CARTESIAN_POINT('Ctrl Pts',(30.5908780114,0.6950462025284,1.070267913782));
#17079=CARTESIAN_POINT('Ctrl Pts',(30.5421280114,1.213702045055,0.3943585966126));
#17080=CARTESIAN_POINT('Ctrl Pts',(30.4933780114,1.191399332028,-0.4573361909988));
#17081=CARTESIAN_POINT('Ctrl Pts',(30.4446280114,0.6380807828327,-1.105188080663));
#17082=CARTESIAN_POINT('Ctrl Pts',(30.3958780114,-0.1996356508131,-1.260449912114));
#17083=CARTESIAN_POINT('Ctrl Pts',(30.3471280114,-0.9483728287337,-0.8539187164967));
#17084=CARTESIAN_POINT('Ctrl Pts',(30.2983780114,-1.274412585824,-0.06678913763317));
#17085=CARTESIAN_POINT('Ctrl Pts',(30.2496280114,-1.032436357454,0.7501089223443));
#17086=CARTESIAN_POINT('Ctrl Pts',(30.2008780114,-0.3302949061378,1.232677370773));
#17087=CARTESIAN_POINT('Ctrl Pts',(30.1521280114,0.5190616528384,1.165831560259));
#17088=CARTESIAN_POINT('Ctrl Pts',(30.1033780114,1.137068240592,0.5793652063734));
#17089=CARTESIAN_POINT('Ctrl Pts',(30.0546280114,1.248274329329,-0.2653288994572));
#17090=CARTESIAN_POINT('Ctrl Pts',(30.0058780114,0.8031144670607,-0.9917637717473));
#17091=CARTESIAN_POINT('Ctrl Pts',(29.9571280114,-1.980022061951E-14,-1.276161520399));
#17092=CARTESIAN_POINT('Ctrl Pts',(29.9083780114,-0.8031144670608,-0.9917637717473));
#17093=CARTESIAN_POINT('Ctrl Pts',(29.8596280114,-1.248274329329,-0.2653288994572));
#17094=CARTESIAN_POINT('Ctrl Pts',(29.8108780114,-1.137068240592,0.5793652063734));
#17095=CARTESIAN_POINT('Ctrl Pts',(29.7621280114,-0.5190616528384,1.165831560259));
#17096=CARTESIAN_POINT('Ctrl Pts',(29.7133780114,0.3302949061378,1.232677370773));
#17097=CARTESIAN_POINT('Ctrl Pts',(29.6646280114,1.032436357454,0.7501089223443));
#17098=CARTESIAN_POINT('Ctrl Pts',(29.6158780114,1.274412585824,-0.06678913763322));
#17099=CARTESIAN_POINT('Ctrl Pts',(29.5671280114,0.9483728287337,-0.8539187164967));
#17100=CARTESIAN_POINT('Ctrl Pts',(29.5183780114,0.1996356508131,-1.260449912114));
#17101=CARTESIAN_POINT('Ctrl Pts',(29.4696280114,-0.6380807828327,-1.105188080663));
#17102=CARTESIAN_POINT('Ctrl Pts',(29.4208780114,-1.191399332028,-0.4573361909987));
#17103=CARTESIAN_POINT('Ctrl Pts',(29.3721280114,-1.213702045055,0.3943585966126));
#17104=CARTESIAN_POINT('Ctrl Pts',(29.3233780114,-0.6950462025284,1.070267913782));
#17105=CARTESIAN_POINT('Ctrl Pts',(29.2746280114,0.1333908119795,1.269212348111));
#17106=CARTESIAN_POINT('Ctrl Pts',(29.2258780114,0.9023988510157,0.9022265620978));
#17107=CARTESIAN_POINT('Ctrl Pts',(29.1933780114,1.146872563997,0.3900602140505));
#17108=CARTESIAN_POINT('Ctrl Pts',(29.1771280114,1.174890644721,0.1234859827342));
#17109=CARTESIAN_POINT('Ctrl Pts',(30.67551056852,-1.281030538212,0.1346417350707));
#17110=CARTESIAN_POINT('Ctrl Pts',(30.65926056852,-1.250481297573,0.4252983443058));
#17111=CARTESIAN_POINT('Ctrl Pts',(30.62676056852,-0.9839217726285,0.9837339190898));
#17112=CARTESIAN_POINT('Ctrl Pts',(30.57801056852,-0.1454413688885,1.383873286175));
#17113=CARTESIAN_POINT('Ctrl Pts',(30.52926056852,0.7578368377583,1.166956165481));
#17114=CARTESIAN_POINT('Ctrl Pts',(30.48051056852,1.323348169458,0.429985043746));
#17115=CARTESIAN_POINT('Ctrl Pts',(30.43176056852,1.299030624161,-0.4986520486237));
#17116=CARTESIAN_POINT('Ctrl Pts',(30.38301056852,0.6957251488278,-1.205031028341));
#17117=CARTESIAN_POINT('Ctrl Pts',(30.33426056852,-0.2176707818353,-1.374319249677));
#17118=CARTESIAN_POINT('Ctrl Pts',(30.28551056852,-1.034049050162,-0.9310619315066));
#17119=CARTESIAN_POINT('Ctrl Pts',(30.23676056852,-1.38954331457,-0.07282288382613));
#17120=CARTESIAN_POINT('Ctrl Pts',(30.18801056852,-1.125706897575,0.8178739364602));
#17121=CARTESIAN_POINT('Ctrl Pts',(30.13926056852,-0.360133824607,1.344037730506));
#17122=CARTESIAN_POINT('Ctrl Pts',(30.09051056852,0.56595380301,1.271153053958));
#17123=CARTESIAN_POINT('Ctrl Pts',(30.04176056852,1.239791249317,0.6317051935655));
#17124=CARTESIAN_POINT('Ctrl Pts',(29.99301056852,1.361043721917,-0.2892987738068));
#17125=CARTESIAN_POINT('Ctrl Pts',(29.94426056852,0.8756680143869,-1.081359941037));
#17126=CARTESIAN_POINT('Ctrl Pts',(29.89551056852,-2.198241588758E-14,-1.3914502483));
#17127=CARTESIAN_POINT('Ctrl Pts',(29.84676056852,-0.875668014387,-1.081359941037));
#17128=CARTESIAN_POINT('Ctrl Pts',(29.79801056852,-1.361043721917,-0.2892987738067));
#17129=CARTESIAN_POINT('Ctrl Pts',(29.74926056852,-1.239791249317,0.6317051935656));
#17130=CARTESIAN_POINT('Ctrl Pts',(29.70051056852,-0.56595380301,1.271153053958));
#17131=CARTESIAN_POINT('Ctrl Pts',(29.65176056852,0.360133824607,1.344037730506));
#17132=CARTESIAN_POINT('Ctrl Pts',(29.60301056852,1.125706897575,0.8178739364602));
#17133=CARTESIAN_POINT('Ctrl Pts',(29.55426056852,1.38954331457,-0.07282288382619));
#17134=CARTESIAN_POINT('Ctrl Pts',(29.50551056852,1.034049050162,-0.9310619315066));
#17135=CARTESIAN_POINT('Ctrl Pts',(29.45676056852,0.2176707818353,-1.374319249677));
#17136=CARTESIAN_POINT('Ctrl Pts',(29.40801056852,-0.6957251488278,-1.205031028341));
#17137=CARTESIAN_POINT('Ctrl Pts',(29.35926056852,-1.299030624161,-0.4986520486236));
#17138=CARTESIAN_POINT('Ctrl Pts',(29.31051056852,-1.323348169458,0.4299850437461));
#17139=CARTESIAN_POINT('Ctrl Pts',(29.26176056852,-0.7578368377582,1.166956165481));
#17140=CARTESIAN_POINT('Ctrl Pts',(29.21301056852,0.1454413688886,1.383873286175));
#17141=CARTESIAN_POINT('Ctrl Pts',(29.16426056852,0.9839217726285,0.9837339190898));
#17142=CARTESIAN_POINT('Ctrl Pts',(29.13176056852,1.250481297573,0.4252983443058));
#17143=CARTESIAN_POINT('Ctrl Pts',(29.11551056852,1.281030538212,0.1346417350707));
#17144=CARTESIAN_POINT('',(29.1676573270715,1.08229570837247,0.624863720396445));
#17145=CARTESIAN_POINT('Ctrl Pts',(29.617627341968,1.08215501597624,0.62476352113272));
#17146=CARTESIAN_POINT('Ctrl Pts',(29.61459741681,1.10800857523719,0.579922158874817));
#17147=CARTESIAN_POINT('Ctrl Pts',(29.6115421791637,1.13109114492466,0.533476323136956));
#17148=CARTESIAN_POINT('Ctrl Pts',(29.5979044654554,1.22146502968022,0.319487471057165));
#17149=CARTESIAN_POINT('Ctrl Pts',(29.5888599482143,1.24922762750675,0.153891219598247));
#17150=CARTESIAN_POINT('Ctrl Pts',(29.5737847077041,1.24989879330249,-0.113832666126114));
#17151=CARTESIAN_POINT('Ctrl Pts',(29.5669031019519,1.23354843079392,-0.230222265136776));
#17152=CARTESIAN_POINT('Ctrl Pts',(29.5560364877087,1.18303861956897,-0.407985503133046));
#17153=CARTESIAN_POINT('Ctrl Pts',(29.5520249813698,1.15886534353969,-0.472541576903855));
#17154=CARTESIAN_POINT('Ctrl Pts',(29.5426236328536,1.08803886439693,-0.622208331795665));
#17155=CARTESIAN_POINT('Ctrl Pts',(29.5373144435947,1.03646342659019,-0.704760379661174));
#17156=CARTESIAN_POINT('Ctrl Pts',(29.5252776000949,0.902890623340095,-0.871840292472444));
#17157=CARTESIAN_POINT('Ctrl Pts',(29.5183993972978,0.81711148767936,-0.952400105380579));
#17158=CARTESIAN_POINT('Ctrl Pts',(29.5072903013536,0.662900641104247,-1.06168646706383));
#17159=CARTESIAN_POINT('Ctrl Pts',(29.5030466274329,0.599916290928708,-1.09861661506134));
#17160=CARTESIAN_POINT('Ctrl Pts',(29.4935499634098,0.448370282102632,-1.17026616405347));
#17161=CARTESIAN_POINT('Ctrl Pts',(29.4883511300327,0.358178885242108,-1.20093403070587));
#17162=CARTESIAN_POINT('Ctrl Pts',(29.4764216575478,0.151089332425558,-1.2459862887354));
#17163=CARTESIAN_POINT('Ctrl Pts',(29.4695340008344,0.0336386874856851,
-1.25443381468143));
#17164=CARTESIAN_POINT('Ctrl Pts',(29.4585602097506,-0.152648874215112,
-1.24216397620102));
#17165=CARTESIAN_POINT('Ctrl Pts',(29.4544538449471,-0.222473817675357,
-1.23166981758508));
#17166=CARTESIAN_POINT('Ctrl Pts',(29.4450136136811,-0.384335500019739,
-1.19293104198071));
#17167=CARTESIAN_POINT('Ctrl Pts',(29.4397494515913,-0.474974442137163,
-1.15981399212218));
#17168=CARTESIAN_POINT('Ctrl Pts',(29.4277636106627,-0.665321913901319,
-1.06424838874914));
#17169=CARTESIAN_POINT('Ctrl Pts',(29.4208892753518,-0.761865224190842,
-0.997128445216505));
#17170=CARTESIAN_POINT('Ctrl Pts',(29.4097593639183,-0.901053681731414,
-0.868778241319131));
#17171=CARTESIAN_POINT('Ctrl Pts',(29.4054913512447,-0.950524419006847,
-0.814508791853337));
#17172=CARTESIAN_POINT('Ctrl Pts',(29.3959883691584,-1.05205634969515,-0.68094437448249));
#17173=CARTESIAN_POINT('Ctrl Pts',(29.3908045259822,-1.10059723896093,-0.599309120618603));
#17174=CARTESIAN_POINT('Ctrl Pts',(29.3801568761226,-1.17827835703337,-0.426851826779456));
#17175=CARTESIAN_POINT('Ctrl Pts',(29.3746502745195,-1.20704346491738,-0.336466924104589));
#17176=CARTESIAN_POINT('Ctrl Pts',(29.3649862290562,-1.2390999636105,-0.1754160308971));
#17177=CARTESIAN_POINT('Ctrl Pts',(29.3608584555161,-1.24704808336017,-0.105612279761285));
#17178=CARTESIAN_POINT('Ctrl Pts',(29.3527448374063,-1.25115038739277,0.0351003553259205));
#17179=CARTESIAN_POINT('Ctrl Pts',(29.3487973845041,-1.24713429538041,0.105792904140653));
#17180=CARTESIAN_POINT('Ctrl Pts',(29.3387661503307,-1.22182615116716,0.284089728846796));
#17181=CARTESIAN_POINT('Ctrl Pts',(29.3326747356135,-1.19237958602683,0.389730367717767));
#17182=CARTESIAN_POINT('Ctrl Pts',(29.3175510069523,-1.09049746262549,0.62776530071626));
#17183=CARTESIAN_POINT('Ctrl Pts',(29.3076789663981,-1.0003923014378,0.771310551286882));
#17184=CARTESIAN_POINT('Ctrl Pts',(29.2940075376696,-0.823883953792329,
0.941501666280569));
#17185=CARTESIAN_POINT('Ctrl Pts',(29.2906548112083,-0.77732146047511,0.980307422285116));
#17186=CARTESIAN_POINT('Ctrl Pts',(29.282259797587,-0.656399188471644,1.06700328117913));
#17187=CARTESIAN_POINT('Ctrl Pts',(29.2771202228619,-0.579432598450008,
1.11052953944549));
#17188=CARTESIAN_POINT('Ctrl Pts',(29.2652769550014,-0.394863984399084,
1.19087511045753));
#17189=CARTESIAN_POINT('Ctrl Pts',(29.2586205770142,-0.284696785371201,
1.22212264404173));
#17190=CARTESIAN_POINT('Ctrl Pts',(29.2476722995244,-0.0914843826785107,
1.24889940201236));
#17191=CARTESIAN_POINT('Ctrl Pts',(29.243215154838,-0.010336908285927,1.25220705415618));
#17192=CARTESIAN_POINT('Ctrl Pts',(29.2332417528454,0.16616149197302,1.24223431935585));
#17193=CARTESIAN_POINT('Ctrl Pts',(29.2276409552425,0.260829710909366,1.22568679187361));
#17194=CARTESIAN_POINT('Ctrl Pts',(29.2159304610313,0.451611747274278,1.169601699981));
#17195=CARTESIAN_POINT('Ctrl Pts',(29.2098673387471,0.547347851324356,1.12817256922947));
#17196=CARTESIAN_POINT('Ctrl Pts',(29.1953702495661,0.769260145843567,0.996707303011102));
#17197=CARTESIAN_POINT('Ctrl Pts',(29.1862505178116,0.897634598070124,0.887573424797484));
#17198=CARTESIAN_POINT('Ctrl Pts',(29.172937791388,1.03241317167635,0.705446011550095));
#17199=CARTESIAN_POINT('Ctrl Pts',(29.1701446500545,1.05843702892822,0.665787836578457));
#17200=CARTESIAN_POINT('Ctrl Pts',(29.1673726659358,1.0821385210664,0.624792090993702));
#17201=CARTESIAN_POINT('',(29.30837346568,0.8712215562072,0.503));
#17202=CARTESIAN_POINT('Ctrl Pts',(29.36036289716,0.5689250970851,0.7830582177302));
#17203=CARTESIAN_POINT('Ctrl Pts',(29.34411289716,0.7465953708295,0.6539732078924));
#17204=CARTESIAN_POINT('Ctrl Pts',(29.31161289716,1.00985274314,0.2706925630537));
#17205=CARTESIAN_POINT('Ctrl Pts',(29.26286289716,0.9552164149722,-0.4252975810125));
#17206=CARTESIAN_POINT('Ctrl Pts',(29.21411289716,0.4746777717184,-0.9316168029278));
#17207=CARTESIAN_POINT('Ctrl Pts',(29.16536289716,-0.2173871517845,-1.022736996495));
#17208=CARTESIAN_POINT('Ctrl Pts',(29.11661289716,-0.812571968791,-0.6580069832544));
#17209=CARTESIAN_POINT('Ctrl Pts',(29.06786289716,-1.045583921078,-1.042734902035E-7));
#17210=CARTESIAN_POINT('Ctrl Pts',(29.01911289716,-0.8125714716224,0.6580074003485));
#17211=CARTESIAN_POINT('Ctrl Pts',(28.97036289716,-0.2173891404584,1.022735536666));
#17212=CARTESIAN_POINT('Ctrl Pts',(28.92161289716,0.4746852292457,0.9316222251505));
#17213=CARTESIAN_POINT('Ctrl Pts',(28.87286289716,0.9551885735371,0.4252773519507));
#17214=CARTESIAN_POINT('Ctrl Pts',(28.82411289716,1.009956651354,-0.2706170690297));
#17215=CARTESIAN_POINT('Ctrl Pts',(28.77536289716,0.614578893256,-0.8458952773463));
#17216=CARTESIAN_POINT('Ctrl Pts',(28.72661289716,-0.0547216418674,-1.044151127966));
#17217=CARTESIAN_POINT('Ctrl Pts',(28.67786289716,-0.69963229914,-0.7770203872106));
#17218=CARTESIAN_POINT('Ctrl Pts',(28.62911289716,-1.032711189717,-0.1635653837992));
#17219=CARTESIAN_POINT('Ctrl Pts',(28.58036289716,-0.9055023617337,0.5227920322988));
#17220=CARTESIAN_POINT('Ctrl Pts',(28.53161289716,-0.3747038173085,0.9761368169669));
#17221=CARTESIAN_POINT('Ctrl Pts',(28.48286289716,0.3231032450129,0.9944095379687));
#17222=CARTESIAN_POINT('Ctrl Pts',(28.43411289716,0.8769005812753,0.5694658959771));
#17223=CARTESIAN_POINT('Ctrl Pts',(28.38536289716,1.039856245751,-0.1092932955163));
#17224=CARTESIAN_POINT('Ctrl Pts',(28.33661289716,0.7393395821542,-0.7393395822784));
#17225=CARTESIAN_POINT('Ctrl Pts',(28.28786289716,0.109293296325,-1.039856246063));
#17226=CARTESIAN_POINT('Ctrl Pts',(28.23911289716,-0.5694658990877,-0.8769005799032));
#17227=CARTESIAN_POINT('Ctrl Pts',(28.19036289716,-0.994409526335,-0.323103250189));
#17228=CARTESIAN_POINT('Ctrl Pts',(28.14161289716,-0.9761368603912,0.3747038366413));
#17229=CARTESIAN_POINT('Ctrl Pts',(28.09286289716,-0.5227918702355,0.905502289579));
#17230=CARTESIAN_POINT('Ctrl Pts',(28.04411289716,0.1635647789705,1.032711459003));
#17231=CARTESIAN_POINT('Ctrl Pts',(27.99536289716,0.7770226444627,0.6996312941492));
#17232=CARTESIAN_POINT('Ctrl Pts',(27.94661289716,1.044142703787,0.05472539254393));
#17233=CARTESIAN_POINT('Ctrl Pts',(27.89786289716,0.845926716811,-0.6145928909717));
#17234=CARTESIAN_POINT('Ctrl Pts',(27.84911289716,0.27049973535,-1.009904411168));
#17235=CARTESIAN_POINT('Ctrl Pts',(27.81661289716,-0.1930597260145,-0.9735571614325));
#17236=CARTESIAN_POINT('Ctrl Pts',(27.80036289716,-0.393685760654,-0.8842326957913));
#17237=CARTESIAN_POINT('Ctrl Pts',(29.29874545428,0.6316562087523,0.86940018568));
#17238=CARTESIAN_POINT('Ctrl Pts',(29.28249545428,0.8289168536007,0.7260819380959));
#17239=CARTESIAN_POINT('Ctrl Pts',(29.24999545428,1.121201645697,0.3005398056651));
#17240=CARTESIAN_POINT('Ctrl Pts',(29.20124545428,1.060540978612,-0.4721919616313));
#17241=CARTESIAN_POINT('Ctrl Pts',(29.15249545428,0.5270169363223,-1.034339214006));
#17242=CARTESIAN_POINT('Ctrl Pts',(29.10374545428,-0.2413568057223,-1.135506549222));
#17243=CARTESIAN_POINT('Ctrl Pts',(29.05499545428,-0.9021681971399,-0.7305604876715));
#17244=CARTESIAN_POINT('Ctrl Pts',(29.00624545428,-1.160872633154,-1.157709476594E-7));
#17245=CARTESIAN_POINT('Ctrl Pts',(28.95749545428,-0.9021676451524,0.7305609507555));
#17246=CARTESIAN_POINT('Ctrl Pts',(28.90874545428,-0.2413590136723,1.135504928428));
#17247=CARTESIAN_POINT('Ctrl Pts',(28.85999545428,0.5270252161353,1.034345234097));
#17248=CARTESIAN_POINT('Ctrl Pts',(28.81124545428,1.06051006731,0.4721695020623));
#17249=CARTESIAN_POINT('Ctrl Pts',(28.76249545428,1.121317011091,-0.3004559874803));
#17250=CARTESIAN_POINT('Ctrl Pts',(28.71374545428,0.6823439072775,-0.9391658174822));
#17251=CARTESIAN_POINT('Ctrl Pts',(28.66499545428,-0.0607553876877,-1.159281856671));
#17252=CARTESIAN_POINT('Ctrl Pts',(28.61624545428,-0.7767755155462,-0.8626966087863));
#17253=CARTESIAN_POINT('Ctrl Pts',(28.56749545428,-1.146580522067,-0.1816005142735));
#17254=CARTESIAN_POINT('Ctrl Pts',(28.51874545428,-1.005345328866,0.5804363962492));
#17255=CARTESIAN_POINT('Ctrl Pts',(28.46999545428,-0.4160196023322,1.083768116731));
#17256=CARTESIAN_POINT('Ctrl Pts',(28.42124545428,0.3587294211946,1.104055633894));
#17257=CARTESIAN_POINT('Ctrl Pts',(28.37249545428,0.9735898441798,0.6322566374899));
#17258=CARTESIAN_POINT('Ctrl Pts',(28.32374545428,1.154513409944,-0.1213442490789));
#17259=CARTESIAN_POINT('Ctrl Pts',(28.27499545428,0.8208610234226,-0.8208610235605));
#17260=CARTESIAN_POINT('Ctrl Pts',(28.22624545428,0.1213442499766,-1.154513410291));
#17261=CARTESIAN_POINT('Ctrl Pts',(28.17749545428,-0.6322566409435,-0.9735898426565));
#17262=CARTESIAN_POINT('Ctrl Pts',(28.12874545428,-1.104055620977,-0.3587294269414));
#17263=CARTESIAN_POINT('Ctrl Pts',(28.07999545428,-1.083768164943,0.4160196237967));
#17264=CARTESIAN_POINT('Ctrl Pts',(28.03124545428,-0.5804362163164,1.005345248755));
#17265=CARTESIAN_POINT('Ctrl Pts',(27.98249545428,0.1815998427548,1.146580821045));
#17266=CARTESIAN_POINT('Ctrl Pts',(27.93374545428,0.8626991149286,0.7767743997426));
#17267=CARTESIAN_POINT('Ctrl Pts',(27.88499545428,1.159272503621,0.06075955192325));
#17268=CARTESIAN_POINT('Ctrl Pts',(27.83624545428,0.9392007235413,-0.6823594484165));
#17269=CARTESIAN_POINT('Ctrl Pts',(27.78749545428,0.300325716294,-1.121259010771));
#17270=CARTESIAN_POINT('Ctrl Pts',(27.75499545428,-0.2143469768198,-1.080904021891));
#17271=CARTESIAN_POINT('Ctrl Pts',(27.73874545428,-0.4370945424777,-0.9817304160776));
#17272=CARTESIAN_POINT('Ctrl Pts',(29.2371280114,0.6943873204196,0.9557421536299));
#17273=CARTESIAN_POINT('Ctrl Pts',(29.2208780114,0.9112383363718,0.7981906682994));
#17274=CARTESIAN_POINT('Ctrl Pts',(29.1883780114,1.232550548254,0.3303870482765));
#17275=CARTESIAN_POINT('Ctrl Pts',(29.1396280114,1.165865542251,-0.5190863422501));
#17276=CARTESIAN_POINT('Ctrl Pts',(29.0908780114,0.5793561009262,-1.137061625084));
#17277=CARTESIAN_POINT('Ctrl Pts',(29.0421280114,-0.26532645966,-1.248276101949));
#17278=CARTESIAN_POINT('Ctrl Pts',(28.9933780114,-0.9917644254889,-0.8031139920886));
#17279=CARTESIAN_POINT('Ctrl Pts',(28.9446280114,-1.27616134523,-1.272684035096E-7));
#17280=CARTESIAN_POINT('Ctrl Pts',(28.8958780114,-0.9917638186823,0.8031145011624));
#17281=CARTESIAN_POINT('Ctrl Pts',(28.8471280114,-0.2653288868863,1.248274320191));
#17282=CARTESIAN_POINT('Ctrl Pts',(28.7983780114,0.5793652030249,1.137068243043));
#17283=CARTESIAN_POINT('Ctrl Pts',(28.7496280114,1.165831561083,0.5190616521739));
#17284=CARTESIAN_POINT('Ctrl Pts',(28.7008780114,1.232677370829,-0.3302949059308));
#17285=CARTESIAN_POINT('Ctrl Pts',(28.6521280114,0.7501089212991,-1.032436357618));
#17286=CARTESIAN_POINT('Ctrl Pts',(28.6033780114,-0.066789133508,-1.274412585376));
#17287=CARTESIAN_POINT('Ctrl Pts',(28.5546280114,-0.8539187319524,-0.948372830362));
#17288=CARTESIAN_POINT('Ctrl Pts',(28.5058780114,-1.260449854417,-0.1996356447477));
#17289=CARTESIAN_POINT('Ctrl Pts',(28.4571280114,-1.105188295998,0.6380807601996));
#17290=CARTESIAN_POINT('Ctrl Pts',(28.4083780114,-0.4573353873558,1.191399416495));
#17291=CARTESIAN_POINT('Ctrl Pts',(28.3596280114,0.3943555973763,1.213701729819));
#17292=CARTESIAN_POINT('Ctrl Pts',(28.3108780114,1.070279107084,0.6950473790027));
#17293=CARTESIAN_POINT('Ctrl Pts',(28.2621280114,1.269170574137,-0.1333952026414));
#17294=CARTESIAN_POINT('Ctrl Pts',(28.2133780114,0.9023824646909,-0.9023824648426));
#17295=CARTESIAN_POINT('Ctrl Pts',(28.1646280114,0.1333952036283,-1.269170574518));
#17296=CARTESIAN_POINT('Ctrl Pts',(28.1158780114,-0.6950473827993,-1.07027910541));
#17297=CARTESIAN_POINT('Ctrl Pts',(28.0671280114,-1.21370171562,-0.3943556036939));
#17298=CARTESIAN_POINT('Ctrl Pts',(28.0183780114,-1.191399469495,0.457335410952));
#17299=CARTESIAN_POINT('Ctrl Pts',(27.9696280114,-0.6380805623973,1.105188207931));
#17300=CARTESIAN_POINT('Ctrl Pts',(27.9208780114,0.1996349065391,1.260450183087));
#17301=CARTESIAN_POINT('Ctrl Pts',(27.8721280114,0.9483755853946,0.853917505336));
#17302=CARTESIAN_POINT('Ctrl Pts',(27.8233780114,1.274402303455,0.06679371130257));
#17303=CARTESIAN_POINT('Ctrl Pts',(27.7746280114,1.032474730272,-0.7501260058614));
#17304=CARTESIAN_POINT('Ctrl Pts',(27.7258780114,0.3301516972379,-1.232613610374));
#17305=CARTESIAN_POINT('Ctrl Pts',(27.6933780114,-0.2356342276251,-1.18825088235));
#17306=CARTESIAN_POINT('Ctrl Pts',(27.6771280114,-0.4805033243014,-1.079228136364));
#17307=CARTESIAN_POINT('Ctrl Pts',(29.17551056852,0.7571184320868,1.04208412158));
#17308=CARTESIAN_POINT('Ctrl Pts',(29.15926056852,0.9935598191429,0.8702993985028));
#17309=CARTESIAN_POINT('Ctrl Pts',(29.12676056852,1.34389945081,0.3602342908879));
#17310=CARTESIAN_POINT('Ctrl Pts',(29.07801056852,1.271190105891,-0.5659807228689));
#17311=CARTESIAN_POINT('Ctrl Pts',(29.02926056852,0.6316952655301,-1.239784036163));
#17312=CARTESIAN_POINT('Ctrl Pts',(28.98051056852,-0.2892961135977,-1.361045654676));
#17313=CARTESIAN_POINT('Ctrl Pts',(28.93176056852,-1.081360653838,-0.8756674965057));
#17314=CARTESIAN_POINT('Ctrl Pts',(28.88301056852,-1.391450057306,-1.387658609686E-7));
#17315=CARTESIAN_POINT('Ctrl Pts',(28.83426056852,-1.081359992212,0.8756680515693));
#17316=CARTESIAN_POINT('Ctrl Pts',(28.78551056852,-0.2892987601002,1.361043711953));
#17317=CARTESIAN_POINT('Ctrl Pts',(28.73676056852,0.6317051899145,1.239791251989));
#17318=CARTESIAN_POINT('Ctrl Pts',(28.68801056852,1.271153054855,0.5659538022855));
#17319=CARTESIAN_POINT('Ctrl Pts',(28.63926056852,1.344037730566,-0.3601338243813));
#17320=CARTESIAN_POINT('Ctrl Pts',(28.59051056852,0.8178739353206,-1.125706897754));
#17321=CARTESIAN_POINT('Ctrl Pts',(28.54176056852,-0.07282287932829,-1.389543314081));
#17322=CARTESIAN_POINT('Ctrl Pts',(28.49301056852,-0.9310619483587,-1.034049051938));
#17323=CARTESIAN_POINT('Ctrl Pts',(28.44426056852,-1.374319186766,-0.217670775222));
#17324=CARTESIAN_POINT('Ctrl Pts',(28.39551056852,-1.20503126313,0.69572512415));
#17325=CARTESIAN_POINT('Ctrl Pts',(28.34676056852,-0.4986511723795,1.299030716259));
#17326=CARTESIAN_POINT('Ctrl Pts',(28.29801056852,0.429981773558,1.323347825744));
#17327=CARTESIAN_POINT('Ctrl Pts',(28.24926056852,1.166968369989,0.7578381205155));
#17328=CARTESIAN_POINT('Ctrl Pts',(28.20051056852,1.383827738331,-0.1454461562039));
#17329=CARTESIAN_POINT('Ctrl Pts',(28.15176056852,0.9839039059593,-0.9839039061246));
#17330=CARTESIAN_POINT('Ctrl Pts',(28.10301056852,0.14544615728,-1.383827738746));
#17331=CARTESIAN_POINT('Ctrl Pts',(28.05426056852,-0.7578381246551,-1.166968368163));
#17332=CARTESIAN_POINT('Ctrl Pts',(28.00551056852,-1.323347810262,-0.4299817804463));
#17333=CARTESIAN_POINT('Ctrl Pts',(27.95676056852,-1.299030774048,0.4986511981073));
#17334=CARTESIAN_POINT('Ctrl Pts',(27.90801056852,-0.6957249084782,1.205031167107));
#17335=CARTESIAN_POINT('Ctrl Pts',(27.85926056852,0.2176699703234,1.374319545129));
#17336=CARTESIAN_POINT('Ctrl Pts',(27.81051056852,1.034052055861,0.9310606109294));
#17337=CARTESIAN_POINT('Ctrl Pts',(27.76176056852,1.389532103288,0.07282787068189));
#17338=CARTESIAN_POINT('Ctrl Pts',(27.71301056852,1.125748737002,-0.8178925633062));
#17339=CARTESIAN_POINT('Ctrl Pts',(27.66426056852,0.3599776781819,-1.343968209978));
#17340=CARTESIAN_POINT('Ctrl Pts',(27.63176056852,-0.2569214784304,-1.295597742809));
#17341=CARTESIAN_POINT('Ctrl Pts',(27.61551056852,-0.5239121061251,-1.17672585665));
#17342=CARTESIAN_POINT('',(28.1173426729269,-1.58041447686304E-9,-1.24972743805679));
#17343=CARTESIAN_POINT('Ctrl Pts',(29.1673856727373,1.08215847935993,0.62480272807601));
#17344=CARTESIAN_POINT('Ctrl Pts',(29.1609968231379,1.13780188993381,0.528907476598624));
#17345=CARTESIAN_POINT('Ctrl Pts',(29.1549070070917,1.18007293410309,0.426766710488715));
#17346=CARTESIAN_POINT('Ctrl Pts',(29.1426003915839,1.23533098518457,0.216609270813267));
#17347=CARTESIAN_POINT('Ctrl Pts',(29.1363846186847,1.24900067471773,0.10985972163656));
#17348=CARTESIAN_POINT('Ctrl Pts',(29.1246079782619,1.24950055350375,-0.0923920289181761));
#17349=CARTESIAN_POINT('Ctrl Pts',(29.1190437443542,1.23898620331935,-0.188034416051438));
#17350=CARTESIAN_POINT('Ctrl Pts',(29.1077827675308,1.19486152256845,-0.380931227675969));
#17351=CARTESIAN_POINT('Ctrl Pts',(29.1021997727515,1.15990323431047,-0.476842290222699));
#17352=CARTESIAN_POINT('Ctrl Pts',(29.0916200775045,1.07536359566911,-0.641674010674401));
#17353=CARTESIAN_POINT('Ctrl Pts',(29.0867995027036,1.03015647433006,-0.711636089148229));
#17354=CARTESIAN_POINT('Ctrl Pts',(29.0763108357406,0.918145662537286,-0.852744715826819));
#17355=CARTESIAN_POINT('Ctrl Pts',(29.0706377368451,0.84887407821414,-0.92207110749063));
#17356=CARTESIAN_POINT('Ctrl Pts',(29.0591400596422,0.690519777313731,-1.04711607636201));
#17357=CARTESIAN_POINT('Ctrl Pts',(29.0534394287303,0.601200097976828,-1.10079838963519));
#17358=CARTESIAN_POINT('Ctrl Pts',(29.0427314765985,0.42969698203359,-1.17621321895953));
#17359=CARTESIAN_POINT('Ctrl Pts',(29.0379106305261,0.350510236428156,-1.2019814912698));
#17360=CARTESIAN_POINT('Ctrl Pts',(29.027445120465,0.174979519771536,-1.2407507654775));
#17361=CARTESIAN_POINT('Ctrl Pts',(29.0217960470484,0.0778867945362808,
-1.2508629837861));
#17362=CARTESIAN_POINT('Ctrl Pts',(29.0103514606849,-0.123010454843654,
-1.24821216732928));
#17363=CARTESIAN_POINT('Ctrl Pts',(29.0046771387381,-0.225730991439992,
-1.23375161025516));
#17364=CARTESIAN_POINT('Ctrl Pts',(28.9939974628599,-0.406028058759957,
-1.18459423747219));
#17365=CARTESIAN_POINT('Ctrl Pts',(28.9891766142402,-0.483792934917113,
-1.15480128143127));
#17366=CARTESIAN_POINT('Ctrl Pts',(28.9787094406642,-0.644644376902829,
-1.07448615399293));
#17367=CARTESIAN_POINT('Ctrl Pts',(28.9730586233196,-0.726493363520805,
-1.02124287488659));
#17368=CARTESIAN_POINT('Ctrl Pts',(28.9616094940918,-0.881023120274798,
-0.892733274025263));
#17369=CARTESIAN_POINT('Ctrl Pts',(28.9559327812777,-0.951788897290975,
-0.816826100660987));
#17370=CARTESIAN_POINT('Ctrl Pts',(28.9452506614896,-1.06100281474115,-0.665128305694781));
#17371=CARTESIAN_POINT('Ctrl Pts',(28.9404298307713,-1.10269161124056,-0.593037192421202));
#17372=CARTESIAN_POINT('Ctrl Pts',(28.9299617104173,-1.17716691154411,-0.429381154843096));
#17373=CARTESIAN_POINT('Ctrl Pts',(28.9243099213453,-1.20727587184561,-0.336478776348865));
#17374=CARTESIAN_POINT('Ctrl Pts',(28.9128589053545,-1.24650146526412,-0.139327474322873));
#17375=CARTESIAN_POINT('Ctrl Pts',(28.9071813054504,-1.25372629152159,-0.0357861780207992));
#17376=CARTESIAN_POINT('Ctrl Pts',(28.8964981796817,-1.24312755625725,0.150850899382122));
#17377=CARTESIAN_POINT('Ctrl Pts',(28.8916773416385,-1.23015475067021,0.233110984081));
#17378=CARTESIAN_POINT('Ctrl Pts',(28.8812097355702,-1.18503744856303,0.407154188490358));
#17379=CARTESIAN_POINT('Ctrl Pts',(28.8755584770246,-1.14997228120041,0.498292059529182));
#17380=CARTESIAN_POINT('Ctrl Pts',(28.8641085952306,-1.05639157416792,0.676175007538576));
#17381=CARTESIAN_POINT('Ctrl Pts',(28.8584315565826,-0.99685151062749,0.761180141227436));
#17382=CARTESIAN_POINT('Ctrl Pts',(28.8477490481642,-0.871168646274408,
0.899548501056932));
#17383=CARTESIAN_POINT('Ctrl Pts',(28.8429282117568,-0.809319472973177,
0.955313355727054));
#17384=CARTESIAN_POINT('Ctrl Pts',(28.8324604491855,-0.664726825936106,
1.0621803476943));
#17385=CARTESIAN_POINT('Ctrl Pts',(28.8268090291305,-0.580119269771693,
1.11094256397802));
#17386=CARTESIAN_POINT('Ctrl Pts',(28.8153608141088,-0.39547571549497,1.19028059577321));
#17387=CARTESIAN_POINT('Ctrl Pts',(28.8096854796079,-0.295740972270812,
1.21886789376563));
#17388=CARTESIAN_POINT('Ctrl Pts',(28.799004920911,-0.111022478533813,1.24731595871076));
#17389=CARTESIAN_POINT('Ctrl Pts',(28.7941840725387,-0.0278621866324802,
1.25173710673691));
#17390=CARTESIAN_POINT('Ctrl Pts',(28.783715371199,0.151777824311083,1.24380664271366));
#17391=CARTESIAN_POINT('Ctrl Pts',(28.7780630096127,0.248233768235987,1.22846011416248));
#17392=CARTESIAN_POINT('Ctrl Pts',(28.7666688661819,0.440745046189595,1.17418381083944));
#17393=CARTESIAN_POINT('Ctrl Pts',(28.761044729133,0.535411455001453,1.13412624208424));
#17394=CARTESIAN_POINT('Ctrl Pts',(28.7504226043197,0.696271670037493,1.0408417898367));
#17395=CARTESIAN_POINT('Ctrl Pts',(28.745601465636,0.763811970201196,0.99208242969822));
#17396=CARTESIAN_POINT('Ctrl Pts',(28.7351059230236,0.89904284123568,0.872862932852518));
#17397=CARTESIAN_POINT('Ctrl Pts',(28.7294265690749,0.964772407202923,0.800013145469062));
#17398=CARTESIAN_POINT('Ctrl Pts',(28.7175549018527,1.08524523589081,0.630024828488589));
#17399=CARTESIAN_POINT('Ctrl Pts',(28.7115121987401,1.13646338425354,0.531967497284216));
#17400=CARTESIAN_POINT('Ctrl Pts',(28.7004178235523,1.20231572056898,0.349876761132139));
#17401=CARTESIAN_POINT('Ctrl Pts',(28.6956005072857,1.22270420461145,0.269312521838998));
#17402=CARTESIAN_POINT('Ctrl Pts',(28.6853025041299,1.24928400747707,0.0944403346743677));
#17403=CARTESIAN_POINT('Ctrl Pts',(28.6798196179985,1.25311307280083,-0.000329806078066004));
#17404=CARTESIAN_POINT('Ctrl Pts',(28.6698538536718,1.24023256691938,-0.175075399992849));
#17405=CARTESIAN_POINT('Ctrl Pts',(28.6654023964275,1.22637185852316,-0.254673920123353));
#17406=CARTESIAN_POINT('Ctrl Pts',(28.656120254182,1.18250126169467,-0.412630540184733));
#17407=CARTESIAN_POINT('Ctrl Pts',(28.651308721134,1.15211009650188,-0.490484077956556));
#17408=CARTESIAN_POINT('Ctrl Pts',(28.6402791571121,1.06621272285659,-0.659611041467915));
#17409=CARTESIAN_POINT('Ctrl Pts',(28.6340423593765,1.0059787604408,-0.748625224630084));
#17410=CARTESIAN_POINT('Ctrl Pts',(28.6235704314111,0.88491755396491,-0.885925058168001));
#17411=CARTESIAN_POINT('Ctrl Pts',(28.619341299677,0.829489182644027,-0.938117904947043));
#17412=CARTESIAN_POINT('Ctrl Pts',(28.6056416940033,0.637217189292378,-1.0880523872875));
#17413=CARTESIAN_POINT('Ctrl Pts',(28.5964663934893,0.493873124613629,-1.1564816575457));
#17414=CARTESIAN_POINT('Ctrl Pts',(28.5832571271695,0.275857378970494,-1.22144536570823));
#17415=CARTESIAN_POINT('Ctrl Pts',(28.5784836206256,0.194162861610605,-1.23735031895491));
#17416=CARTESIAN_POINT('Ctrl Pts',(28.5681687583255,0.0118748310926331,
-1.25389771722638));
#17417=CARTESIAN_POINT('Ctrl Pts',(28.5626389226762,-0.0880714154939871,
-1.25071016360653));
#17418=CARTESIAN_POINT('Ctrl Pts',(28.5495790029823,-0.312377603319782,
-1.21620261797431));
#17419=CARTESIAN_POINT('Ctrl Pts',(28.5421259172881,-0.434727227617343,
-1.17797308587252));
#17420=CARTESIAN_POINT('Ctrl Pts',(28.5259541327221,-0.686696704182463,
-1.05550036517512));
#17421=CARTESIAN_POINT('Ctrl Pts',(28.5176743220364,-0.809974980446674,
-0.964339063317631));
#17422=CARTESIAN_POINT('Ctrl Pts',(28.5018915255945,-0.996684232313097,
-0.762897639913671));
#17423=CARTESIAN_POINT('Ctrl Pts',(28.4947884408799,-1.06605194740329,-0.662310901274681));
#17424=CARTESIAN_POINT('Ctrl Pts',(28.478242069081,-1.19332547341186,-0.406321486463468));
#17425=CARTESIAN_POINT('Ctrl Pts',(28.4693392709946,-1.23647935954279,-0.246852651704806));
#17426=CARTESIAN_POINT('Ctrl Pts',(28.4527491629305,-1.25466077156035,0.0411246745072808));
#17427=CARTESIAN_POINT('Ctrl Pts',(28.445519723942,-1.24435020038222,0.165043891084873));
#17428=CARTESIAN_POINT('Ctrl Pts',(28.4289027367094,-1.17940926325769,0.444977178094289));
#17429=CARTESIAN_POINT('Ctrl Pts',(28.4200489075221,-1.11165294241514,0.594751104676615));
#17430=CARTESIAN_POINT('Ctrl Pts',(28.4032467279876,-0.940922001055101,
0.831567809637354));
#17431=CARTESIAN_POINT('Ctrl Pts',(28.3957655905894,-0.850859018249042,
0.923455894554462));
#17432=CARTESIAN_POINT('Ctrl Pts',(28.379695000864,-0.628378280453494,1.09092775812837));
#17433=CARTESIAN_POINT('Ctrl Pts',(28.3715266034993,-0.493160971631295,
1.15851365987721));
#17434=CARTESIAN_POINT('Ctrl Pts',(28.3559740940566,-0.23287888310737,1.23319870860315));
#17435=CARTESIAN_POINT('Ctrl Pts',(28.3489751243855,-0.113607696680456,
1.24971763753644));
#17436=CARTESIAN_POINT('Ctrl Pts',(28.3324939596632,0.170943447329841,1.24898130791147));
#17437=CARTESIAN_POINT('Ctrl Pts',(28.3235539903221,0.333427313594694,1.21608692054995));
#17438=CARTESIAN_POINT('Ctrl Pts',(28.3071454749248,0.596307822609007,1.10431561727585));
#17439=CARTESIAN_POINT('Ctrl Pts',(28.3001230430521,0.699661147036682,1.04176253692698));
#17440=CARTESIAN_POINT('Ctrl Pts',(28.283626841901,0.920268908395139,0.861552091487536));
#17441=CARTESIAN_POINT('Ctrl Pts',(28.2746953841206,1.02554613396491,0.733653396596494));
#17442=CARTESIAN_POINT('Ctrl Pts',(28.2582441863208,1.15945745744885,0.480551291001781));
#17443=CARTESIAN_POINT('Ctrl Pts',(28.2511735069117,1.20042346896607,0.366020576549046));
#17444=CARTESIAN_POINT('Ctrl Pts',(28.2346450095893,1.25765576767662,0.08631348627535));
#17445=CARTESIAN_POINT('Ctrl Pts',(28.2257275433854,1.25842963526239,-0.079101086624162));
#17446=CARTESIAN_POINT('Ctrl Pts',(28.2091729460902,1.20209026283813,-0.361504893424582));
#17447=CARTESIAN_POINT('Ctrl Pts',(28.2019899388488,1.16064213771058,-0.477888717818062));
#17448=CARTESIAN_POINT('Ctrl Pts',(28.1854044491616,1.02666889684467,-0.731427854742207));
#17449=CARTESIAN_POINT('Ctrl Pts',(28.1765426400489,0.922762085626656,-0.859122704134831));
#17450=CARTESIAN_POINT('Ctrl Pts',(28.1599441436812,0.699673347662511,-1.04230381455487));
#17451=CARTESIAN_POINT('Ctrl Pts',(28.1526754229846,0.592495098195602,-1.10666724822368));
#17452=CARTESIAN_POINT('Ctrl Pts',(28.1360033505331,0.3264006252068,-1.21762615967261));
#17453=CARTESIAN_POINT('Ctrl Pts',(28.1271255168001,0.165037419574197,-1.2499368389208));
#17454=CARTESIAN_POINT('Ctrl Pts',(28.1176143326274,-1.57020897636201E-5,
-1.249578098287));
#17455=CARTESIAN_POINT('',(27.6676389699633,5.88637870807089E-8,-1.24975677572573));
#17456=CARTESIAN_POINT('Ctrl Pts',(28.1176273340642,-1.65623511105583E-5,
-1.24955549515429));
#17457=CARTESIAN_POINT('Ctrl Pts',(28.114597434561,-0.0517766618297808,
-1.24952464781677));
#17458=CARTESIAN_POINT('Ctrl Pts',(28.111542222149,-0.103540795931321,-1.24629187069692));
#17459=CARTESIAN_POINT('Ctrl Pts',(28.0979036849824,-0.33406144677909,-1.21756200064025));
#17460=CARTESIAN_POINT('Ctrl Pts',(28.088858522933,-0.491365261329243,-1.15879939649692));
#17461=CARTESIAN_POINT('Ctrl Pts',(28.0737796659526,-0.723606544051522,
-1.02548045909452));
#17462=CARTESIAN_POINT('Ctrl Pts',(28.0668948495712,-0.816261884977432,
-0.953085469185867));
#17463=CARTESIAN_POINT('Ctrl Pts',(28.0494181450597,-1.02320760685829,-0.73975314249526));
#17464=CARTESIAN_POINT('Ctrl Pts',(28.0403027353165,-1.10952736406557,-0.594731371774655));
#17465=CARTESIAN_POINT('Ctrl Pts',(28.0251273885272,-1.20721997126105,-0.343480859683428));
#17466=CARTESIAN_POINT('Ctrl Pts',(28.0182320724213,-1.23389522300968,-0.228649129135059));
#17467=CARTESIAN_POINT('Ctrl Pts',(28.0007833825742,-1.26074007501739,0.0670551869020103));
#17468=CARTESIAN_POINT('Ctrl Pts',(27.9916773707338,-1.2369704103679,0.233902809861688));
#17469=CARTESIAN_POINT('Ctrl Pts',(27.9765170782386,-1.15523094543665,0.490596117452913));
#17470=CARTESIAN_POINT('Ctrl Pts',(27.9696504679827,-1.10410954293391,0.596333410766813));
#17471=CARTESIAN_POINT('Ctrl Pts',(27.9584962475405,-0.998929190634868,
0.754248903470159));
#17472=CARTESIAN_POINT('Ctrl Pts',(27.9541973498062,-0.952707784063023,
0.812003758880748));
#17473=CARTESIAN_POINT('Ctrl Pts',(27.9446828069813,-0.836372557148644,
0.933237617417355));
#17474=CARTESIAN_POINT('Ctrl Pts',(27.9395147789793,-0.76352459211252,0.99371067926825));
#17475=CARTESIAN_POINT('Ctrl Pts',(27.9276110431682,-0.586654373116962,
1.10958073156092));
#17476=CARTESIAN_POINT('Ctrl Pts',(27.9207162695047,-0.479901383405464,
1.1595048481225));
#17477=CARTESIAN_POINT('Ctrl Pts',(27.9102433336147,-0.309658999011491,
1.2121249866436));
#17478=CARTESIAN_POINT('Ctrl Pts',(27.9066355286707,-0.249344448199697,
1.22602349690604));
#17479=CARTESIAN_POINT('Ctrl Pts',(27.8996144255548,-0.127684267857531,
1.24460926497425));
#17480=CARTESIAN_POINT('Ctrl Pts',(27.8961978838974,-0.0664023934340222,
1.24936472140608));
#17481=CARTESIAN_POINT('Ctrl Pts',(27.8868889978988,0.100755768653574,1.25004530085504));
#17482=CARTESIAN_POINT('Ctrl Pts',(27.8809844783008,0.205835675470576,1.23711210933622));
#17483=CARTESIAN_POINT('Ctrl Pts',(27.866063896433,0.453204407927191,1.1738612253448));
#17484=CARTESIAN_POINT('Ctrl Pts',(27.856213080806,0.608698407592886,1.10681429561789));
#17485=CARTESIAN_POINT('Ctrl Pts',(27.8395800869788,0.846351136838392,0.926418544103274));
#17486=CARTESIAN_POINT('Ctrl Pts',(27.8332688401072,0.927130493094757,0.845659476794221));
#17487=CARTESIAN_POINT('Ctrl Pts',(27.8186212718494,1.07846991579612,0.645463686210442));
#17488=CARTESIAN_POINT('Ctrl Pts',(27.8092257227739,1.15640644586381,0.505721482317762));
#17489=CARTESIAN_POINT('Ctrl Pts',(27.7954118410962,1.22259629351538,0.26771901643447));
#17490=CARTESIAN_POINT('Ctrl Pts',(27.7915580466048,1.23564912429041,0.199007734412521));
#17491=CARTESIAN_POINT('Ctrl Pts',(27.7821086507589,1.25304459091087,0.0322260207484144));
#17492=CARTESIAN_POINT('Ctrl Pts',(27.7763945867012,1.25156055595434,-0.0659228708369851));
#17493=CARTESIAN_POINT('Ctrl Pts',(27.7642947702092,1.22482575759592,-0.269777035042931));
#17494=CARTESIAN_POINT('Ctrl Pts',(27.7579805476016,1.19694742303447,-0.375180422268098));
#17495=CARTESIAN_POINT('Ctrl Pts',(27.7473290248235,1.12462059282187,-0.550801416131723));
#17496=CARTESIAN_POINT('Ctrl Pts',(27.7428588117817,1.08644298546842,-0.622744909367946));
#17497=CARTESIAN_POINT('Ctrl Pts',(27.7330032437985,0.99004410923169,-0.76816749366027));
#17498=CARTESIAN_POINT('Ctrl Pts',(27.7275452739627,0.929840142731238,-0.83980225227136));
#17499=CARTESIAN_POINT('Ctrl Pts',(27.7159670225675,0.787597811969291,-0.975531989088523));
#17500=CARTESIAN_POINT('Ctrl Pts',(27.7098877499555,0.703663058459404,-1.03791885621826));
#17501=CARTESIAN_POINT('Ctrl Pts',(27.6953515319807,0.478261841137807,-1.16472539300529));
#17502=CARTESIAN_POINT('Ctrl Pts',(27.6862138350629,0.319229236952419,-1.22135269437979));
#17503=CARTESIAN_POINT('Ctrl Pts',(27.6729043749472,0.0941610011493839,
-1.24685136243848));
#17504=CARTESIAN_POINT('Ctrl Pts',(27.6701280384454,0.0470868928079041,
-1.24952748149934));
#17505=CARTESIAN_POINT('Ctrl Pts',(27.6673726054814,1.55296021863114E-5,
-1.24955549576934));
#17506=CARTESIAN_POINT('',(27.8084092102543,1.84542703834228E-6,-1.0059988235311));
#17507=CARTESIAN_POINT('',(27.80837346568,-3.363943902264E-14,-1.006));
#17508=CARTESIAN_POINT('Ctrl Pts',(29.3083864422337,0.870773359785393,0.50273974407169));
#17509=CARTESIAN_POINT('Ctrl Pts',(29.3008521885262,0.923830150460179,0.411176385780162));
#17510=CARTESIAN_POINT('Ctrl Pts',(29.2920928354003,0.972239729359923,0.295767848335686));
#17511=CARTESIAN_POINT('Ctrl Pts',(29.2731153143574,1.01254518840658,0.032506499430731));
#17512=CARTESIAN_POINT('Ctrl Pts',(29.2642892222818,1.00848954053166,-0.0936168937764817));
#17513=CARTESIAN_POINT('Ctrl Pts',(29.2460042305897,0.954288507126743,-0.344674989241621));
#17514=CARTESIAN_POINT('Ctrl Pts',(29.2367588244469,0.901467497815239,-0.465863888580671));
#17515=CARTESIAN_POINT('Ctrl Pts',(29.2180479571781,0.750666938273129,-0.68107453632207));
#17516=CARTESIAN_POINT('Ctrl Pts',(29.2088151157514,0.655791268906725,-0.773156797467887));
#17517=CARTESIAN_POINT('Ctrl Pts',(29.1886171121703,0.4183279909562,-0.928000835580233));
#17518=CARTESIAN_POINT('Ctrl Pts',(29.1792516786671,0.290445664438387,-0.968960876829268));
#17519=CARTESIAN_POINT('Ctrl Pts',(29.1624059009713,0.0575864727316603,
-1.01153056273425));
#17520=CARTESIAN_POINT('Ctrl Pts',(29.1534069464231,-0.0710782558689916,
-1.01133291870579));
#17521=CARTESIAN_POINT('Ctrl Pts',(29.1342989682696,-0.33408320271348,-0.95951102980604));
#17522=CARTESIAN_POINT('Ctrl Pts',(29.1247947693779,-0.458249759673372,
-0.903490004899863));
#17523=CARTESIAN_POINT('Ctrl Pts',(29.1082077163494,-0.651606739985276,
-0.773324037322213));
#17524=CARTESIAN_POINT('Ctrl Pts',(29.0990210738255,-0.750738679733316,
-0.686734029266899));
#17525=CARTESIAN_POINT('Ctrl Pts',(29.0788719338336,-0.908027886469017,
-0.45174961613479));
#17526=CARTESIAN_POINT('Ctrl Pts',(29.069460600101,-0.959648553525928,-0.327158651203322));
#17527=CARTESIAN_POINT('Ctrl Pts',(29.0505675506108,-1.01247717924914,-0.0671105513275628));
#17528=CARTESIAN_POINT('Ctrl Pts',(29.0413142276786,-1.01261280867459,0.0652074783840518));
#17529=CARTESIAN_POINT('Ctrl Pts',(29.0226106191189,-0.960786276316734,
0.322740178671338));
#17530=CARTESIAN_POINT('Ctrl Pts',(29.0133914653586,-0.910941399638767,
0.44497502400733));
#17531=CARTESIAN_POINT('Ctrl Pts',(28.9931854475346,-0.755567145070642,
0.682208090561088));
#17532=CARTESIAN_POINT('Ctrl Pts',(28.9838067366341,-0.654636111382683,
0.771092380231502));
#17533=CARTESIAN_POINT('Ctrl Pts',(28.9670009367567,-0.4589204170802,0.903256265996078));
#17534=CARTESIAN_POINT('Ctrl Pts',(28.9580168824801,-0.34122541900454,0.954680725569356));
#17535=CARTESIAN_POINT('Ctrl Pts',(28.9394916971386,-0.0875413822859824,
1.01111645447045));
#17536=CARTESIAN_POINT('Ctrl Pts',(28.9299862507462,0.0486169665867024,
1.01287742140832));
#17537=CARTESIAN_POINT('Ctrl Pts',(28.9128021772271,0.286247499755411,0.969965709350142));
#17538=CARTESIAN_POINT('Ctrl Pts',(28.9036116032874,0.411828409927549,0.930377288092358));
#17539=CARTESIAN_POINT('Ctrl Pts',(28.8834719027533,0.650119117375473,0.778369367719755));
#17540=CARTESIAN_POINT('Ctrl Pts',(28.8740686495798,0.747374114001158,0.685109299358981));
#17541=CARTESIAN_POINT('Ctrl Pts',(28.855169283962,0.900301395997063,0.46815105805523));
#17542=CARTESIAN_POINT('Ctrl Pts',(28.8459048150744,0.953566173341328,0.346849748046555));
#17543=CARTESIAN_POINT('Ctrl Pts',(28.8272137745117,1.00948095071544,0.0903434934989256));
#17544=CARTESIAN_POINT('Ctrl Pts',(28.8180068956468,1.01296598826026,-0.0414324395852837));
#17545=CARTESIAN_POINT('Ctrl Pts',(28.7977899305546,0.96601949268219,-0.321250069431297));
#17546=CARTESIAN_POINT('Ctrl Pts',(28.7883977032764,0.909104926108196,-0.443337235931546));
#17547=CARTESIAN_POINT('Ctrl Pts',(28.7716308252545,0.783304765554663,-0.642559988636238));
#17548=CARTESIAN_POINT('Ctrl Pts',(28.7626606378465,0.696376860255621,-0.736824922057778));
#17549=CARTESIAN_POINT('Ctrl Pts',(28.7441622029206,0.48711729937632,-0.890303235238164));
#17550=CARTESIAN_POINT('Ctrl Pts',(28.7346587869632,0.363230754563944,-0.946762314668834));
#17551=CARTESIAN_POINT('Ctrl Pts',(28.7174342420197,0.127880192190257,-1.00327016540539));
#17552=CARTESIAN_POINT('Ctrl Pts',(28.7082400320689,-0.00307419136589923,
-1.01744177706707));
#17553=CARTESIAN_POINT('Ctrl Pts',(28.6881085385381,-0.28226357624072,-0.974048387998716));
#17554=CARTESIAN_POINT('Ctrl Pts',(28.6787128604578,-0.408717770745895,
-0.927836026440964));
#17555=CARTESIAN_POINT('Ctrl Pts',(28.6598090757102,-0.636054869835315,
-0.790710405276924));
#17556=CARTESIAN_POINT('Ctrl Pts',(28.6505332144177,-0.733676604436167,
-0.700904969244602));
#17557=CARTESIAN_POINT('Ctrl Pts',(28.6318547354579,-0.887904373733202,
-0.488659821461708));
#17558=CARTESIAN_POINT('Ctrl Pts',(28.6226591218941,-0.944048573936195,
-0.369579698988372));
#17559=CARTESIAN_POINT('Ctrl Pts',(28.6024311543348,-1.01369908580114,-0.0943832969988881));
#17560=CARTESIAN_POINT('Ctrl Pts',(28.593026368846,-1.01058265066987,0.0404795504745563));
#17561=CARTESIAN_POINT('Ctrl Pts',(28.5762958650646,-0.975656602098983,
0.272979304096125));
#17562=CARTESIAN_POINT('Ctrl Pts',(28.5673383109915,-0.934104160209119,
0.394084134956389));
#17563=CARTESIAN_POINT('Ctrl Pts',(28.5494086203685,-0.808338952205143,
0.611915865043621));
#17564=CARTESIAN_POINT('Ctrl Pts',(28.5404510663023,-0.724235313104038,
0.708453750739589));
#17565=CARTESIAN_POINT('Ctrl Pts',(28.523720562521,-0.540347644379399,0.854950472866602));
#17566=CARTESIAN_POINT('Ctrl Pts',(28.5143157770323,-0.425111210006109,
0.925080808596303));
#17567=CARTESIAN_POINT('Ctrl Pts',(28.4940878094729,-0.151958878920122,
1.00235989692945));
#17568=CARTESIAN_POINT('Ctrl Pts',(28.4848921959089,-0.0207603676706828,
1.01327765451514));
#17569=CARTESIAN_POINT('Ctrl Pts',(28.466213716949,0.240163206787955,0.985835062226093));
#17570=CARTESIAN_POINT('Ctrl Pts',(28.4569378556565,0.366747863090104,0.946194878116318));
#17571=CARTESIAN_POINT('Ctrl Pts',(28.4380340709089,0.599170684072258,0.817877985664096));
#17572=CARTESIAN_POINT('Ctrl Pts',(28.4286383928286,0.702418860402568,0.731471621586338));
#17573=CARTESIAN_POINT('Ctrl Pts',(28.408506899298,0.879593330129104,0.511383216351959));
#17574=CARTESIAN_POINT('Ctrl Pts',(28.3993126893472,0.932797546195434,0.390887587624588));
#17575=CARTESIAN_POINT('Ctrl Pts',(28.3820881444036,1.00153559313095,0.158814096445713));
#17576=CARTESIAN_POINT('Ctrl Pts',(28.3725847284462,1.01458386847578,0.0232956617357079));
#17577=CARTESIAN_POINT('Ctrl Pts',(28.3540862935203,0.986297530771062,-0.234667590561133));
#17578=CARTESIAN_POINT('Ctrl Pts',(28.3451161061124,0.94812565639132,-0.357081831558977));
#17579=CARTESIAN_POINT('Ctrl Pts',(28.3283492280907,0.838493771813711,-0.565639342750808));
#17580=CARTESIAN_POINT('Ctrl Pts',(28.3189570008126,0.761220467435563,-0.675972386498997));
#17581=CARTESIAN_POINT('Ctrl Pts',(28.2987400357204,0.542364539351688,-0.856538059210497));
#17582=CARTESIAN_POINT('Ctrl Pts',(28.2895331568556,0.426500714921247,-0.919407894705333));
#17583=CARTESIAN_POINT('Ctrl Pts',(28.2708421162929,0.17640239356655,-0.999237404326076));
#17584=CARTESIAN_POINT('Ctrl Pts',(28.2615776474052,0.0447199889143341,
-1.01375940902338));
#17585=CARTESIAN_POINT('Ctrl Pts',(28.2426782817872,-0.219635000613443,
-0.989799618535093));
#17586=CARTESIAN_POINT('Ctrl Pts',(28.2332750286137,-0.349028087285606,
-0.952204354992624));
#17587=CARTESIAN_POINT('Ctrl Pts',(28.2131353280796,-0.599816161628714,
-0.821842509043127));
#17588=CARTESIAN_POINT('Ctrl Pts',(28.2039447541399,-0.696891195219628,
-0.73288046123261));
#17589=CARTESIAN_POINT('Ctrl Pts',(28.1867606806209,-0.852869094566055,
-0.548542238822853));
#17590=CARTESIAN_POINT('Ctrl Pts',(28.1772552342284,-0.919423226898889,
-0.429745166292887));
#17591=CARTESIAN_POINT('Ctrl Pts',(28.158730048887,-0.997390470348596,-0.181830481509589));
#17592=CARTESIAN_POINT('Ctrl Pts',(28.1497459946104,-1.01170308102003,-0.0541913934911194));
#17593=CARTESIAN_POINT('Ctrl Pts',(28.132940194733,-0.995103645636232,0.181385312576464));
#17594=CARTESIAN_POINT('Ctrl Pts',(28.1235614838324,-0.968593109628244,
0.313236296615785));
#17595=CARTESIAN_POINT('Ctrl Pts',(28.1033554660083,-0.840830374658895,
0.566410881442946));
#17596=CARTESIAN_POINT('Ctrl Pts',(28.094136312248,-0.759894331709154,0.670695233562644));
#17597=CARTESIAN_POINT('Ctrl Pts',(28.0754327036883,-0.562777737133924,
0.844344677318257));
#17598=CARTESIAN_POINT('Ctrl Pts',(28.066179380756,-0.448119147312189,0.910386233646077));
#17599=CARTESIAN_POINT('Ctrl Pts',(28.0472863312657,-0.196496573752323,
0.994659351660517));
#17600=CARTESIAN_POINT('Ctrl Pts',(28.037874997533,-0.0627872995112181,
1.01225002509461));
#17601=CARTESIAN_POINT('Ctrl Pts',(28.017725857541,0.219359775122049,0.993525782886262));
#17602=CARTESIAN_POINT('Ctrl Pts',(28.0085392150173,0.343914891685593,0.950970008765679));
#17603=CARTESIAN_POINT('Ctrl Pts',(27.9919521619889,0.553320416471902,0.848600935605234));
#17604=CARTESIAN_POINT('Ctrl Pts',(27.9824479630972,0.663919325666461,0.769080055430507));
#17605=CARTESIAN_POINT('Ctrl Pts',(27.9633399849438,0.840300871347782,0.56722203459224));
#17606=CARTESIAN_POINT('Ctrl Pts',(27.9543410303957,0.904804400397691,0.455893933067184));
#17607=CARTESIAN_POINT('Ctrl Pts',(27.9374952527,0.984367566826246,0.23294711459173));
#17608=CARTESIAN_POINT('Ctrl Pts',(27.9281298191968,1.01283629382342,0.101717750507591));
#17609=CARTESIAN_POINT('Ctrl Pts',(27.9079318156157,0.997469062168756,-0.181353499719985));
#17610=CARTESIAN_POINT('Ctrl Pts',(27.8986989741889,0.965161319461705,-0.309559370165414));
#17611=CARTESIAN_POINT('Ctrl Pts',(27.8799881069201,0.85418371112365,-0.547761809504526));
#17612=CARTESIAN_POINT('Ctrl Pts',(27.8707427007773,0.775641550295086,-0.654100595091252));
#17613=CARTESIAN_POINT('Ctrl Pts',(27.8524577057846,0.5853193441443,-0.826569145795593));
#17614=CARTESIAN_POINT('Ctrl Pts',(27.8436316104026,0.478121059661468,-0.893143155202069));
#17615=CARTESIAN_POINT('Ctrl Pts',(27.8246541289103,0.229977818093696,-0.989868041870531));
#17616=CARTESIAN_POINT('Ctrl Pts',(27.8158948070511,0.105826781086848,-1.0056484510065));
#17617=CARTESIAN_POINT('Ctrl Pts',(27.8083605733564,2.47301423003647E-6,
-1.00548172441298));
#17618=CARTESIAN_POINT('Ctrl Pts',(29.66948943148,0.7571184320868,1.04208412158));
#17619=CARTESIAN_POINT('Ctrl Pts',(29.65323943148,0.9935598191429,0.8702993985028));
#17620=CARTESIAN_POINT('Ctrl Pts',(29.62073943148,1.34389945081,0.360234290888));
#17621=CARTESIAN_POINT('Ctrl Pts',(29.57198943148,1.271190105891,-0.5659807228689));
#17622=CARTESIAN_POINT('Ctrl Pts',(29.52323943148,0.6316952655301,-1.239784036163));
#17623=CARTESIAN_POINT('Ctrl Pts',(29.47448943148,-0.2892961135977,-1.361045654676));
#17624=CARTESIAN_POINT('Ctrl Pts',(29.42573943148,-1.081360653838,-0.8756674965057));
#17625=CARTESIAN_POINT('Ctrl Pts',(29.37698943148,-1.391450057306,-1.387658549734E-7));
#17626=CARTESIAN_POINT('Ctrl Pts',(29.32823943148,-1.081359992212,0.8756680515693));
#17627=CARTESIAN_POINT('Ctrl Pts',(29.27948943148,-0.2892987601002,1.361043711953));
#17628=CARTESIAN_POINT('Ctrl Pts',(29.23073943148,0.6317051899145,1.239791251989));
#17629=CARTESIAN_POINT('Ctrl Pts',(29.18198943148,1.271153054855,0.5659538022855));
#17630=CARTESIAN_POINT('Ctrl Pts',(29.13323943148,1.344037730566,-0.3601338243813));
#17631=CARTESIAN_POINT('Ctrl Pts',(29.08448943148,0.8178739353206,-1.125706897754));
#17632=CARTESIAN_POINT('Ctrl Pts',(29.03573943148,-0.07282287932829,-1.389543314081));
#17633=CARTESIAN_POINT('Ctrl Pts',(28.98698943148,-0.9310619483587,-1.034049051938));
#17634=CARTESIAN_POINT('Ctrl Pts',(28.93823943148,-1.374319186766,-0.217670775222));
#17635=CARTESIAN_POINT('Ctrl Pts',(28.88948943148,-1.20503126313,0.69572512415));
#17636=CARTESIAN_POINT('Ctrl Pts',(28.84073943148,-0.4986511723795,1.299030716259));
#17637=CARTESIAN_POINT('Ctrl Pts',(28.79198943148,0.429981773558,1.323347825744));
#17638=CARTESIAN_POINT('Ctrl Pts',(28.74323943148,1.166968369989,0.7578381205155));
#17639=CARTESIAN_POINT('Ctrl Pts',(28.69448943148,1.383827738331,-0.1454461562039));
#17640=CARTESIAN_POINT('Ctrl Pts',(28.64573943148,0.9839039059593,-0.9839039061246));
#17641=CARTESIAN_POINT('Ctrl Pts',(28.59698943148,0.14544615728,-1.383827738746));
#17642=CARTESIAN_POINT('Ctrl Pts',(28.54823943148,-0.7578381246551,-1.166968368163));
#17643=CARTESIAN_POINT('Ctrl Pts',(28.49948943148,-1.323347810262,-0.4299817804463));
#17644=CARTESIAN_POINT('Ctrl Pts',(28.45073943148,-1.299030774048,0.4986511981073));
#17645=CARTESIAN_POINT('Ctrl Pts',(28.40198943148,-0.6957249084782,1.205031167107));
#17646=CARTESIAN_POINT('Ctrl Pts',(28.35323943148,0.2176699703234,1.374319545129));
#17647=CARTESIAN_POINT('Ctrl Pts',(28.30448943148,1.034052055861,0.9310606109294));
#17648=CARTESIAN_POINT('Ctrl Pts',(28.25573943148,1.389532103288,0.0728278706819));
#17649=CARTESIAN_POINT('Ctrl Pts',(28.20698943148,1.125748737002,-0.8178925633062));
#17650=CARTESIAN_POINT('Ctrl Pts',(28.15823943148,0.3599776781819,-1.343968209978));
#17651=CARTESIAN_POINT('Ctrl Pts',(28.12573943148,-0.2569214784304,-1.295597742809));
#17652=CARTESIAN_POINT('Ctrl Pts',(28.10948943148,-0.5239121061251,-1.17672585665));
#17653=CARTESIAN_POINT('Ctrl Pts',(29.6078719886,0.6943873204196,0.9557421536299));
#17654=CARTESIAN_POINT('Ctrl Pts',(29.5916219886,0.9112383363718,0.7981906682994));
#17655=CARTESIAN_POINT('Ctrl Pts',(29.5591219886,1.232550548254,0.3303870482766));
#17656=CARTESIAN_POINT('Ctrl Pts',(29.5103719886,1.165865542251,-0.5190863422501));
#17657=CARTESIAN_POINT('Ctrl Pts',(29.4616219886,0.5793561009262,-1.137061625084));
#17658=CARTESIAN_POINT('Ctrl Pts',(29.4128719886,-0.26532645966,-1.248276101949));
#17659=CARTESIAN_POINT('Ctrl Pts',(29.3641219886,-0.9917644254889,-0.8031139920886));
#17660=CARTESIAN_POINT('Ctrl Pts',(29.3153719886,-1.27616134523,-1.272683984522E-7));
#17661=CARTESIAN_POINT('Ctrl Pts',(29.2666219886,-0.9917638186823,0.8031145011624));
#17662=CARTESIAN_POINT('Ctrl Pts',(29.2178719886,-0.2653288868863,1.248274320191));
#17663=CARTESIAN_POINT('Ctrl Pts',(29.1691219886,0.5793652030249,1.137068243043));
#17664=CARTESIAN_POINT('Ctrl Pts',(29.1203719886,1.165831561083,0.5190616521739));
#17665=CARTESIAN_POINT('Ctrl Pts',(29.0716219886,1.232677370829,-0.3302949059308));
#17666=CARTESIAN_POINT('Ctrl Pts',(29.0228719886,0.7501089212991,-1.032436357618));
#17667=CARTESIAN_POINT('Ctrl Pts',(28.9741219886,-0.066789133508,-1.274412585376));
#17668=CARTESIAN_POINT('Ctrl Pts',(28.9253719886,-0.8539187319524,-0.948372830362));
#17669=CARTESIAN_POINT('Ctrl Pts',(28.8766219886,-1.260449854417,-0.1996356447477));
#17670=CARTESIAN_POINT('Ctrl Pts',(28.8278719886,-1.105188295998,0.6380807601996));
#17671=CARTESIAN_POINT('Ctrl Pts',(28.7791219886,-0.4573353873558,1.191399416495));
#17672=CARTESIAN_POINT('Ctrl Pts',(28.7303719886,0.3943555973763,1.213701729819));
#17673=CARTESIAN_POINT('Ctrl Pts',(28.6816219886,1.070279107084,0.6950473790027));
#17674=CARTESIAN_POINT('Ctrl Pts',(28.6328719886,1.269170574137,-0.1333952026414));
#17675=CARTESIAN_POINT('Ctrl Pts',(28.5841219886,0.9023824646909,-0.9023824648426));
#17676=CARTESIAN_POINT('Ctrl Pts',(28.5353719886,0.1333952036283,-1.269170574518));
#17677=CARTESIAN_POINT('Ctrl Pts',(28.4866219886,-0.6950473827993,-1.07027910541));
#17678=CARTESIAN_POINT('Ctrl Pts',(28.4378719886,-1.21370171562,-0.3943556036939));
#17679=CARTESIAN_POINT('Ctrl Pts',(28.3891219886,-1.191399469495,0.457335410952));
#17680=CARTESIAN_POINT('Ctrl Pts',(28.3403719886,-0.6380805623973,1.105188207931));
#17681=CARTESIAN_POINT('Ctrl Pts',(28.2916219886,0.1996349065391,1.260450183087));
#17682=CARTESIAN_POINT('Ctrl Pts',(28.2428719886,0.9483755853946,0.853917505336));
#17683=CARTESIAN_POINT('Ctrl Pts',(28.1941219886,1.274402303455,0.06679371130257));
#17684=CARTESIAN_POINT('Ctrl Pts',(28.1453719886,1.032474730272,-0.7501260058614));
#17685=CARTESIAN_POINT('Ctrl Pts',(28.0966219886,0.3301516972379,-1.232613610374));
#17686=CARTESIAN_POINT('Ctrl Pts',(28.0641219886,-0.2356342276251,-1.18825088235));
#17687=CARTESIAN_POINT('Ctrl Pts',(28.0478719886,-0.4805033243014,-1.079228136364));
#17688=CARTESIAN_POINT('Ctrl Pts',(29.54625454572,0.6316562087523,0.86940018568));
#17689=CARTESIAN_POINT('Ctrl Pts',(29.53000454572,0.8289168536007,0.7260819380959));
#17690=CARTESIAN_POINT('Ctrl Pts',(29.49750454572,1.121201645697,0.3005398056651));
#17691=CARTESIAN_POINT('Ctrl Pts',(29.44875454572,1.060540978612,-0.4721919616313));
#17692=CARTESIAN_POINT('Ctrl Pts',(29.40000454572,0.5270169363223,-1.034339214006));
#17693=CARTESIAN_POINT('Ctrl Pts',(29.35125454572,-0.2413568057223,-1.135506549222));
#17694=CARTESIAN_POINT('Ctrl Pts',(29.30250454572,-0.9021681971399,-0.7305604876715));
#17695=CARTESIAN_POINT('Ctrl Pts',(29.25375454572,-1.160872633154,-1.157709407763E-7));
#17696=CARTESIAN_POINT('Ctrl Pts',(29.20500454572,-0.9021676451524,0.7305609507555));
#17697=CARTESIAN_POINT('Ctrl Pts',(29.15625454572,-0.2413590136723,1.135504928428));
#17698=CARTESIAN_POINT('Ctrl Pts',(29.10750454572,0.5270252161353,1.034345234097));
#17699=CARTESIAN_POINT('Ctrl Pts',(29.05875454572,1.06051006731,0.4721695020623));
#17700=CARTESIAN_POINT('Ctrl Pts',(29.01000454572,1.121317011091,-0.3004559874803));
#17701=CARTESIAN_POINT('Ctrl Pts',(28.96125454572,0.6823439072775,-0.9391658174822));
#17702=CARTESIAN_POINT('Ctrl Pts',(28.91250454572,-0.0607553876877,-1.159281856671));
#17703=CARTESIAN_POINT('Ctrl Pts',(28.86375454572,-0.7767755155462,-0.8626966087863));
#17704=CARTESIAN_POINT('Ctrl Pts',(28.81500454572,-1.146580522067,-0.1816005142735));
#17705=CARTESIAN_POINT('Ctrl Pts',(28.76625454572,-1.005345328866,0.5804363962492));
#17706=CARTESIAN_POINT('Ctrl Pts',(28.71750454572,-0.4160196023322,1.083768116731));
#17707=CARTESIAN_POINT('Ctrl Pts',(28.66875454572,0.3587294211946,1.104055633894));
#17708=CARTESIAN_POINT('Ctrl Pts',(28.62000454572,0.9735898441798,0.6322566374899));
#17709=CARTESIAN_POINT('Ctrl Pts',(28.57125454572,1.154513409944,-0.1213442490789));
#17710=CARTESIAN_POINT('Ctrl Pts',(28.52250454572,0.8208610234226,-0.8208610235605));
#17711=CARTESIAN_POINT('Ctrl Pts',(28.47375454572,0.1213442499766,-1.154513410291));
#17712=CARTESIAN_POINT('Ctrl Pts',(28.42500454572,-0.6322566409435,-0.9735898426565));
#17713=CARTESIAN_POINT('Ctrl Pts',(28.37625454572,-1.104055620977,-0.3587294269414));
#17714=CARTESIAN_POINT('Ctrl Pts',(28.32750454572,-1.083768164943,0.4160196237967));
#17715=CARTESIAN_POINT('Ctrl Pts',(28.27875454572,-0.5804362163164,1.005345248755));
#17716=CARTESIAN_POINT('Ctrl Pts',(28.23000454572,0.1815998427548,1.146580821045));
#17717=CARTESIAN_POINT('Ctrl Pts',(28.18125454572,0.8626991149286,0.7767743997426));
#17718=CARTESIAN_POINT('Ctrl Pts',(28.13250454572,1.159272503621,0.06075955192325));
#17719=CARTESIAN_POINT('Ctrl Pts',(28.08375454572,0.9392007235413,-0.6823594484165));
#17720=CARTESIAN_POINT('Ctrl Pts',(28.03500454572,0.300325716294,-1.121259010771));
#17721=CARTESIAN_POINT('Ctrl Pts',(28.00250454572,-0.2143469768198,-1.080904021891));
#17722=CARTESIAN_POINT('Ctrl Pts',(27.98625454572,-0.4370945424777,-0.9817304160776));
#17723=CARTESIAN_POINT('Ctrl Pts',(29.48463710284,0.5689250970851,0.7830582177302));
#17724=CARTESIAN_POINT('Ctrl Pts',(29.46838710284,0.7465953708295,0.6539732078924));
#17725=CARTESIAN_POINT('Ctrl Pts',(29.43588710284,1.00985274314,0.2706925630537));
#17726=CARTESIAN_POINT('Ctrl Pts',(29.38713710284,0.9552164149722,-0.4252975810125));
#17727=CARTESIAN_POINT('Ctrl Pts',(29.33838710284,0.4746777717184,-0.9316168029278));
#17728=CARTESIAN_POINT('Ctrl Pts',(29.28963710284,-0.2173871517845,-1.022736996495));
#17729=CARTESIAN_POINT('Ctrl Pts',(29.24088710284,-0.812571968791,-0.6580069832544));
#17730=CARTESIAN_POINT('Ctrl Pts',(29.19213710284,-1.045583921078,-1.042734842915E-7));
#17731=CARTESIAN_POINT('Ctrl Pts',(29.14338710284,-0.8125714716224,0.6580074003485));
#17732=CARTESIAN_POINT('Ctrl Pts',(29.09463710284,-0.2173891404584,1.022735536666));
#17733=CARTESIAN_POINT('Ctrl Pts',(29.04588710284,0.4746852292457,0.9316222251505));
#17734=CARTESIAN_POINT('Ctrl Pts',(28.99713710284,0.9551885735371,0.4252773519507));
#17735=CARTESIAN_POINT('Ctrl Pts',(28.94838710284,1.009956651354,-0.2706170690297));
#17736=CARTESIAN_POINT('Ctrl Pts',(28.89963710284,0.614578893256,-0.8458952773463));
#17737=CARTESIAN_POINT('Ctrl Pts',(28.85088710284,-0.0547216418674,-1.044151127966));
#17738=CARTESIAN_POINT('Ctrl Pts',(28.80213710284,-0.69963229914,-0.7770203872106));
#17739=CARTESIAN_POINT('Ctrl Pts',(28.75338710284,-1.032711189717,-0.1635653837992));
#17740=CARTESIAN_POINT('Ctrl Pts',(28.70463710284,-0.9055023617337,0.5227920322988));
#17741=CARTESIAN_POINT('Ctrl Pts',(28.65588710284,-0.3747038173085,0.9761368169669));
#17742=CARTESIAN_POINT('Ctrl Pts',(28.60713710284,0.3231032450129,0.9944095379687));
#17743=CARTESIAN_POINT('Ctrl Pts',(28.55838710284,0.8769005812753,0.569465895977));
#17744=CARTESIAN_POINT('Ctrl Pts',(28.50963710284,1.039856245751,-0.1092932955163));
#17745=CARTESIAN_POINT('Ctrl Pts',(28.46088710284,0.7393395821542,-0.7393395822784));
#17746=CARTESIAN_POINT('Ctrl Pts',(28.41213710284,0.109293296325,-1.039856246063));
#17747=CARTESIAN_POINT('Ctrl Pts',(28.36338710284,-0.5694658990877,-0.8769005799032));
#17748=CARTESIAN_POINT('Ctrl Pts',(28.31463710284,-0.994409526335,-0.323103250189));
#17749=CARTESIAN_POINT('Ctrl Pts',(28.26588710284,-0.9761368603912,0.3747038366413));
#17750=CARTESIAN_POINT('Ctrl Pts',(28.21713710284,-0.5227918702355,0.905502289579));
#17751=CARTESIAN_POINT('Ctrl Pts',(28.16838710284,0.1635647789705,1.032711459003));
#17752=CARTESIAN_POINT('Ctrl Pts',(28.11963710284,0.7770226444627,0.6996312941492));
#17753=CARTESIAN_POINT('Ctrl Pts',(28.07088710284,1.044142703787,0.05472539254393));
#17754=CARTESIAN_POINT('Ctrl Pts',(28.02213710284,0.845926716811,-0.6145928909717));
#17755=CARTESIAN_POINT('Ctrl Pts',(27.97338710284,0.27049973535,-1.009904411168));
#17756=CARTESIAN_POINT('Ctrl Pts',(27.94088710284,-0.1930597260145,-0.9735571614325));
#17757=CARTESIAN_POINT('Ctrl Pts',(27.92463710284,-0.393685760654,-0.8842326957913));
#17758=CARTESIAN_POINT('',(27.9766265322859,2.05983980323309E-10,-1.00599991871459));
#17759=CARTESIAN_POINT('Ctrl Pts',(29.4766395048596,0.870773402089107,0.502739671065568));
#17760=CARTESIAN_POINT('Ctrl Pts',(29.4691052524585,0.923830175985616,0.411176324318506));
#17761=CARTESIAN_POINT('Ctrl Pts',(29.4603459013364,0.972239735087807,0.295767810922782));
#17762=CARTESIAN_POINT('Ctrl Pts',(29.4413683829903,1.01254518840659,0.0325064994309846));
#17763=CARTESIAN_POINT('Ctrl Pts',(29.4325422909147,1.00848954053169,-0.0936168937763489));
#17764=CARTESIAN_POINT('Ctrl Pts',(29.4142572992227,0.954288507126751,-0.344674989241598));
#17765=CARTESIAN_POINT('Ctrl Pts',(29.4050118930799,0.901467497815252,-0.465863888580647));
#17766=CARTESIAN_POINT('Ctrl Pts',(29.3863010258111,0.750666938273149,-0.681074536322047));
#17767=CARTESIAN_POINT('Ctrl Pts',(29.3770681843844,0.655791268906749,-0.773156797467866));
#17768=CARTESIAN_POINT('Ctrl Pts',(29.3568701808035,0.418327990956232,-0.928000835580218));
#17769=CARTESIAN_POINT('Ctrl Pts',(29.3475047473003,0.290445664438423,-0.968960876829257));
#17770=CARTESIAN_POINT('Ctrl Pts',(29.3306589696046,0.0575864727316964,
-1.01153056273425));
#17771=CARTESIAN_POINT('Ctrl Pts',(29.3216600150564,-0.0710782558689575,
-1.01133291870579));
#17772=CARTESIAN_POINT('Ctrl Pts',(29.3025520369029,-0.33408320271347,-0.959511029806047));
#17773=CARTESIAN_POINT('Ctrl Pts',(29.2930478380111,-0.458249759673364,
-0.903490004899866));
#17774=CARTESIAN_POINT('Ctrl Pts',(29.2764607849825,-0.651606739985256,
-0.773324037322229));
#17775=CARTESIAN_POINT('Ctrl Pts',(29.2672741424586,-0.750738679733299,
-0.686734029266918));
#17776=CARTESIAN_POINT('Ctrl Pts',(29.2471250024667,-0.908027886469006,
-0.451749616134813));
#17777=CARTESIAN_POINT('Ctrl Pts',(29.237713668734,-0.95964855352592,-0.327158651203346));
#17778=CARTESIAN_POINT('Ctrl Pts',(29.2188206192439,-1.01247717924914,-0.0671105513275875));
#17779=CARTESIAN_POINT('Ctrl Pts',(29.2095672963116,-1.01261280867459,0.0652074783840267));
#17780=CARTESIAN_POINT('Ctrl Pts',(29.190863687752,-0.960786276316742,0.322740178671316));
#17781=CARTESIAN_POINT('Ctrl Pts',(29.1816445339917,-0.910941399638776,
0.444975024007311));
#17782=CARTESIAN_POINT('Ctrl Pts',(29.1614385161677,-0.755567145070654,
0.682208090561074));
#17783=CARTESIAN_POINT('Ctrl Pts',(29.1520598052671,-0.654636111382696,
0.771092380231491));
#17784=CARTESIAN_POINT('Ctrl Pts',(29.1352540053897,-0.458920417080214,
0.903256265996071));
#17785=CARTESIAN_POINT('Ctrl Pts',(29.126269951113,-0.341225419004554,0.954680725569352));
#17786=CARTESIAN_POINT('Ctrl Pts',(29.1077447657715,-0.0875413822859973,
1.01111645447045));
#17787=CARTESIAN_POINT('Ctrl Pts',(29.0982393193791,0.0486169665866859,
1.01287742140832));
#17788=CARTESIAN_POINT('Ctrl Pts',(29.08105524586,0.286247499755392,0.969965709350147));
#17789=CARTESIAN_POINT('Ctrl Pts',(29.0718646719204,0.411828409927529,0.930377288092367));
#17790=CARTESIAN_POINT('Ctrl Pts',(29.0517249713864,0.650119117375458,0.778369367719768));
#17791=CARTESIAN_POINT('Ctrl Pts',(29.0423217182129,0.747374114001147,0.685109299358994));
#17792=CARTESIAN_POINT('Ctrl Pts',(29.023422352595,0.900301395997063,0.468151058055233));
#17793=CARTESIAN_POINT('Ctrl Pts',(29.0141578837073,0.95356617334133,0.346849748046551));
#17794=CARTESIAN_POINT('Ctrl Pts',(28.9954668431443,1.00948095071544,0.0903434934989169));
#17795=CARTESIAN_POINT('Ctrl Pts',(28.9862599642793,1.01296598826026,-0.0414324395852936));
#17796=CARTESIAN_POINT('Ctrl Pts',(28.966042999187,0.966019492682187,-0.321250069431303));
#17797=CARTESIAN_POINT('Ctrl Pts',(28.956650771909,0.909104926108195,-0.443337235931549));
#17798=CARTESIAN_POINT('Ctrl Pts',(28.9398838938874,0.783304765554662,-0.642559988636239));
#17799=CARTESIAN_POINT('Ctrl Pts',(28.9309137064795,0.696376860255623,-0.736824922057775));
#17800=CARTESIAN_POINT('Ctrl Pts',(28.9124152715538,0.487117299376328,-0.890303235238159));
#17801=CARTESIAN_POINT('Ctrl Pts',(28.9029118555964,0.363230754563954,-0.94676231466883));
#17802=CARTESIAN_POINT('Ctrl Pts',(28.8856873106528,0.127880192190271,-1.00327016540539));
#17803=CARTESIAN_POINT('Ctrl Pts',(28.876493100702,-0.00307419136588492,
-1.01744177706707));
#17804=CARTESIAN_POINT('Ctrl Pts',(28.8563616071713,-0.282263576240707,
-0.97404838799872));
#17805=CARTESIAN_POINT('Ctrl Pts',(28.846965929091,-0.408717770745884,-0.927836026440969));
#17806=CARTESIAN_POINT('Ctrl Pts',(28.8280621443433,-0.636054869835307,
-0.79071040527693));
#17807=CARTESIAN_POINT('Ctrl Pts',(28.8187862830508,-0.733676604436161,
-0.700904969244608));
#17808=CARTESIAN_POINT('Ctrl Pts',(28.800107804091,-0.887904373733199,-0.488659821461714));
#17809=CARTESIAN_POINT('Ctrl Pts',(28.7909121905271,-0.944048573936193,
-0.369579698988377));
#17810=CARTESIAN_POINT('Ctrl Pts',(28.7706842229678,-1.01369908580114,-0.0943832969988919));
#17811=CARTESIAN_POINT('Ctrl Pts',(28.761279437479,-1.01058265066987,0.0404795504745535));
#17812=CARTESIAN_POINT('Ctrl Pts',(28.7445489336977,-0.975656602098983,
0.272979304096127));
#17813=CARTESIAN_POINT('Ctrl Pts',(28.7355913796315,-0.934104160209119,
0.394084134956389));
#17814=CARTESIAN_POINT('Ctrl Pts',(28.7176616890085,-0.808338952205141,
0.611915865043623));
#17815=CARTESIAN_POINT('Ctrl Pts',(28.7087041349353,-0.724235313104034,
0.708453750739594));
#17816=CARTESIAN_POINT('Ctrl Pts',(28.6919736311539,-0.540347644379399,
0.854950472866602));
#17817=CARTESIAN_POINT('Ctrl Pts',(28.6825688456651,-0.425111210006108,
0.925080808596303));
#17818=CARTESIAN_POINT('Ctrl Pts',(28.6623408781058,-0.151958878920123,
1.00235989692945));
#17819=CARTESIAN_POINT('Ctrl Pts',(28.653145264542,-0.0207603676706871,
1.01327765451514));
#17820=CARTESIAN_POINT('Ctrl Pts',(28.6344667855823,0.240163206787947,0.985835062226095));
#17821=CARTESIAN_POINT('Ctrl Pts',(28.6251909242898,0.366747863090091,0.946194878116322));
#17822=CARTESIAN_POINT('Ctrl Pts',(28.6062871395422,0.599170684072242,0.817877985664108));
#17823=CARTESIAN_POINT('Ctrl Pts',(28.5968914614618,0.702418860402553,0.731471621586352));
#17824=CARTESIAN_POINT('Ctrl Pts',(28.5767599679311,0.879593330129096,0.511383216351974));
#17825=CARTESIAN_POINT('Ctrl Pts',(28.5675657579803,0.93279754619543,0.3908875876246));
#17826=CARTESIAN_POINT('Ctrl Pts',(28.5503412130367,1.00153559313095,0.158814096445722));
#17827=CARTESIAN_POINT('Ctrl Pts',(28.5408377970793,1.01458386847578,0.023295661735716));
#17828=CARTESIAN_POINT('Ctrl Pts',(28.5223393621534,0.986297530771063,-0.234667590561126));
#17829=CARTESIAN_POINT('Ctrl Pts',(28.5133691747455,0.948125656391323,-0.35708183155897));
#17830=CARTESIAN_POINT('Ctrl Pts',(28.4966022967238,0.838493771813713,-0.565639342750806));
#17831=CARTESIAN_POINT('Ctrl Pts',(28.4872100694457,0.761220467435563,-0.675972386498998));
#17832=CARTESIAN_POINT('Ctrl Pts',(28.4669931043534,0.542364539351682,-0.856538059210502));
#17833=CARTESIAN_POINT('Ctrl Pts',(28.4577862254884,0.426500714921235,-0.919407894705339));
#17834=CARTESIAN_POINT('Ctrl Pts',(28.4390951849256,0.176402393566531,-0.99923740432608));
#17835=CARTESIAN_POINT('Ctrl Pts',(28.4298307160378,0.0447199889143125,
-1.01375940902338));
#17836=CARTESIAN_POINT('Ctrl Pts',(28.41093135042,-0.219635000613468,-0.989799618535087));
#17837=CARTESIAN_POINT('Ctrl Pts',(28.4015280972466,-0.349028087285628,
-0.952204354992616));
#17838=CARTESIAN_POINT('Ctrl Pts',(28.3813883967126,-0.599816161628727,
-0.821842509043117));
#17839=CARTESIAN_POINT('Ctrl Pts',(28.3721978227729,-0.696891195219636,
-0.732880461232601));
#17840=CARTESIAN_POINT('Ctrl Pts',(28.3550137492539,-0.85286909456606,-0.548542238822846));
#17841=CARTESIAN_POINT('Ctrl Pts',(28.3455083028614,-0.919423226898893,
-0.429745166292879));
#17842=CARTESIAN_POINT('Ctrl Pts',(28.3269831175199,-0.997390470348598,
-0.181830481509578));
#17843=CARTESIAN_POINT('Ctrl Pts',(28.3179990632432,-1.01170308102003,-0.0541913934911062));
#17844=CARTESIAN_POINT('Ctrl Pts',(28.3011932633659,-0.995103645636229,
0.181385312576479));
#17845=CARTESIAN_POINT('Ctrl Pts',(28.2918145524652,-0.968593109628239,
0.313236296615798));
#17846=CARTESIAN_POINT('Ctrl Pts',(28.2716085346412,-0.840830374658889,
0.566410881442955));
#17847=CARTESIAN_POINT('Ctrl Pts',(28.262389380881,-0.759894331709147,0.670695233562651));
#17848=CARTESIAN_POINT('Ctrl Pts',(28.2436857723214,-0.562777737133921,
0.844344677318258));
#17849=CARTESIAN_POINT('Ctrl Pts',(28.2344324493892,-0.448119147312191,
0.910386233646076));
#17850=CARTESIAN_POINT('Ctrl Pts',(28.2155393998992,-0.196496573752333,
0.994659351660514));
#17851=CARTESIAN_POINT('Ctrl Pts',(28.2061280661666,-0.0627872995112383,
1.01225002509461));
#17852=CARTESIAN_POINT('Ctrl Pts',(28.1859789261748,0.21935977512202,0.993525782886269));
#17853=CARTESIAN_POINT('Ctrl Pts',(28.1767922836509,0.343914891685563,0.95097000876569));
#17854=CARTESIAN_POINT('Ctrl Pts',(28.1602052306222,0.553320416471885,0.848600935605246));
#17855=CARTESIAN_POINT('Ctrl Pts',(28.1507010317303,0.663919325666453,0.769080055430514));
#17856=CARTESIAN_POINT('Ctrl Pts',(28.1315930535768,0.840300871347782,0.567222034592242));
#17857=CARTESIAN_POINT('Ctrl Pts',(28.1225940990285,0.904804400397695,0.455893933067178));
#17858=CARTESIAN_POINT('Ctrl Pts',(28.1057483213327,0.98436756682625,0.232947114591715));
#17859=CARTESIAN_POINT('Ctrl Pts',(28.0963828878294,1.01283629382343,0.101717750507575));
#17860=CARTESIAN_POINT('Ctrl Pts',(28.0761848842484,0.997469062168753,-0.181353499720004));
#17861=CARTESIAN_POINT('Ctrl Pts',(28.0669520428217,0.965161319461699,-0.309559370165432));
#17862=CARTESIAN_POINT('Ctrl Pts',(28.048241175553,0.854183711123641,-0.54776180950454));
#17863=CARTESIAN_POINT('Ctrl Pts',(28.0389957694103,0.775641550295079,-0.65410059509126));
#17864=CARTESIAN_POINT('Ctrl Pts',(28.0207108054875,0.585319667539776,-0.826568852737046));
#17865=CARTESIAN_POINT('Ctrl Pts',(28.0118847412308,0.4781218150517,-0.893142685975639));
#17866=CARTESIAN_POINT('Ctrl Pts',(27.9929072063119,0.229977999238873,-0.989868172118325));
#17867=CARTESIAN_POINT('Ctrl Pts',(27.9841478270495,0.105826098472935,-1.00564856987941));
#17868=CARTESIAN_POINT('Ctrl Pts',(27.9766135594424,1.31358039184295E-6,
-1.00548172258563));
#17869=CARTESIAN_POINT('',(28.1175,-3.956254470204E-14,-1.25));
#17870=CARTESIAN_POINT('Ctrl Pts',(28.16948943148,0.523912106125,-1.17672585665));
#17871=CARTESIAN_POINT('Ctrl Pts',(28.15323943148,0.2569214784303,-1.295597742809));
#17872=CARTESIAN_POINT('Ctrl Pts',(28.12073943148,-0.359977678182,-1.343968209978));
#17873=CARTESIAN_POINT('Ctrl Pts',(28.07198943148,-1.125748737002,-0.8178925633062));
#17874=CARTESIAN_POINT('Ctrl Pts',(28.02323943148,-1.389532103288,0.07282787068199));
#17875=CARTESIAN_POINT('Ctrl Pts',(27.97448943148,-1.034052055861,0.9310606109295));
#17876=CARTESIAN_POINT('Ctrl Pts',(27.92573943148,-0.2176699703233,1.374319545129));
#17877=CARTESIAN_POINT('Ctrl Pts',(27.87698943148,0.6957249084783,1.205031167107));
#17878=CARTESIAN_POINT('Ctrl Pts',(27.82823943148,1.299030774048,0.4986511981072));
#17879=CARTESIAN_POINT('Ctrl Pts',(27.77948943148,1.323347810262,-0.4299817804464));
#17880=CARTESIAN_POINT('Ctrl Pts',(27.73073943148,0.757838124655,-1.166968368163));
#17881=CARTESIAN_POINT('Ctrl Pts',(27.68198943148,-0.1454461572801,-1.383827738746));
#17882=CARTESIAN_POINT('Ctrl Pts',(27.63323943148,-0.9839039059594,-0.9839039061246));
#17883=CARTESIAN_POINT('Ctrl Pts',(27.58448943148,-1.383827738331,-0.1454461562038));
#17884=CARTESIAN_POINT('Ctrl Pts',(27.53573943148,-1.166968369989,0.7578381205156));
#17885=CARTESIAN_POINT('Ctrl Pts',(27.48698943148,-0.4299817735579,1.323347825744));
#17886=CARTESIAN_POINT('Ctrl Pts',(27.43823943148,0.4986511723796,1.299030716259));
#17887=CARTESIAN_POINT('Ctrl Pts',(27.38948943148,1.20503126313,0.6957251241499));
#17888=CARTESIAN_POINT('Ctrl Pts',(27.34073943148,1.374319186766,-0.2176707752221));
#17889=CARTESIAN_POINT('Ctrl Pts',(27.29198943148,0.9310619483586,-1.034049051938));
#17890=CARTESIAN_POINT('Ctrl Pts',(27.24323943148,0.0728228793282,-1.389543314081));
#17891=CARTESIAN_POINT('Ctrl Pts',(27.19448943148,-0.8178739353207,-1.125706897754));
#17892=CARTESIAN_POINT('Ctrl Pts',(27.14573943148,-1.344037730566,-0.3601338243812));
#17893=CARTESIAN_POINT('Ctrl Pts',(27.09698943148,-1.271153054855,0.5659538022856));
#17894=CARTESIAN_POINT('Ctrl Pts',(27.04823943148,-0.6317051899144,1.239791251989));
#17895=CARTESIAN_POINT('Ctrl Pts',(26.99948943148,0.2892987601003,1.361043711953));
#17896=CARTESIAN_POINT('Ctrl Pts',(26.95073943148,1.081359992212,0.8756680515693));
#17897=CARTESIAN_POINT('Ctrl Pts',(26.90198943148,1.391450057306,-1.387659428753E-7));
#17898=CARTESIAN_POINT('Ctrl Pts',(26.85323943148,1.081360653838,-0.8756674965058));
#17899=CARTESIAN_POINT('Ctrl Pts',(26.80448943148,0.2892961135976,-1.361045654676));
#17900=CARTESIAN_POINT('Ctrl Pts',(26.75573943148,-0.6316952655301,-1.239784036163));
#17901=CARTESIAN_POINT('Ctrl Pts',(26.70698943148,-1.271190105891,-0.5659807228688));
#17902=CARTESIAN_POINT('Ctrl Pts',(26.65823943148,-1.34389945081,0.360234290888));
#17903=CARTESIAN_POINT('Ctrl Pts',(26.62573943148,-0.9935598191429,0.8702993985029));
#17904=CARTESIAN_POINT('Ctrl Pts',(26.60948943148,-0.7571184320867,1.04208412158));
#17905=CARTESIAN_POINT('Ctrl Pts',(28.1078719886,0.4805033243013,-1.079228136364));
#17906=CARTESIAN_POINT('Ctrl Pts',(28.0916219886,0.235634227625,-1.18825088235));
#17907=CARTESIAN_POINT('Ctrl Pts',(28.0591219886,-0.330151697238,-1.232613610374));
#17908=CARTESIAN_POINT('Ctrl Pts',(28.0103719886,-1.032474730272,-0.7501260058613));
#17909=CARTESIAN_POINT('Ctrl Pts',(27.9616219886,-1.274402303455,0.06679371130266));
#17910=CARTESIAN_POINT('Ctrl Pts',(27.9128719886,-0.9483755853946,0.8539175053361));
#17911=CARTESIAN_POINT('Ctrl Pts',(27.8641219886,-0.199634906539,1.260450183087));
#17912=CARTESIAN_POINT('Ctrl Pts',(27.8153719886,0.6380805623974,1.105188207931));
#17913=CARTESIAN_POINT('Ctrl Pts',(27.7666219886,1.191399469495,0.4573354109519));
#17914=CARTESIAN_POINT('Ctrl Pts',(27.7178719886,1.21370171562,-0.394355603694));
#17915=CARTESIAN_POINT('Ctrl Pts',(27.6691219886,0.6950473827992,-1.07027910541));
#17916=CARTESIAN_POINT('Ctrl Pts',(27.6203719886,-0.1333952036284,-1.269170574518));
#17917=CARTESIAN_POINT('Ctrl Pts',(27.5716219886,-0.902382464691,-0.9023824648425));
#17918=CARTESIAN_POINT('Ctrl Pts',(27.5228719886,-1.269170574137,-0.1333952026413));
#17919=CARTESIAN_POINT('Ctrl Pts',(27.4741219886,-1.070279107084,0.6950473790028));
#17920=CARTESIAN_POINT('Ctrl Pts',(27.4253719886,-0.3943555973762,1.213701729819));
#17921=CARTESIAN_POINT('Ctrl Pts',(27.3766219886,0.4573353873559,1.191399416495));
#17922=CARTESIAN_POINT('Ctrl Pts',(27.3278719886,1.105188295998,0.6380807601996));
#17923=CARTESIAN_POINT('Ctrl Pts',(27.2791219886,1.260449854417,-0.1996356447478));
#17924=CARTESIAN_POINT('Ctrl Pts',(27.2303719886,0.8539187319524,-0.9483728303621));
#17925=CARTESIAN_POINT('Ctrl Pts',(27.1816219886,0.06678913350791,-1.274412585376));
#17926=CARTESIAN_POINT('Ctrl Pts',(27.1328719886,-0.7501089212991,-1.032436357618));
#17927=CARTESIAN_POINT('Ctrl Pts',(27.0841219886,-1.232677370829,-0.3302949059307));
#17928=CARTESIAN_POINT('Ctrl Pts',(27.0353719886,-1.165831561083,0.519061652174));
#17929=CARTESIAN_POINT('Ctrl Pts',(26.9866219886,-0.5793652030248,1.137068243043));
#17930=CARTESIAN_POINT('Ctrl Pts',(26.9378719886,0.2653288868863,1.248274320191));
#17931=CARTESIAN_POINT('Ctrl Pts',(26.8891219886,0.9917638186823,0.8031145011623));
#17932=CARTESIAN_POINT('Ctrl Pts',(26.8403719886,1.27616134523,-1.272684787665E-7));
#17933=CARTESIAN_POINT('Ctrl Pts',(26.7916219886,0.9917644254889,-0.8031139920887));
#17934=CARTESIAN_POINT('Ctrl Pts',(26.7428719886,0.2653264596599,-1.248276101949));
#17935=CARTESIAN_POINT('Ctrl Pts',(26.6941219886,-0.5793561009262,-1.137061625084));
#17936=CARTESIAN_POINT('Ctrl Pts',(26.6453719886,-1.165865542251,-0.51908634225));
#17937=CARTESIAN_POINT('Ctrl Pts',(26.5966219886,-1.232550548254,0.3303870482766));
#17938=CARTESIAN_POINT('Ctrl Pts',(26.5641219886,-0.9112383363717,0.7981906682994));
#17939=CARTESIAN_POINT('Ctrl Pts',(26.5478719886,-0.6943873204195,0.9557421536299));
#17940=CARTESIAN_POINT('Ctrl Pts',(28.04625454572,0.4370945424776,-0.9817304160777));
#17941=CARTESIAN_POINT('Ctrl Pts',(28.03000454572,0.2143469768197,-1.080904021891));
#17942=CARTESIAN_POINT('Ctrl Pts',(27.99750454572,-0.3003257162941,-1.121259010771));
#17943=CARTESIAN_POINT('Ctrl Pts',(27.94875454572,-0.9392007235413,-0.6823594484165));
#17944=CARTESIAN_POINT('Ctrl Pts',(27.90000454572,-1.159272503621,0.06075955192333));
#17945=CARTESIAN_POINT('Ctrl Pts',(27.85125454572,-0.8626991149286,0.7767743997427));
#17946=CARTESIAN_POINT('Ctrl Pts',(27.80250454572,-0.1815998427547,1.146580821045));
#17947=CARTESIAN_POINT('Ctrl Pts',(27.75375454572,0.5804362163165,1.005345248755));
#17948=CARTESIAN_POINT('Ctrl Pts',(27.70500454572,1.083768164943,0.4160196237966));
#17949=CARTESIAN_POINT('Ctrl Pts',(27.65625454572,1.104055620977,-0.3587294269415));
#17950=CARTESIAN_POINT('Ctrl Pts',(27.60750454572,0.6322566409434,-0.9735898426565));
#17951=CARTESIAN_POINT('Ctrl Pts',(27.55875454572,-0.1213442499767,-1.154513410291));
#17952=CARTESIAN_POINT('Ctrl Pts',(27.51000454572,-0.8208610234226,-0.8208610235604));
#17953=CARTESIAN_POINT('Ctrl Pts',(27.46125454572,-1.154513409944,-0.1213442490788));
#17954=CARTESIAN_POINT('Ctrl Pts',(27.41250454572,-0.9735898441798,0.6322566374899));
#17955=CARTESIAN_POINT('Ctrl Pts',(27.36375454572,-0.3587294211945,1.104055633894));
#17956=CARTESIAN_POINT('Ctrl Pts',(27.31500454572,0.4160196023323,1.083768116731));
#17957=CARTESIAN_POINT('Ctrl Pts',(27.26625454572,1.005345328866,0.5804363962492));
#17958=CARTESIAN_POINT('Ctrl Pts',(27.21750454572,1.146580522067,-0.1816005142735));
#17959=CARTESIAN_POINT('Ctrl Pts',(27.16875454572,0.7767755155462,-0.8626966087864));
#17960=CARTESIAN_POINT('Ctrl Pts',(27.12000454572,0.06075538768762,-1.159281856671));
#17961=CARTESIAN_POINT('Ctrl Pts',(27.07125454572,-0.6823439072776,-0.9391658174821));
#17962=CARTESIAN_POINT('Ctrl Pts',(27.02250454572,-1.121317011091,-0.3004559874802));
#17963=CARTESIAN_POINT('Ctrl Pts',(26.97375454572,-1.06051006731,0.4721695020624));
#17964=CARTESIAN_POINT('Ctrl Pts',(26.92500454572,-0.5270252161352,1.034345234097));
#17965=CARTESIAN_POINT('Ctrl Pts',(26.87625454572,0.2413590136724,1.135504928428));
#17966=CARTESIAN_POINT('Ctrl Pts',(26.82750454572,0.9021676451524,0.7305609507554));
#17967=CARTESIAN_POINT('Ctrl Pts',(26.77875454572,1.160872633154,-1.157710151699E-7));
#17968=CARTESIAN_POINT('Ctrl Pts',(26.73000454572,0.9021681971399,-0.7305604876716));
#17969=CARTESIAN_POINT('Ctrl Pts',(26.68125454572,0.2413568057222,-1.135506549222));
#17970=CARTESIAN_POINT('Ctrl Pts',(26.63250454572,-0.5270169363223,-1.034339214006));
#17971=CARTESIAN_POINT('Ctrl Pts',(26.58375454572,-1.060540978612,-0.4721919616312));
#17972=CARTESIAN_POINT('Ctrl Pts',(26.53500454572,-1.121201645697,0.3005398056652));
#17973=CARTESIAN_POINT('Ctrl Pts',(26.50250454572,-0.8289168536006,0.726081938096));
#17974=CARTESIAN_POINT('Ctrl Pts',(26.48625454572,-0.6316562087523,0.86940018568));
#17975=CARTESIAN_POINT('Ctrl Pts',(27.98463710284,0.3936857606539,-0.8842326957913));
#17976=CARTESIAN_POINT('Ctrl Pts',(27.96838710284,0.1930597260145,-0.9735571614325));
#17977=CARTESIAN_POINT('Ctrl Pts',(27.93588710284,-0.2704997353501,-1.009904411168));
#17978=CARTESIAN_POINT('Ctrl Pts',(27.88713710284,-0.845926716811,-0.6145928909716));
#17979=CARTESIAN_POINT('Ctrl Pts',(27.83838710284,-1.044142703787,0.054725392544));
#17980=CARTESIAN_POINT('Ctrl Pts',(27.78963710284,-0.7770226444626,0.6996312941493));
#17981=CARTESIAN_POINT('Ctrl Pts',(27.74088710284,-0.1635647789704,1.032711459003));
#17982=CARTESIAN_POINT('Ctrl Pts',(27.69213710284,0.5227918702356,0.9055022895789));
#17983=CARTESIAN_POINT('Ctrl Pts',(27.64338710284,0.9761368603912,0.3747038366413));
#17984=CARTESIAN_POINT('Ctrl Pts',(27.59463710284,0.9944095263349,-0.3231032501891));
#17985=CARTESIAN_POINT('Ctrl Pts',(27.54588710284,0.5694658990876,-0.8769005799033));
#17986=CARTESIAN_POINT('Ctrl Pts',(27.49713710284,-0.109293296325,-1.039856246063));
#17987=CARTESIAN_POINT('Ctrl Pts',(27.44838710284,-0.7393395821542,-0.7393395822784));
#17988=CARTESIAN_POINT('Ctrl Pts',(27.39963710284,-1.039856245751,-0.1092932955163));
#17989=CARTESIAN_POINT('Ctrl Pts',(27.35088710284,-0.8769005812753,0.5694658959771));
#17990=CARTESIAN_POINT('Ctrl Pts',(27.30213710284,-0.3231032450128,0.9944095379687));
#17991=CARTESIAN_POINT('Ctrl Pts',(27.25338710284,0.3747038173086,0.9761368169669));
#17992=CARTESIAN_POINT('Ctrl Pts',(27.20463710284,0.9055023617338,0.5227920322988));
#17993=CARTESIAN_POINT('Ctrl Pts',(27.15588710284,1.032711189717,-0.1635653837993));
#17994=CARTESIAN_POINT('Ctrl Pts',(27.10713710284,0.69963229914,-0.7770203872107));
#17995=CARTESIAN_POINT('Ctrl Pts',(27.05838710284,0.05472164186733,-1.044151127966));
#17996=CARTESIAN_POINT('Ctrl Pts',(27.00963710284,-0.6145788932561,-0.8458952773462));
#17997=CARTESIAN_POINT('Ctrl Pts',(26.96088710284,-1.009956651354,-0.2706170690297));
#17998=CARTESIAN_POINT('Ctrl Pts',(26.91213710284,-0.9551885735371,0.4252773519508));
#17999=CARTESIAN_POINT('Ctrl Pts',(26.86338710284,-0.4746852292456,0.9316222251505));
#18000=CARTESIAN_POINT('Ctrl Pts',(26.81463710284,0.2173891404585,1.022735536666));
#18001=CARTESIAN_POINT('Ctrl Pts',(26.76588710284,0.8125714716225,0.6580074003485));
#18002=CARTESIAN_POINT('Ctrl Pts',(26.71713710284,1.045583921078,-1.042735511825E-7));
#18003=CARTESIAN_POINT('Ctrl Pts',(26.66838710284,0.8125719687909,-0.6580069832545));
#18004=CARTESIAN_POINT('Ctrl Pts',(26.61963710284,0.2173871517845,-1.022736996495));
#18005=CARTESIAN_POINT('Ctrl Pts',(26.57088710284,-0.4746777717184,-0.9316168029278));
#18006=CARTESIAN_POINT('Ctrl Pts',(26.52213710284,-0.9552164149723,-0.4252975810124));
#18007=CARTESIAN_POINT('Ctrl Pts',(26.47338710284,-1.00985274314,0.2706925630538));
#18008=CARTESIAN_POINT('Ctrl Pts',(26.44088710284,-0.7465953708295,0.6539732078925));
#18009=CARTESIAN_POINT('Ctrl Pts',(26.42463710284,-0.568925097085,0.7830582177302));
#18010=CARTESIAN_POINT('',(26.4799708243305,-0.893567698107012,0.46113007932394));
#18011=CARTESIAN_POINT('Ctrl Pts',(27.9766422174339,-1.5373237190809E-6,
-1.00548643891288));
#18012=CARTESIAN_POINT('Ctrl Pts',(27.9705255346309,-0.0859077806927734,
-1.00562089711478));
#18013=CARTESIAN_POINT('Ctrl Pts',(27.9644038376714,-0.171834166064752,
-0.994932640726613));
#18014=CARTESIAN_POINT('Ctrl Pts',(27.9521313122326,-0.338307248628255,
-0.951321255208717));
#18015=CARTESIAN_POINT('Ctrl Pts',(27.9459996491108,-0.41859324830683,-0.918352377669841));
#18016=CARTESIAN_POINT('Ctrl Pts',(27.9308010923912,-0.604507474757968,
-0.813185183941887));
#18017=CARTESIAN_POINT('Ctrl Pts',(27.9217162790432,-0.70401704675962,-0.729489940877468));
#18018=CARTESIAN_POINT('Ctrl Pts',(27.9004547199262,-0.891186104950947,
-0.497397527776343));
#18019=CARTESIAN_POINT('Ctrl Pts',(27.8906214013537,-0.941335991090675,
-0.364860551214267));
#18020=CARTESIAN_POINT('Ctrl Pts',(27.8766754648128,-0.995276073891188,
-0.176341402154162));
#18021=CARTESIAN_POINT('Ctrl Pts',(27.867508386247,-1.01642369245459,-0.0467042547600237));
#18022=CARTESIAN_POINT('Ctrl Pts',(27.8472694827219,-0.986706480683557,
0.235516124889919));
#18023=CARTESIAN_POINT('Ctrl Pts',(27.8378314007197,-0.946071719962327,
0.364715479070765));
#18024=CARTESIAN_POINT('Ctrl Pts',(27.8214313439974,-0.836161765852973,
0.567325413516962));
#18025=CARTESIAN_POINT('Ctrl Pts',(27.8119819791548,-0.760098085984591,
0.679268787558479));
#18026=CARTESIAN_POINT('Ctrl Pts',(27.7910321513064,-0.530789606151427,
0.863653013790982));
#18027=CARTESIAN_POINT('Ctrl Pts',(27.7817681502791,-0.413223717409633,
0.925788399292649));
#18028=CARTESIAN_POINT('Ctrl Pts',(27.7679188615263,-0.227184383092205,
0.982048937828046));
#18029=CARTESIAN_POINT('Ctrl Pts',(27.7633615602744,-0.164380263775081,
0.994628768871488));
#18030=CARTESIAN_POINT('Ctrl Pts',(27.7493060807227,0.0316682215204115,
1.01386448246957));
#18031=CARTESIAN_POINT('Ctrl Pts',(27.7398895019711,0.166239806421696,1.00019965980914));
#18032=CARTESIAN_POINT('Ctrl Pts',(27.722948630156,0.39422446910652,0.931294753093088));
#18033=CARTESIAN_POINT('Ctrl Pts',(27.7135806633062,0.516769776937294,0.87757223757841));
#18034=CARTESIAN_POINT('Ctrl Pts',(27.6930688620494,0.738867116514401,0.693970728769147));
#18035=CARTESIAN_POINT('Ctrl Pts',(27.6838346853022,0.823293763365346,0.5916217309268));
#18036=CARTESIAN_POINT('Ctrl Pts',(27.6699847101733,0.91597535503147,0.420829660664151));
#18037=CARTESIAN_POINT('Ctrl Pts',(27.6654152401922,0.940974162891107,0.361768629684782));
#18038=CARTESIAN_POINT('Ctrl Pts',(27.6513591638085,0.999311500696718,0.173674766097076));
#18039=CARTESIAN_POINT('Ctrl Pts',(27.6419654083536,1.01314003710848,0.039311455778221));
#18040=CARTESIAN_POINT('Ctrl Pts',(27.6231252836627,0.989400550382701,-0.22455377395045));
#18041=CARTESIAN_POINT('Ctrl Pts',(27.6138328999225,0.951988050045546,-0.351293863160414));
#18042=CARTESIAN_POINT('Ctrl Pts',(27.595128759979,0.828821871769212,-0.583495916260747));
#18043=CARTESIAN_POINT('Ctrl Pts',(27.5859242982163,0.745869543467991,-0.6866586081706));
#18044=CARTESIAN_POINT('Ctrl Pts',(27.5720731185926,0.597410474983936,-0.811959898152375));
#18045=CARTESIAN_POINT('Ctrl Pts',(27.5674917366428,0.544541205515937,-0.84839663720727));
#18046=CARTESIAN_POINT('Ctrl Pts',(27.5534388142855,0.372180503743955,-0.943469506501608));
#18047=CARTESIAN_POINT('Ctrl Pts',(27.5440688767006,0.243602562677523,-0.984185395931866));
#18048=CARTESIAN_POINT('Ctrl Pts',(27.5252181077583,-0.019790956493,-1.01445554834801));
#18049=CARTESIAN_POINT('Ctrl Pts',(27.5159060230867,-0.151558042053847,
-1.00333391119788));
#18050=CARTESIAN_POINT('Ctrl Pts',(27.4972207684037,-0.403699692496189,
-0.929699387128286));
#18051=CARTESIAN_POINT('Ctrl Pts',(27.4880454718056,-0.521279955364169,
-0.869530077180673));
#18052=CARTESIAN_POINT('Ctrl Pts',(27.4741927612439,-0.674040239658134,
-0.74960673165156));
#18053=CARTESIAN_POINT('Ctrl Pts',(27.4695997466732,-0.720459910529298,
-0.705142509973364));
#18054=CARTESIAN_POINT('Ctrl Pts',(27.4555529346347,-0.848377502645995,
-0.555681059924086));
#18055=CARTESIAN_POINT('Ctrl Pts',(27.4462074184943,-0.914262872089956,
-0.438238959868308));
#18056=CARTESIAN_POINT('Ctrl Pts',(27.4273501142183,-0.997461472283246,
-0.186370890415201));
#18057=CARTESIAN_POINT('Ctrl Pts',(27.418014468959,-1.01320279607384,-0.0549322312585341));
#18058=CARTESIAN_POINT('Ctrl Pts',(27.3993516905516,-0.992221655655208,
0.206690030888449));
#18059=CARTESIAN_POINT('Ctrl Pts',(27.3902046226188,-0.957291168985145,
0.333772807407334));
#18060=CARTESIAN_POINT('Ctrl Pts',(27.3763512181046,-0.870967954992039,
0.50764905831));
#18061=CARTESIAN_POINT('Ctrl Pts',(27.3717448653341,-0.836781532034192,
0.562196601259316));
#18062=CARTESIAN_POINT('Ctrl Pts',(27.3577073802788,-0.716486421177458,
0.71767212754246));
#18063=CARTESIAN_POINT('Ctrl Pts',(27.3483865423645,-0.615086538827653,
0.805957361969493));
#18064=CARTESIAN_POINT('Ctrl Pts',(27.3295286233357,-0.38542249522935,0.93874078967969));
#18065=CARTESIAN_POINT('Ctrl Pts',(27.3201620212027,-0.259667379149739,
0.980868466998606));
#18066=CARTESIAN_POINT('Ctrl Pts',(27.301526323939,0.000490033357717634,
1.01348106517059));
#18067=CARTESIAN_POINT('Ctrl Pts',(27.2924062511612,0.131755232397248,1.00521032755393));
#18068=CARTESIAN_POINT('Ctrl Pts',(27.2785538277661,0.319464250831635,0.95617772108636));
#18069=CARTESIAN_POINT('Ctrl Pts',(27.2739310443358,0.379954363604974,0.933743418142628));
#18070=CARTESIAN_POINT('Ctrl Pts',(27.2645824710877,0.497634642074296,0.876392064260345));
#18071=CARTESIAN_POINT('Ctrl Pts',(27.2598914483125,0.55413873606994,0.841549933535181));
#18072=CARTESIAN_POINT('Ctrl Pts',(27.2462803892375,0.707134147413743,0.725557967358108));
#18073=CARTESIAN_POINT('Ctrl Pts',(27.237362246922,0.793622219861324,0.630917404931592));
#18074=CARTESIAN_POINT('Ctrl Pts',(27.2238373535096,0.891630461095201,0.470034499211284));
#18075=CARTESIAN_POINT('Ctrl Pts',(27.2193698487091,0.918935033135005,0.41356732956778));
#18076=CARTESIAN_POINT('Ctrl Pts',(27.2055606395873,0.987004581363573,0.231746318671411));
#18077=CARTESIAN_POINT('Ctrl Pts',(27.1962633766506,1.00922718171059,0.0992152525598969));
#18078=CARTESIAN_POINT('Ctrl Pts',(27.1822401043235,1.00340136620523,-0.0972176553217059));
#18079=CARTESIAN_POINT('Ctrl Pts',(27.1776216056682,0.9951638680146,-0.161078166755552));
#18080=CARTESIAN_POINT('Ctrl Pts',(27.1637406949851,0.951401802556867,-0.350214922113325));
#18081=CARTESIAN_POINT('Ctrl Pts',(27.1546119632471,0.897664854294904,-0.470552356748959));
#18082=CARTESIAN_POINT('Ctrl Pts',(27.1359749150596,0.747685981774503,-0.68597793018104));
#18083=CARTESIAN_POINT('Ctrl Pts',(27.1265959280299,0.652004951410655,-0.777543331604733));
#18084=CARTESIAN_POINT('Ctrl Pts',(27.1077449073936,0.427849061677098,-0.919147495175399));
#18085=CARTESIAN_POINT('Ctrl Pts',(27.0984509493297,0.302542158836555,-0.967956149819254));
#18086=CARTESIAN_POINT('Ctrl Pts',(27.0844210573905,0.1090489926338,-1.00219031322694));
#18087=CARTESIAN_POINT('Ctrl Pts',(27.0798076083915,0.0450129822140624,
-1.00708214754234));
#18088=CARTESIAN_POINT('Ctrl Pts',(27.0659280179578,-0.149048344906606,
-1.00279330227197));
#18089=CARTESIAN_POINT('Ctrl Pts',(27.0567949468168,-0.278033405463916,
-0.974675255245754));
#18090=CARTESIAN_POINT('Ctrl Pts',(27.0381489605883,-0.519590955197979,
-0.871589515518927));
#18091=CARTESIAN_POINT('Ctrl Pts',(27.028767681825,-0.628508797564383,-0.796566723643565));
#18092=CARTESIAN_POINT('Ctrl Pts',(27.00994229388,-0.812678040764659,-0.606170204142176));
#18093=CARTESIAN_POINT('Ctrl Pts',(27.0006529512941,-0.886066522647178,
-0.493396421490482));
#18094=CARTESIAN_POINT('Ctrl Pts',(26.9866194370948,-0.958938614597588,
-0.310992833312596));
#18095=CARTESIAN_POINT('Ctrl Pts',(26.9820091985959,-0.97671250646186,-0.249421384271684));
#18096=CARTESIAN_POINT('Ctrl Pts',(26.9681351506143,-1.0121086090019,-0.0586423619505615));
#18097=CARTESIAN_POINT('Ctrl Pts',(26.9589993728496,-1.01091662374079,0.0735675041066844));
#18098=CARTESIAN_POINT('Ctrl Pts',(26.9403491684073,-0.959179498422769,
0.331121220497063));
#18099=CARTESIAN_POINT('Ctrl Pts',(26.9309611376611,-0.907891952129337,
0.452903835131262));
#18100=CARTESIAN_POINT('Ctrl Pts',(26.9121666250875,-0.759302137912035,
0.671823573379696));
#18101=CARTESIAN_POINT('Ctrl Pts',(26.9028834236569,-0.663875135361441,
0.766745789531095));
#18102=CARTESIAN_POINT('Ctrl Pts',(26.8888483303339,-0.500262661165281,
0.875221855367422));
#18103=CARTESIAN_POINT('Ctrl Pts',(26.8842421532104,-0.443733473377021,
0.905105546364918));
#18104=CARTESIAN_POINT('Ctrl Pts',(26.8703760201451,-0.264322102188032,
0.978738236522294));
#18105=CARTESIAN_POINT('Ctrl Pts',(26.8612394304227,-0.134496425536785,
1.00465935483348));
#18106=CARTESIAN_POINT('Ctrl Pts',(26.8425874128787,0.12821796553708,1.00659844603438));
#18107=CARTESIAN_POINT('Ctrl Pts',(26.8331935286416,0.257776737069651,0.98122067919966));
#18108=CARTESIAN_POINT('Ctrl Pts',(26.8144314676225,0.502179497876163,0.880737299645244));
#18109=CARTESIAN_POINT('Ctrl Pts',(26.8051560975335,0.614658956622138,0.806776652592242));
#18110=CARTESIAN_POINT('Ctrl Pts',(26.7911216829485,0.754198706932562,0.668917525005024));
#18111=CARTESIAN_POINT('Ctrl Pts',(26.7865203133558,0.794916339912257,0.619808451467912));
#18112=CARTESIAN_POINT('Ctrl Pts',(26.7726637815399,0.903723053949885,0.459423824527641));
#18113=CARTESIAN_POINT('Ctrl Pts',(26.7635284434174,0.955795481190457,0.337553314734785));
#18114=CARTESIAN_POINT('Ctrl Pts',(26.7430671285445,1.01691671680807,0.0559092551204978));
#18115=CARTESIAN_POINT('Ctrl Pts',(26.7335726504057,1.00827361012557,-0.0774627611606082));
#18116=CARTESIAN_POINT('Ctrl Pts',(26.7167489140092,0.96510418020808,-0.310561847663239));
#18117=CARTESIAN_POINT('Ctrl Pts',(26.7074831618654,0.915855808452785,-0.43583755702115));
#18118=CARTESIAN_POINT('Ctrl Pts',(26.6934517331005,0.809682273584885,-0.600555290111322));
#18119=CARTESIAN_POINT('Ctrl Pts',(26.6888556296663,0.770074228022994,-0.650371937404803));
#18120=CARTESIAN_POINT('Ctrl Pts',(26.675009634705,0.63563363352959,-0.789775672636881));
#18121=CARTESIAN_POINT('Ctrl Pts',(26.6658776811606,0.527018763233726,-0.865902447959457));
#18122=CARTESIAN_POINT('Ctrl Pts',(26.6451332237827,0.260335337877291,-0.985279478959959));
#18123=CARTESIAN_POINT('Ctrl Pts',(26.6356306855464,0.12774312417312,-1.00266395438481));
#18124=CARTESIAN_POINT('Ctrl Pts',(26.6191285504318,-0.10481767593479,-1.00840079955666));
#18125=CARTESIAN_POINT('Ctrl Pts',(26.6098742312728,-0.237527656582644,
-0.986082378766112));
#18126=CARTESIAN_POINT('Ctrl Pts',(26.5958478040773,-0.420419005484187,
-0.916233293702868));
#18127=CARTESIAN_POINT('Ctrl Pts',(26.5912565838117,-0.477212390052805,
-0.887817863142468));
#18128=CARTESIAN_POINT('Ctrl Pts',(26.5774207798424,-0.64129015998728,-0.785193009416701));
#18129=CARTESIAN_POINT('Ctrl Pts',(26.5682937239647,-0.738299711072096,
-0.694631109053306));
#18130=CARTESIAN_POINT('Ctrl Pts',(26.5474252312128,-0.911213333992815,
-0.456976015197982));
#18131=CARTESIAN_POINT('Ctrl Pts',(26.5378160228461,-0.955228839604515,
-0.329238910539293));
#18132=CARTESIAN_POINT('Ctrl Pts',(26.5225016105883,-1.0051919273077,-0.119087333308766));
#18133=CARTESIAN_POINT('Ctrl Pts',(26.5141604723334,-1.01252416824994,0.00158815197311223));
#18134=CARTESIAN_POINT('Ctrl Pts',(26.5013873245562,-0.991708199632223,
0.179309126855524));
#18135=CARTESIAN_POINT('Ctrl Pts',(26.4970734565504,-0.979393895210917,
0.237713999577028));
#18136=CARTESIAN_POINT('Ctrl Pts',(26.4884634191094,-0.944019929726152,
0.352096395825399));
#18137=CARTESIAN_POINT('Ctrl Pts',(26.4842212099352,-0.921272789443298,
0.407435861295654));
#18138=CARTESIAN_POINT('Ctrl Pts',(26.48,-0.8939005627167,0.460377710173328));
#18139=CARTESIAN_POINT('',(26.4800266000133,-0.875887823837977,0.505699775546759));
#18140=CARTESIAN_POINT('Ctrl Pts',(26.48,-0.893613512752342,0.4611507504989));
#18141=CARTESIAN_POINT('Ctrl Pts',(26.48,-0.89081917574886,0.468666621828444));
#18142=CARTESIAN_POINT('Ctrl Pts',(26.48,-0.887935158142909,0.476149169831144));
#18143=CARTESIAN_POINT('Ctrl Pts',(26.48,-0.882010577760306,0.490993452370655));
#18144=CARTESIAN_POINT('Ctrl Pts',(26.48,-0.878971184435156,0.498355708662359));
#18145=CARTESIAN_POINT('Ctrl Pts',(26.48,-0.875845991678543,0.505681328412502));
#18146=CARTESIAN_POINT('',(26.6175803212394,-1.08239526302019,0.624914431681246));
#18147=CARTESIAN_POINT('Ctrl Pts',(26.6177473887885,-1.08236453146925,0.624903453604815));
#18148=CARTESIAN_POINT('Ctrl Pts',(26.5948291214948,-1.04800484136653,0.605065877274762));
#18149=CARTESIAN_POINT('Ctrl Pts',(26.5719108542008,-1.01364515126075,0.58522830095031));
#18150=CARTESIAN_POINT('Ctrl Pts',(26.5260127912802,-0.944833526103479,
0.545499890642383));
#18151=CARTESIAN_POINT('Ctrl Pts',(26.5030329956536,-0.910381591051974,
0.525609056658872));
#18152=CARTESIAN_POINT('Ctrl Pts',(26.4800532000267,-0.87592965599741,0.505718222681016));
#18153=CARTESIAN_POINT('Ctrl Pts',(26.6176729436514,-1.08225296268473,0.62483892430428));
#18154=CARTESIAN_POINT('Ctrl Pts',(26.6233229277769,-1.13222243988375,0.538356821464131));
#18155=CARTESIAN_POINT('Ctrl Pts',(26.628840140606,-1.17178227932954,0.445892888274432));
#18156=CARTESIAN_POINT('Ctrl Pts',(26.6398126160615,-1.22565723371071,0.261226310700327));
#18157=CARTESIAN_POINT('Ctrl Pts',(26.6452637354378,-1.24149712443581,0.169751315722489));
#18158=CARTESIAN_POINT('Ctrl Pts',(26.6602924600519,-1.25737930305406,-0.0862086344073024));
#18159=CARTESIAN_POINT('Ctrl Pts',(26.6685515184089,-1.23440178668179,-0.235205427087828));
#18160=CARTESIAN_POINT('Ctrl Pts',(26.6850772214207,-1.14935312334068,-0.516442894477973));
#18161=CARTESIAN_POINT('Ctrl Pts',(26.693633133589,-1.07866597598953,-0.644497028069737));
#18162=CARTESIAN_POINT('Ctrl Pts',(26.705952000928,-0.951273837925217,-0.814528408486582));
#18163=CARTESIAN_POINT('Ctrl Pts',(26.7106361966476,-0.895018277429958,
-0.87577575106266));
#18164=CARTESIAN_POINT('Ctrl Pts',(26.7206751402919,-0.762322350473856,
-0.994581826367339));
#18165=CARTESIAN_POINT('Ctrl Pts',(26.7260298582995,-0.684068404833238,
-1.05018828899575));
#18166=CARTESIAN_POINT('Ctrl Pts',(26.7355561252237,-0.53891920407384,-1.12995717925848));
#18167=CARTESIAN_POINT('Ctrl Pts',(26.7396608009472,-0.474911111502257,
-1.15829422468238));
#18168=CARTESIAN_POINT('Ctrl Pts',(26.7530210523164,-0.25800087723676,-1.23305883785933));
#18169=CARTESIAN_POINT('Ctrl Pts',(26.7619861989868,-0.0972512468538276,
-1.25562451060708));
#18170=CARTESIAN_POINT('Ctrl Pts',(26.7803410435921,0.225443202719235,-1.24029034488642));
#18171=CARTESIAN_POINT('Ctrl Pts',(26.7896883750463,0.383702507178638,-1.2007301368539));
#18172=CARTESIAN_POINT('Ctrl Pts',(26.80382706628,0.606433346984284,-1.0954489537623));
#18173=CARTESIAN_POINT('Ctrl Pts',(26.8085441969838,0.677671505270773,-1.05281147333592));
#18174=CARTESIAN_POINT('Ctrl Pts',(26.8199336274881,0.838263677832852,-0.934102162227965));
#18175=CARTESIAN_POINT('Ctrl Pts',(26.829328142703,0.964516250915906,-0.821620611431171));
#18176=CARTESIAN_POINT('Ctrl Pts',(26.8504869605049,1.15343023316433,-0.506482220582575));
#18177=CARTESIAN_POINT('Ctrl Pts',(26.8598366313787,1.20978204209892,-0.351570030074152));
#18178=CARTESIAN_POINT('Ctrl Pts',(26.8737389494541,1.2478031354602,-0.110426880252088));
#18179=CARTESIAN_POINT('Ctrl Pts',(26.8783363175325,1.2524274771249,-0.0283093125836477));
#18180=CARTESIAN_POINT('Ctrl Pts',(26.8918898714561,1.24172752266081,0.208333288214192));
#18181=CARTESIAN_POINT('Ctrl Pts',(26.9009488769085,1.2058442502652,0.361223885151522));
#18182=CARTESIAN_POINT('Ctrl Pts',(26.9190682007871,1.07937320915612,0.650515496858714));
#18183=CARTESIAN_POINT('Ctrl Pts',(26.9277929791483,0.987506469895415,0.783029094899924));
#18184=CARTESIAN_POINT('Ctrl Pts',(26.9454649798215,0.768868859633136,0.995161173191032));
#18185=CARTESIAN_POINT('Ctrl Pts',(26.9547722464512,0.638107577335029,1.08803878674962));
#18186=CARTESIAN_POINT('Ctrl Pts',(26.9684941446703,0.412490985363296,1.18199876591539));
#18187=CARTESIAN_POINT('Ctrl Pts',(26.9725362315898,0.342875121890448,1.20407214480854));
#18188=CARTESIAN_POINT('Ctrl Pts',(26.9813229028305,0.192126306293707,1.23759666842505));
#18189=CARTESIAN_POINT('Ctrl Pts',(26.9861010085444,0.110744116420164,1.24736969716722));
#18190=CARTESIAN_POINT('Ctrl Pts',(26.9957932142666,-0.0546765437387625,
1.2511707678145));
#18191=CARTESIAN_POINT('Ctrl Pts',(27.0007125467791,-0.138968930008962,
1.24471180503867));
#18192=CARTESIAN_POINT('Ctrl Pts',(27.0138122303823,-0.366001853172527,
1.20378429434567));
#18193=CARTESIAN_POINT('Ctrl Pts',(27.0227913010392,-0.523855189025296,
1.14928485542831));
#18194=CARTESIAN_POINT('Ctrl Pts',(27.0378215228918,-0.739530067688057,
1.01012100713631));
#18195=CARTESIAN_POINT('Ctrl Pts',(27.0422130830678,-0.798426271672689,
0.964216832556656));
#18196=CARTESIAN_POINT('Ctrl Pts',(27.0512360042357,-0.912670203933948,
0.857452222520315));
#18197=CARTESIAN_POINT('Ctrl Pts',(27.05584015108,-0.967015893635766,0.795547574443293));
#18198=CARTESIAN_POINT('Ctrl Pts',(27.0659525686896,-1.07220736914641,0.649253735520837));
#18199=CARTESIAN_POINT('Ctrl Pts',(27.0714835605872,-1.12033323576103,0.562678461508257));
#18200=CARTESIAN_POINT('Ctrl Pts',(27.0819455506405,-1.18817465505177,0.396139701307846));
#18201=CARTESIAN_POINT('Ctrl Pts',(27.0867385530711,-1.21134478405695,0.318194492985015));
#18202=CARTESIAN_POINT('Ctrl Pts',(27.0962163230492,-1.2424108923148,0.15708382713042));
#18203=CARTESIAN_POINT('Ctrl Pts',(27.1008945859079,-1.24996681522301,0.0743209691452767));
#18204=CARTESIAN_POINT('Ctrl Pts',(27.111106975172,-1.24880222921897,-0.106693673917988));
#18205=CARTESIAN_POINT('Ctrl Pts',(27.1166420030754,-1.23673577746144,-0.204964063443941));
#18206=CARTESIAN_POINT('Ctrl Pts',(27.1266813126859,-1.1951055545968,-0.373989150302864));
#18207=CARTESIAN_POINT('Ctrl Pts',(27.1311183617704,-1.17029860772482,-0.445467179592022));
#18208=CARTESIAN_POINT('Ctrl Pts',(27.1447673082394,-1.07278792151908,-0.660273870989051));
#18209=CARTESIAN_POINT('Ctrl Pts',(27.1537912956173,-0.97829819161165,-0.793339356174457));
#18210=CARTESIAN_POINT('Ctrl Pts',(27.1673751717089,-0.806192065988158,
-0.958291527069703));
#18211=CARTESIAN_POINT('Ctrl Pts',(27.1718772242941,-0.744634653422319,
-1.00713043498214));
#18212=CARTESIAN_POINT('Ctrl Pts',(27.185600276084,-0.545160500110301,-1.13577857803707));
#18213=CARTESIAN_POINT('Ctrl Pts',(27.194708148134,-0.394986518730001,-1.19570312093531));
#18214=CARTESIAN_POINT('Ctrl Pts',(27.210896999223,-0.116849507298023,-1.25044185698086));
#18215=CARTESIAN_POINT('Ctrl Pts',(27.2202104785418,0.0506293948963337,
-1.26554583438168));
#18216=CARTESIAN_POINT('Ctrl Pts',(27.2412324844468,0.407852860075084,-1.19180544801608));
#18217=CARTESIAN_POINT('Ctrl Pts',(27.2505976074347,0.559836704426273,-1.12866736293217));
#18218=CARTESIAN_POINT('Ctrl Pts',(27.26421794799,0.759501734458928,-0.995862606038345));
#18219=CARTESIAN_POINT('Ctrl Pts',(27.2685769038316,0.820173225627903,-0.946539669293757));
#18220=CARTESIAN_POINT('Ctrl Pts',(27.2800270563151,0.962634433699707,-0.806046356647483));
#18221=CARTESIAN_POINT('Ctrl Pts',(27.287149432565,1.03664674878547,-0.707833652042005));
#18222=CARTESIAN_POINT('Ctrl Pts',(27.3037659770571,1.17511828860313,-0.456149209535922));
#18223=CARTESIAN_POINT('Ctrl Pts',(27.3127655717947,1.22549966150738,-0.297199147241388));
#18224=CARTESIAN_POINT('Ctrl Pts',(27.3278203043008,1.25270772564518,-0.0368720188271256));
#18225=CARTESIAN_POINT('Ctrl Pts',(27.3334311918074,1.25171066149632,0.0591489682065003));
#18226=CARTESIAN_POINT('Ctrl Pts',(27.3493594591518,1.21813364413176,0.330701470812096));
#18227=CARTESIAN_POINT('Ctrl Pts',(27.3583824392094,1.16064739395832,0.488307261101328));
#18228=CARTESIAN_POINT('Ctrl Pts',(27.3710195528419,1.05054076564694,0.680361565920234));
#18229=CARTESIAN_POINT('Ctrl Pts',(27.3750061791313,1.01172907400335,0.736682885072757));
#18230=CARTESIAN_POINT('Ctrl Pts',(27.3837173999563,0.917762226612901,0.851842029224438));
#18231=CARTESIAN_POINT('Ctrl Pts',(27.3884507068375,0.860813114976424,0.909412367610113));
#18232=CARTESIAN_POINT('Ctrl Pts',(27.3973428772326,0.741055000375852,1.00895802344042));
#18233=CARTESIAN_POINT('Ctrl Pts',(27.4015275583348,0.679029369463859,1.05170053647916));
#18234=CARTESIAN_POINT('Ctrl Pts',(27.4156137715033,0.46012589084204,1.17528367642436));
#18235=CARTESIAN_POINT('Ctrl Pts',(27.4251567813477,0.302460240456135,1.22161543060849));
#18236=CARTESIAN_POINT('Ctrl Pts',(27.4392158463335,0.0621563960705467,
1.25159362700516));
#18237=CARTESIAN_POINT('Ctrl Pts',(27.444496878216,-0.0322708771125176,
1.2525822727184));
#18238=CARTESIAN_POINT('Ctrl Pts',(27.4543480803958,-0.206727963977358,
1.23505225854882));
#18239=CARTESIAN_POINT('Ctrl Pts',(27.4589334593879,-0.287152557177882,
1.21902395681331));
#18240=CARTESIAN_POINT('Ctrl Pts',(27.4682321073975,-0.4416970928263,1.1719697789001));
#18241=CARTESIAN_POINT('Ctrl Pts',(27.4729516116456,-0.515727287380908,
1.14127995022307));
#18242=CARTESIAN_POINT('Ctrl Pts',(27.4843874363185,-0.689129958916375,
1.04895667382227));
#18243=CARTESIAN_POINT('Ctrl Pts',(27.4909756978049,-0.784294679972773,
0.979488370451264));
#18244=CARTESIAN_POINT('Ctrl Pts',(27.5022112586547,-0.927437896374184,
0.841419073632032));
#18245=CARTESIAN_POINT('Ctrl Pts',(27.5068694100356,-0.981136459626848,
0.778485227271648));
#18246=CARTESIAN_POINT('Ctrl Pts',(27.5163578130054,-1.07504666274919,0.643084026884325));
#18247=CARTESIAN_POINT('Ctrl Pts',(27.5211626001225,-1.1148376357819,0.571161446600757));
#18248=CARTESIAN_POINT('Ctrl Pts',(27.5352457956388,-1.21111916930948,0.346914450665397));
#18249=CARTESIAN_POINT('Ctrl Pts',(27.5443859627255,-1.24599797633614,0.185793411298435));
#18250=CARTESIAN_POINT('Ctrl Pts',(27.5653868720338,-1.25396608250648,-0.182192741678661));
#18251=CARTESIAN_POINT('Ctrl Pts',(27.5749869004016,-1.206632677805,-0.344777573954174));
#18252=CARTESIAN_POINT('Ctrl Pts',(27.5863792440645,-1.13455557543746,-0.529557994741678));
#18253=CARTESIAN_POINT('Ctrl Pts',(27.5911157086978,-1.09700019906553,-0.603652685816796));
#18254=CARTESIAN_POINT('Ctrl Pts',(27.6052193646264,-0.96440654221833,-0.81188213774616));
#18255=CARTESIAN_POINT('Ctrl Pts',(27.614292162518,-0.851307653605388,-0.929748658073967));
#18256=CARTESIAN_POINT('Ctrl Pts',(27.6310557749972,-0.613091677158633,
-1.09581581684141));
#18257=CARTESIAN_POINT('Ctrl Pts',(27.638388107942,-0.498563383005862,-1.15256212981081));
#18258=CARTESIAN_POINT('Ctrl Pts',(27.6529532597672,-0.255556338240585,
-1.23032546824917));
#18259=CARTESIAN_POINT('Ctrl Pts',(27.6600166118184,-0.128743288277099,
-1.24994404136352));
#18260=CARTESIAN_POINT('Ctrl Pts',(27.6674547598791,1.13833429835281E-5,
-1.24969819048317));
#18261=CARTESIAN_POINT('Ctrl Pts',(27.85693036647,0.3508711481781,-0.9020783645694));
#18262=CARTESIAN_POINT('Ctrl Pts',(27.84253965393,0.1696145104598,-0.9725796947077));
#18263=CARTESIAN_POINT('Ctrl Pts',(27.81375822884,-0.2362176485044,-1.000787437649));
#18264=CARTESIAN_POINT('Ctrl Pts',(27.7705860912,-0.7620645579118,-0.6904694580177));
#18265=CARTESIAN_POINT('Ctrl Pts',(27.72741395357,-1.019191121247,-0.136727519574));
#18266=CARTESIAN_POINT('Ctrl Pts',(27.68424181593,-0.9170855048544,0.4651998272662));
#18267=CARTESIAN_POINT('Ctrl Pts',(27.6410696783,-0.491706155922,0.9031499546372));
#18268=CARTESIAN_POINT('Ctrl Pts',(27.59789754066,0.1069945696502,1.022744811683));
#18269=CARTESIAN_POINT('Ctrl Pts',(27.55472540303,0.6679809012817,0.7818289067868));
#18270=CARTESIAN_POINT('Ctrl Pts',(27.51155326539,0.9935081337884,0.2653232965403));
#18271=CARTESIAN_POINT('Ctrl Pts',(27.46838112776,0.9688301855632,-0.3447070524446));
#18272=CARTESIAN_POINT('Ctrl Pts',(27.42520899013,0.6026458286235,-0.8332303898637));
#18273=CARTESIAN_POINT('Ctrl Pts',(27.38203685249,0.0240327020293,-1.028045381657));
#18274=CARTESIAN_POINT('Ctrl Pts',(27.33886471486,-0.5630517979017,-0.8604809995253));
#18275=CARTESIAN_POINT('Ctrl Pts',(27.29569257722,-0.9516641661597,-0.3896026083503));
#18276=CARTESIAN_POINT('Ctrl Pts',(27.25252043959,-1.004821046675,0.2186081923639));
#18277=CARTESIAN_POINT('Ctrl Pts',(27.20934830195,-0.7037849814483,0.7497610135854));
#18278=CARTESIAN_POINT('Ctrl Pts',(27.16617616432,-0.1546692441643,1.016627907602));
#18279=CARTESIAN_POINT('Ctrl Pts',(27.12300402668,0.4489664052826,0.9251400134749));
#18280=CARTESIAN_POINT('Ctrl Pts',(27.07983188905,0.8943442891871,0.5075462245036));
#18281=CARTESIAN_POINT('Ctrl Pts',(27.03665975141,1.024471572654,-0.08895433890703));
#18282=CARTESIAN_POINT('Ctrl Pts',(26.99348761378,0.7934792266292,-0.6540990709153));
#18283=CARTESIAN_POINT('Ctrl Pts',(26.95031547614,0.282790564744,-0.9886780942271));
#18284=CARTESIAN_POINT('Ctrl Pts',(26.90714333851,-0.3275799486865,-0.9747544586039));
#18285=CARTESIAN_POINT('Ctrl Pts',(26.86397120087,-0.8224806433027,-0.6172361556615));
#18286=CARTESIAN_POINT('Ctrl Pts',(26.82079906324,-1.027462199362,-0.04214608490148));
#18287=CARTESIAN_POINT('Ctrl Pts',(26.7776269256,-0.8702699878541,0.5478002119432));
#18288=CARTESIAN_POINT('Ctrl Pts',(26.73445478797,-0.4063130678999,0.9446504531373));
#18289=CARTESIAN_POINT('Ctrl Pts',(26.69128265034,0.200866052972,1.008517532369));
#18290=CARTESIAN_POINT('Ctrl Pts',(26.6481105127,0.7372431919551,0.7168885397455));
#18291=CARTESIAN_POINT('Ctrl Pts',(26.60493837507,1.013739362113,0.172561472936));
#18292=CARTESIAN_POINT('Ctrl Pts',(26.56176623743,0.9329269024502,-0.4325943337183));
#18293=CARTESIAN_POINT('Ctrl Pts',(26.5185940998,0.5231593542597,-0.8852562131224));
#18294=CARTESIAN_POINT('Ctrl Pts',(26.48981267471,0.1273004522624,-0.9790173336412));
#18295=CARTESIAN_POINT('Ctrl Pts',(26.47542196216,-0.06672189150808,-0.9656107536899));
#18296=CARTESIAN_POINT('Ctrl Pts',(27.79531292359,0.3895590831803,-1.001543793165));
#18297=CARTESIAN_POINT('Ctrl Pts',(27.78092221105,0.1883166328491,-1.079818777228));
#18298=CARTESIAN_POINT('Ctrl Pts',(27.75214078596,-0.2622636003565,-1.111136776829));
#18299=CARTESIAN_POINT('Ctrl Pts',(27.70896864832,-0.8460917121451,-0.7666023565235));
#18300=CARTESIAN_POINT('Ctrl Pts',(27.66579651069,-1.131569696854,-0.1518034396597));
#18301=CARTESIAN_POINT('Ctrl Pts',(27.62262437306,-1.018205658471,0.5164939298841));
#18302=CARTESIAN_POINT('Ctrl Pts',(27.57945223542,-0.545922912983,1.002733539448));
#18303=CARTESIAN_POINT('Ctrl Pts',(27.53628009779,0.1187920599189,1.135515226132));
#18304=CARTESIAN_POINT('Ctrl Pts',(27.49310796015,0.7416341549781,0.8680353278211));
#18305=CARTESIAN_POINT('Ctrl Pts',(27.44993582252,1.103054838622,0.2945785103259));
#18306=CARTESIAN_POINT('Ctrl Pts',(27.40676368488,1.075655837777,-0.3827153187527));
#18307=CARTESIAN_POINT('Ctrl Pts',(27.36359154725,0.669095072935,-0.9251044676621));
#18308=CARTESIAN_POINT('Ctrl Pts',(27.32041940961,0.02668260818108,-1.141400250279));
#18309=CARTESIAN_POINT('Ctrl Pts',(27.27724727198,-0.6251353048336,-0.9553597980619));
#18310=CARTESIAN_POINT('Ctrl Pts',(27.23407513434,-1.056597049914,-0.4325611715347));
#18311=CARTESIAN_POINT('Ctrl Pts',(27.19090299671,-1.115615141728,0.242712481306));
#18312=CARTESIAN_POINT('Ctrl Pts',(27.14773085907,-0.781386083047,0.8324315480863));
#18313=CARTESIAN_POINT('Ctrl Pts',(27.10455872144,-0.1717234639146,1.128723856827));
#18314=CARTESIAN_POINT('Ctrl Pts',(27.0613865838,0.4984705699766,1.027148277463));
#18315=CARTESIAN_POINT('Ctrl Pts',(27.01821444617,0.9929569391852,0.5635095473536));
#18316=CARTESIAN_POINT('Ctrl Pts',(26.97504230853,1.137432384109,-0.09876266797504));
#18317=CARTESIAN_POINT('Ctrl Pts',(26.9318701709,0.8809702412221,-0.7262216790921));
#18318=CARTESIAN_POINT('Ctrl Pts',(26.88869803327,0.3139717634401,-1.097692226755));
#18319=CARTESIAN_POINT('Ctrl Pts',(26.84552589563,-0.3636997374712,-1.082233336059));
#18320=CARTESIAN_POINT('Ctrl Pts',(26.802353758,-0.913169427017,-0.6852941661171));
#18321=CARTESIAN_POINT('Ctrl Pts',(26.75918162036,-1.140752764838,-0.04679321819168));
#18322=CARTESIAN_POINT('Ctrl Pts',(26.71600948273,-0.9662281448565,0.6082020406598));
#18323=CARTESIAN_POINT('Ctrl Pts',(26.67283734509,-0.4511141683696,1.048809987259));
#18324=CARTESIAN_POINT('Ctrl Pts',(26.62966520746,0.2230140490152,1.119719211229));
#18325=CARTESIAN_POINT('Ctrl Pts',(26.58649306982,0.8185334799691,0.7959344726286));
#18326=CARTESIAN_POINT('Ctrl Pts',(26.54332093219,1.125516813049,0.1915885348176));
#18327=CARTESIAN_POINT('Ctrl Pts',(26.50014879455,1.035793768396,-0.4802932726369));
#18328=CARTESIAN_POINT('Ctrl Pts',(26.45697665692,0.580844220053,-0.9828667890031));
#18329=CARTESIAN_POINT('Ctrl Pts',(26.42819523183,0.1413369202036,-1.086966246416));
#18330=CARTESIAN_POINT('Ctrl Pts',(26.41380451928,-0.07407881502629,-1.072081423251));
#18331=CARTESIAN_POINT('Ctrl Pts',(27.73369548072,0.4282470181825,-1.101009221761));
#18332=CARTESIAN_POINT('Ctrl Pts',(27.71930476817,0.2070187552385,-1.187057859748));
#18333=CARTESIAN_POINT('Ctrl Pts',(27.69052334308,-0.2883095522085,-1.221486116009));
#18334=CARTESIAN_POINT('Ctrl Pts',(27.64735120545,-0.9301188663785,-0.8427352550292));
#18335=CARTESIAN_POINT('Ctrl Pts',(27.60417906781,-1.24394827246,-0.1668793597454));
#18336=CARTESIAN_POINT('Ctrl Pts',(27.56100693018,-1.119325812087,0.5677880325021));
#18337=CARTESIAN_POINT('Ctrl Pts',(27.51783479254,-0.6001396700441,1.102317124259));
#18338=CARTESIAN_POINT('Ctrl Pts',(27.47466265491,0.1305895501877,1.248285640581));
#18339=CARTESIAN_POINT('Ctrl Pts',(27.43149051727,0.8152874086746,0.9542417488555));
#18340=CARTESIAN_POINT('Ctrl Pts',(27.38831837964,1.212601543456,0.3238337241115));
#18341=CARTESIAN_POINT('Ctrl Pts',(27.345146242,1.182481489992,-0.4207235850609));
#18342=CARTESIAN_POINT('Ctrl Pts',(27.30197410437,0.7355443172465,-1.016978545461));
#18343=CARTESIAN_POINT('Ctrl Pts',(27.25880196673,0.02933251433285,-1.2547551189));
#18344=CARTESIAN_POINT('Ctrl Pts',(27.2156298291,-0.6872188117655,-1.050238596599));
#18345=CARTESIAN_POINT('Ctrl Pts',(27.17245769147,-1.161529933667,-0.475519734719));
#18346=CARTESIAN_POINT('Ctrl Pts',(27.12928555383,-1.226409236781,0.2668167702481));
#18347=CARTESIAN_POINT('Ctrl Pts',(27.0861134162,-0.8589871846457,0.9151020825871));
#18348=CARTESIAN_POINT('Ctrl Pts',(27.04294127856,-0.1887776836649,1.240819806052));
#18349=CARTESIAN_POINT('Ctrl Pts',(26.99976914093,0.5479747346705,1.129156541452));
#18350=CARTESIAN_POINT('Ctrl Pts',(26.95659700329,1.091569589183,0.6194728702036));
#18351=CARTESIAN_POINT('Ctrl Pts',(26.91342486566,1.250393195564,-0.1085709970431));
#18352=CARTESIAN_POINT('Ctrl Pts',(26.87025272802,0.968461255815,-0.7983442872689));
#18353=CARTESIAN_POINT('Ctrl Pts',(26.82708059039,0.3451529621362,-1.206706359282));
#18354=CARTESIAN_POINT('Ctrl Pts',(26.78390845275,-0.3998195262558,-1.189712213514));
#18355=CARTESIAN_POINT('Ctrl Pts',(26.74073631512,-1.003858210731,-0.7533521765727));
#18356=CARTESIAN_POINT('Ctrl Pts',(26.69756417748,-1.254043330314,-0.05144035148188));
#18357=CARTESIAN_POINT('Ctrl Pts',(26.65439203985,-1.062186301859,0.6686038693765));
#18358=CARTESIAN_POINT('Ctrl Pts',(26.61121990221,-0.4959152688394,1.15296952138));
#18359=CARTESIAN_POINT('Ctrl Pts',(26.56804776458,0.2451620450585,1.230920890089));
#18360=CARTESIAN_POINT('Ctrl Pts',(26.52487562694,0.8998237679831,0.8749804055118));
#18361=CARTESIAN_POINT('Ctrl Pts',(26.48170348931,1.237294263986,0.2106155966992));
#18362=CARTESIAN_POINT('Ctrl Pts',(26.43853135168,1.138660634342,-0.5279922115554));
#18363=CARTESIAN_POINT('Ctrl Pts',(26.39535921404,0.6385290858464,-1.080477364884));
#18364=CARTESIAN_POINT('Ctrl Pts',(26.36657778895,0.1553733881448,-1.194915159191));
#18365=CARTESIAN_POINT('Ctrl Pts',(26.35218707641,-0.08143573854449,-1.178552092812));
#18366=CARTESIAN_POINT('Ctrl Pts',(27.67207803784,0.4669349531848,-1.200474650356));
#18367=CARTESIAN_POINT('Ctrl Pts',(27.65768732529,0.2257208776278,-1.294296942268));
#18368=CARTESIAN_POINT('Ctrl Pts',(27.6289059002,-0.3143555040606,-1.33183545519));
#18369=CARTESIAN_POINT('Ctrl Pts',(27.58573376257,-1.014146020612,-0.9188681535349));
#18370=CARTESIAN_POINT('Ctrl Pts',(27.54256162493,-1.356326848067,-0.181955279831));
#18371=CARTESIAN_POINT('Ctrl Pts',(27.4993894873,-1.220445965703,0.6190821351201));
#18372=CARTESIAN_POINT('Ctrl Pts',(27.45621734966,-0.6543564271052,1.20190070907));
#18373=CARTESIAN_POINT('Ctrl Pts',(27.41304521203,0.1423870404564,1.36105605503));
#18374=CARTESIAN_POINT('Ctrl Pts',(27.3698730744,0.888940662371,1.04044816989));
#18375=CARTESIAN_POINT('Ctrl Pts',(27.32670093676,1.32214824829,0.353088937897));
#18376=CARTESIAN_POINT('Ctrl Pts',(27.28352879913,1.289307142206,-0.458731851369));
#18377=CARTESIAN_POINT('Ctrl Pts',(27.24035666149,0.8019935615581,-1.108852623259));
#18378=CARTESIAN_POINT('Ctrl Pts',(27.19718452386,0.03198242048463,-1.368109987522));
#18379=CARTESIAN_POINT('Ctrl Pts',(27.15401238622,-0.7493023186974,-1.145117395135));
#18380=CARTESIAN_POINT('Ctrl Pts',(27.11084024859,-1.266462817421,-0.5184782979033));
#18381=CARTESIAN_POINT('Ctrl Pts',(27.06766811095,-1.337203331834,0.2909210591902));
#18382=CARTESIAN_POINT('Ctrl Pts',(27.02449597332,-0.9365882862444,0.997772617088));
#18383=CARTESIAN_POINT('Ctrl Pts',(26.98132383568,-0.2058319034152,1.352915755277));
#18384=CARTESIAN_POINT('Ctrl Pts',(26.93815169805,0.5974788993645,1.23116480544));
#18385=CARTESIAN_POINT('Ctrl Pts',(26.89497956041,1.190182239181,0.6754361930536));
#18386=CARTESIAN_POINT('Ctrl Pts',(26.85180742278,1.36335400702,-0.1183793261111));
#18387=CARTESIAN_POINT('Ctrl Pts',(26.80863528514,1.055952270408,-0.8704668954457));
#18388=CARTESIAN_POINT('Ctrl Pts',(26.76546314751,0.3763341608323,-1.31572049181));
#18389=CARTESIAN_POINT('Ctrl Pts',(26.72229100988,-0.4359393150405,-1.29719109097));
#18390=CARTESIAN_POINT('Ctrl Pts',(26.67911887224,-1.094546994446,-0.8214101870282));
#18391=CARTESIAN_POINT('Ctrl Pts',(26.63594673461,-1.367333895789,-0.05608748477207));
#18392=CARTESIAN_POINT('Ctrl Pts',(26.59277459697,-1.158144458861,0.7290056980931));
#18393=CARTESIAN_POINT('Ctrl Pts',(26.54960245934,-0.5407163693092,1.257129055501));
#18394=CARTESIAN_POINT('Ctrl Pts',(26.5064303217,0.2673100411017,1.342122568949));
#18395=CARTESIAN_POINT('Ctrl Pts',(26.46325818407,0.9811140559971,0.954026338395));
#18396=CARTESIAN_POINT('Ctrl Pts',(26.42008604643,1.349071714923,0.2296426585807));
#18397=CARTESIAN_POINT('Ctrl Pts',(26.3769139088,1.241527500287,-0.575691150474));
#18398=CARTESIAN_POINT('Ctrl Pts',(26.33374177116,0.6962139516397,-1.178087940765));
#18399=CARTESIAN_POINT('Ctrl Pts',(26.30496034607,0.1694098560859,-1.302864071967));
#18400=CARTESIAN_POINT('Ctrl Pts',(26.29056963353,-0.08879266206269,-1.285022762373));
#18401=CARTESIAN_POINT('',(26.4799750801814,0.957494124951751,0.803490379093413));
#18402=CARTESIAN_POINT('',(26.48,0.30130639050121,-0.959765445450973));
#18403=CARTESIAN_POINT('Ctrl Pts',(26.48,0.957461769231118,0.803461599229706));
#18404=CARTESIAN_POINT('Ctrl Pts',(26.48,1.02085303890837,0.710326903088572));
#18405=CARTESIAN_POINT('Ctrl Pts',(26.4800000000004,1.07146792946953,0.608458766671006));
#18406=CARTESIAN_POINT('Ctrl Pts',(26.4800000000004,1.14222700822191,0.398129979097469));
#18407=CARTESIAN_POINT('Ctrl Pts',(26.48,1.16333891588263,0.289629207331002));
#18408=CARTESIAN_POINT('Ctrl Pts',(26.48,1.17576370208854,0.0291771618104245));
#18409=CARTESIAN_POINT('Ctrl Pts',(26.4799999998511,1.15317936540575,-0.122946830566836));
#18410=CARTESIAN_POINT('Ctrl Pts',(26.4799999998511,1.05339965425113,-0.402142814256775));
#18411=CARTESIAN_POINT('Ctrl Pts',(26.48,0.979092823411478,-0.526892044615511));
#18412=CARTESIAN_POINT('Ctrl Pts',(26.48,0.80319537267829,-0.719709080817574));
#18413=CARTESIAN_POINT('Ctrl Pts',(26.48,0.711886836330681,-0.792651002690939));
#18414=CARTESIAN_POINT('Ctrl Pts',(26.48,0.488721612126881,-0.916845005852681));
#18415=CARTESIAN_POINT('Ctrl Pts',(26.48,0.378913387594024,-0.945604681625937));
#18416=CARTESIAN_POINT('Ctrl Pts',(26.48,0.30130639050121,-0.959765445450973));
#18417=CARTESIAN_POINT('Ctrl Pts',(27.8084936838606,-7.83629518364392E-6,
-1.00548644875247));
#18418=CARTESIAN_POINT('Ctrl Pts',(27.8009336227228,-0.105754067060467,
-1.00565130875726));
#18419=CARTESIAN_POINT('Ctrl Pts',(27.7920355843156,-0.229774370990478,
-0.989890792203826));
#18420=CARTESIAN_POINT('Ctrl Pts',(27.773278015885,-0.47684507127086,-0.893688393002027));
#18421=CARTESIAN_POINT('Ctrl Pts',(27.7647110839715,-0.58323674538791,-0.827893655969334));
#18422=CARTESIAN_POINT('Ctrl Pts',(27.7494978495145,-0.741104731770526,
-0.685814064305951));
#18423=CARTESIAN_POINT('Ctrl Pts',(27.7433408520941,-0.794958590434357,
-0.621862691176406));
#18424=CARTESIAN_POINT('Ctrl Pts',(27.7328730435246,-0.875623640068458,
-0.499430636746069));
#18425=CARTESIAN_POINT('Ctrl Pts',(27.7282665986025,-0.906439891086461,
-0.440457560251828));
#18426=CARTESIAN_POINT('Ctrl Pts',(27.7174007537854,-0.964992524600893,
-0.295815934039164));
#18427=CARTESIAN_POINT('Ctrl Pts',(27.7111175803318,-0.987750306056034,
-0.208040340531976));
#18428=CARTESIAN_POINT('Ctrl Pts',(27.6986095379843,-1.00844004152666,-0.0382152991818625));
#18429=CARTESIAN_POINT('Ctrl Pts',(27.6925773617797,-1.00849881112007,0.0433778302428258));
#18430=CARTESIAN_POINT('Ctrl Pts',(27.6808363100849,-0.987396042424842,
0.209104271202132));
#18431=CARTESIAN_POINT('Ctrl Pts',(27.6750717349432,-0.965801035552071,
0.291998972276148));
#18432=CARTESIAN_POINT('Ctrl Pts',(27.6627065622329,-0.900686289080503,
0.455917110370338));
#18433=CARTESIAN_POINT('Ctrl Pts',(27.6558888426671,-0.855591925828399,
0.536406732927371));
#18434=CARTESIAN_POINT('Ctrl Pts',(27.6426720250847,-0.746938893915059,
0.679824479257801));
#18435=CARTESIAN_POINT('Ctrl Pts',(27.6363904762984,-0.682615856064763,
0.745256780425583));
#18436=CARTESIAN_POINT('Ctrl Pts',(27.6261346961145,-0.562949307185261,
0.834625638450677));
#18437=CARTESIAN_POINT('Ctrl Pts',(27.6226177132574,-0.519867531455672,
0.862024926125074));
#18438=CARTESIAN_POINT('Ctrl Pts',(27.6131419042199,-0.403160023299481,
0.924626544942976));
#18439=CARTESIAN_POINT('Ctrl Pts',(27.6070066010663,-0.326679169221438,
0.954639953302017));
#18440=CARTESIAN_POINT('Ctrl Pts',(27.597120056192,-0.19552463113609,0.988296274420178));
#18441=CARTESIAN_POINT('Ctrl Pts',(27.5933330803712,-0.14272693439211,0.99730913976307));
#18442=CARTESIAN_POINT('Ctrl Pts',(27.5829898392745,0.00664271603791499,
1.01023975061682));
#18443=CARTESIAN_POINT('Ctrl Pts',(27.5764661542004,0.103460129787075,1.0045930441376));
#18444=CARTESIAN_POINT('Ctrl Pts',(27.563773697374,0.274950320035545,0.970307099663595));
#18445=CARTESIAN_POINT('Ctrl Pts',(27.5578955858851,0.350585845332744,0.945917150096465));
#18446=CARTESIAN_POINT('Ctrl Pts',(27.5461449513803,0.498391225782096,0.87796896122679));
#18447=CARTESIAN_POINT('Ctrl Pts',(27.540531079811,0.56887184427116,0.833722867995117));
#18448=CARTESIAN_POINT('Ctrl Pts',(27.5262887031483,0.728308631585911,0.703771282776339));
#18449=CARTESIAN_POINT('Ctrl Pts',(27.5172053338825,0.809402654229873,0.608834343437791));
#18450=CARTESIAN_POINT('Ctrl Pts',(27.4964498235742,0.953372208461222,0.361035812979152));
#18451=CARTESIAN_POINT('Ctrl Pts',(27.4875406304835,0.983506134098712,0.229915481838277));
#18452=CARTESIAN_POINT('Ctrl Pts',(27.4718461172469,1.01312158666829,0.0114826670106345));
#18453=CARTESIAN_POINT('Ctrl Pts',(27.4625850017575,1.00681094283761,-0.117481830530138));
#18454=CARTESIAN_POINT('Ctrl Pts',(27.448890878927,0.961220081906566,-0.30412355893231));
#18455=CARTESIAN_POINT('Ctrl Pts',(27.4443571105972,0.939479882086676,-0.365378803348319));
#18456=CARTESIAN_POINT('Ctrl Pts',(27.4305000744923,0.856277477027791,-0.542967381960826));
#18457=CARTESIAN_POINT('Ctrl Pts',(27.4211503950537,0.777214337805915,-0.651022403982935));
#18458=CARTESIAN_POINT('Ctrl Pts',(27.4072442145789,0.634940248517312,-0.782652594761028));
#18459=CARTESIAN_POINT('Ctrl Pts',(27.4027040017641,0.584921314853706,-0.820976495091213));
#18460=CARTESIAN_POINT('Ctrl Pts',(27.3888085142676,0.419653710460084,-0.923480810164823));
#18461=CARTESIAN_POINT('Ctrl Pts',(27.3797021246236,0.29411315679714,-0.970164097544654));
#18462=CARTESIAN_POINT('Ctrl Pts',(27.3636473871652,0.071521787740989,-1.00750002449848));
#18463=CARTESIAN_POINT('Ctrl Pts',(27.3537095866507,-0.0642830173812026,
-1.017760320162));
#18464=CARTESIAN_POINT('Ctrl Pts',(27.3328121873029,-0.354868943366727,
-0.949954651919668));
#18465=CARTESIAN_POINT('Ctrl Pts',(27.3237113341857,-0.478148457487225,
-0.894231261672206));
#18466=CARTESIAN_POINT('Ctrl Pts',(27.3100724995674,-0.629200057466457,
-0.786558893392617));
#18467=CARTESIAN_POINT('Ctrl Pts',(27.3061262548567,-0.669982979999203,
-0.752350761317609));
#18468=CARTESIAN_POINT('Ctrl Pts',(27.2975937907535,-0.754422366048413,
-0.668679633211809));
#18469=CARTESIAN_POINT('Ctrl Pts',(27.2930682902501,-0.796349974820793,
-0.617739935544105));
#18470=CARTESIAN_POINT('Ctrl Pts',(27.2828415758626,-0.879122103649902,
-0.494677808294302));
#18471=CARTESIAN_POINT('Ctrl Pts',(27.27710540015,-0.916911696347268,-0.420457326220017));
#18472=CARTESIAN_POINT('Ctrl Pts',(27.2642008684414,-0.977418418500146,
-0.254773622903383));
#18473=CARTESIAN_POINT('Ctrl Pts',(27.2545397745644,-1.01089657642268,-0.127082208364601));
#18474=CARTESIAN_POINT('Ctrl Pts',(27.2379084037118,-1.002202109097,0.115191605784107));
#18475=CARTESIAN_POINT('Ctrl Pts',(27.2322586174677,-0.989262746073459,
0.196801934931889));
#18476=CARTESIAN_POINT('Ctrl Pts',(27.2183588117237,-0.937186932251371,
0.380334639660224));
#18477=CARTESIAN_POINT('Ctrl Pts',(27.2086823458243,-0.885524725166168,
0.500766071236578));
#18478=CARTESIAN_POINT('Ctrl Pts',(27.1934790672189,-0.748776202161178,
0.675135895490028));
#18479=CARTESIAN_POINT('Ctrl Pts',(27.1885710133545,-0.698348939271822,
0.726855320763439));
#18480=CARTESIAN_POINT('Ctrl Pts',(27.1787772818171,-0.593528840519058,
0.814013154258869));
#18481=CARTESIAN_POINT('Ctrl Pts',(27.174009726289,-0.540026394969414,0.850601928307751));
#18482=CARTESIAN_POINT('Ctrl Pts',(27.1650329138941,-0.432715409844361,
0.90983782809936));
#18483=CARTESIAN_POINT('Ctrl Pts',(27.1608107122522,-0.379380989376285,
0.93355737677979));
#18484=CARTESIAN_POINT('Ctrl Pts',(27.1525700659823,-0.26797998648047,0.971452041509777));
#18485=CARTESIAN_POINT('Ctrl Pts',(27.1485518003818,-0.209998949928167,
0.985397384558026));
#18486=CARTESIAN_POINT('Ctrl Pts',(27.1397847329914,-0.0856608380001726,
1.00397337165135));
#18487=CARTESIAN_POINT('Ctrl Pts',(27.1350049237552,-0.0191006219463654,
1.00733745497235));
#18488=CARTESIAN_POINT('Ctrl Pts',(27.1253893832093,0.113181376821662,1.00125048035375));
#18489=CARTESIAN_POINT('Ctrl Pts',(27.120551622183,0.17897468945219,0.991827642205074));
#18490=CARTESIAN_POINT('Ctrl Pts',(27.105694488606,0.379768703194086,0.942345165306981));
#18491=CARTESIAN_POINT('Ctrl Pts',(27.0979105674963,0.482056046731077,0.886609333801805));
#18492=CARTESIAN_POINT('Ctrl Pts',(27.0825651562094,0.661963323035827,0.767793898264308));
#18493=CARTESIAN_POINT('Ctrl Pts',(27.0729859011291,0.757757849185879,0.674195878184252));
#18494=CARTESIAN_POINT('Ctrl Pts',(27.054263232748,0.905973775380077,0.457076143509283));
#18495=CARTESIAN_POINT('Ctrl Pts',(27.0455407361517,0.954259556577819,0.339816288159658));
#18496=CARTESIAN_POINT('Ctrl Pts',(27.0320144835362,0.9957262694812,0.154100298030815));
#18497=CARTESIAN_POINT('Ctrl Pts',(27.0272397936893,1.003935703847,0.0873954592435777));
#18498=CARTESIAN_POINT('Ctrl Pts',(27.0177717823106,1.00700302449346,-0.0444843111274326));
#18499=CARTESIAN_POINT('Ctrl Pts',(27.013044895658,1.00221469752981,-0.109729607703128));
#18500=CARTESIAN_POINT('Ctrl Pts',(26.9993758608286,0.968747071973493,-0.298252835788282));
#18501=CARTESIAN_POINT('Ctrl Pts',(26.9906629320194,0.922879088675033,-0.417883691589809));
#18502=CARTESIAN_POINT('Ctrl Pts',(26.9723583139129,0.788667222308375,-0.637735077391912));
#18503=CARTESIAN_POINT('Ctrl Pts',(26.9628426827107,0.701272403080465,-0.733523066314639));
#18504=CARTESIAN_POINT('Ctrl Pts',(26.945029819685,0.495705288711316,-0.883192578930708));
#18505=CARTESIAN_POINT('Ctrl Pts',(26.9367073299812,0.38396161494691,-0.937028583468894));
#18506=CARTESIAN_POINT('Ctrl Pts',(26.9234973859547,0.209548310468475,-0.985462237804072));
#18507=CARTESIAN_POINT('Ctrl Pts',(26.9190729775717,0.151198444492355,-0.996299134478789));
#18508=CARTESIAN_POINT('Ctrl Pts',(26.9107316961501,0.0364449296399151,
-1.00692734940693));
#18509=CARTESIAN_POINT('Ctrl Pts',(26.9068314082864,-0.0197150318892842,
-1.00720593274486));
#18510=CARTESIAN_POINT('Ctrl Pts',(26.8991961895396,-0.129935669177869,
-0.998606009375022));
#18511=CARTESIAN_POINT('Ctrl Pts',(26.8954498587092,-0.184115446692132,
-0.989914924496511));
#18512=CARTESIAN_POINT('Ctrl Pts',(26.8886420806066,-0.27860726670274,-0.966923747560494));
#18513=CARTESIAN_POINT('Ctrl Pts',(26.8856029715941,-0.319348681791324,
-0.954288572120448));
#18514=CARTESIAN_POINT('Ctrl Pts',(26.876278734407,-0.438581322083352,-0.908979279685783));
#18515=CARTESIAN_POINT('Ctrl Pts',(26.8677039954806,-0.542210751803785,
-0.858841061577955));
#18516=CARTESIAN_POINT('Ctrl Pts',(26.8540971674004,-0.692723890886937,
-0.731436714620663));
#18517=CARTESIAN_POINT('Ctrl Pts',(26.8501107762574,-0.734215447107898,
-0.689496080237736));
#18518=CARTESIAN_POINT('Ctrl Pts',(26.8411141794617,-0.816719544410732,
-0.590401558842806));
#18519=CARTESIAN_POINT('Ctrl Pts',(26.8359760088228,-0.856097745748887,
-0.531847235370042));
#18520=CARTESIAN_POINT('Ctrl Pts',(26.8242232810824,-0.930905847823687,
-0.391197353485646));
#18521=CARTESIAN_POINT('Ctrl Pts',(26.8182257784963,-0.959237421582567,
-0.313552337099464));
#18522=CARTESIAN_POINT('Ctrl Pts',(26.8084899505984,-0.9920819207877,-0.176839070096071));
#18523=CARTESIAN_POINT('Ctrl Pts',(26.8043316223949,-1.00083739890212,-0.115589566840668));
#18524=CARTESIAN_POINT('Ctrl Pts',(26.7958733475466,-1.00710165815903,0.00524138072349242));
#18525=CARTESIAN_POINT('Ctrl Pts',(26.791562957255,-1.0050070914625,0.0648276033447589));
#18526=CARTESIAN_POINT('Ctrl Pts',(26.7824246016789,-0.989835609104069,
0.188767362050434));
#18527=CARTESIAN_POINT('Ctrl Pts',(26.7775899504897,-0.975637924444642,
0.253039895424551));
#18528=CARTESIAN_POINT('Ctrl Pts',(26.7675145592988,-0.931932833192986,
0.386377020525932));
#18529=CARTESIAN_POINT('Ctrl Pts',(26.7624848873892,-0.900738489313069,
0.453879427471441));
#18530=CARTESIAN_POINT('Ctrl Pts',(26.7508247859445,-0.813764531387686,
0.597951517757357));
#18531=CARTESIAN_POINT('Ctrl Pts',(26.7439861045199,-0.753768829314911,
0.671792661606329));
#18532=CARTESIAN_POINT('Ctrl Pts',(26.732313158003,-0.63642527740879,0.781414580552255));
#18533=CARTESIAN_POINT('Ctrl Pts',(26.7274836783147,-0.583436919963472,
0.822051017128429));
#18534=CARTESIAN_POINT('Ctrl Pts',(26.7180391551223,-0.47022637164988,0.891900283266709));
#18535=CARTESIAN_POINT('Ctrl Pts',(26.7135120120417,-0.410507019943939,
0.920676426924196));
#18536=CARTESIAN_POINT('Ctrl Pts',(26.6996488614091,-0.225546255409973,
0.988430098645153));
#18537=CARTESIAN_POINT('Ctrl Pts',(26.6901311955291,-0.0935309357609265,
1.00955494059032));
#18538=CARTESIAN_POINT('Ctrl Pts',(26.6688743049094,0.202509412642327,0.999369048917218));
#18539=CARTESIAN_POINT('Ctrl Pts',(26.6595920452875,0.330583752256524,0.954406597362309));
#18540=CARTESIAN_POINT('Ctrl Pts',(26.6481896460982,0.477002107226659,0.88747520526504));
#18541=CARTESIAN_POINT('Ctrl Pts',(26.6434549358668,0.534926394103887,0.85384167615128));
#18542=CARTESIAN_POINT('Ctrl Pts',(26.6317093514896,0.668341736471132,0.757855225867808));
#18543=CARTESIAN_POINT('Ctrl Pts',(26.622097262116,0.769455365185776,0.669034510295732));
#18544=CARTESIAN_POINT('Ctrl Pts',(26.6014636705348,0.9227959351281,0.418879376339033));
#18545=CARTESIAN_POINT('Ctrl Pts',(26.5925615294449,0.969028638283612,0.296941886440832));
#18546=CARTESIAN_POINT('Ctrl Pts',(26.5797404230048,0.999437393194108,0.123541511218597));
#18547=CARTESIAN_POINT('Ctrl Pts',(26.5761718406925,1.00435207811376,0.0754448842792575));
#18548=CARTESIAN_POINT('Ctrl Pts',(26.5679515523816,1.00737329060242,-0.038667420070806));
#18549=CARTESIAN_POINT('Ctrl Pts',(26.5633693507695,1.0024200700062,-0.104585601058802));
#18550=CARTESIAN_POINT('Ctrl Pts',(26.5542249799062,0.979913496597944,-0.234360841833059));
#18551=CARTESIAN_POINT('Ctrl Pts',(26.549658364145,0.962336259399457,-0.298233941414874));
#18552=CARTESIAN_POINT('Ctrl Pts',(26.5393351018499,0.910634045058272,-0.43369640109639));
#18553=CARTESIAN_POINT('Ctrl Pts',(26.5334081765392,0.873884718327807,-0.504322181721031));
#18554=CARTESIAN_POINT('Ctrl Pts',(26.5222539995358,0.787577860226268,-0.630341976828754));
#18555=CARTESIAN_POINT('Ctrl Pts',(26.5171776069107,0.739341679098445,-0.685834840722942));
#18556=CARTESIAN_POINT('Ctrl Pts',(26.5071323384881,0.632397905463546,-0.78503152398032));
#18557=CARTESIAN_POINT('Ctrl Pts',(26.5021274264087,0.573559983600013,-0.828865420537326));
#18558=CARTESIAN_POINT('Ctrl Pts',(26.4913633348382,0.444814130765567,-0.905021459156498));
#18559=CARTESIAN_POINT('Ctrl Pts',(26.4855829862639,0.37441792388143,-0.936673453025792));
#18560=CARTESIAN_POINT('Ctrl Pts',(26.48,0.301306390501208,-0.959765445450967));
#18561=CARTESIAN_POINT('Ctrl Pts',(26.6174876988274,-1.08253756335566,0.624989939058213));
#18562=CARTESIAN_POINT('Ctrl Pts',(26.6118401171573,-1.03277812122718,0.711177670842943));
#18563=CARTESIAN_POINT('Ctrl Pts',(26.6059838000754,-0.972907071838,0.791109058417356));
#18564=CARTESIAN_POINT('Ctrl Pts',(26.5945079327168,-0.836620351594296,
0.93388751221825));
#18565=CARTESIAN_POINT('Ctrl Pts',(26.5889475836508,-0.760956332926198,
0.996507324316406));
#18566=CARTESIAN_POINT('Ctrl Pts',(26.579230377562,-0.615904061961894,1.09030505776182));
#18567=CARTESIAN_POINT('Ctrl Pts',(26.5750586406361,-0.549527520478794,
1.12522083031085));
#18568=CARTESIAN_POINT('Ctrl Pts',(26.5633658017298,-0.361940074516377,
1.2033170497122));
#18569=CARTESIAN_POINT('Ctrl Pts',(26.5557938111644,-0.236556154100087,
1.23410603940934));
#18570=CARTESIAN_POINT('Ctrl Pts',(26.54125785368,0.0171101028460626,1.25624490060463));
#18571=CARTESIAN_POINT('Ctrl Pts',(26.5343477764224,0.143836069469094,1.24810014955365));
#18572=CARTESIAN_POINT('Ctrl Pts',(26.5224569159616,0.345301590116501,1.20401890236638));
#18573=CARTESIAN_POINT('Ctrl Pts',(26.5177537241328,0.42159976540536,1.17946955919645));
#18574=CARTESIAN_POINT('Ctrl Pts',(26.5074861461494,0.583961520950492,1.10944536839998));
#18575=CARTESIAN_POINT('Ctrl Pts',(26.5019955497172,0.668138478073375,1.06088303115606));
#18576=CARTESIAN_POINT('Ctrl Pts',(26.4910936682112,0.823720462037962,0.945196959309205));
#18577=CARTESIAN_POINT('Ctrl Pts',(26.4856504306765,0.894565028502785,0.878444420944619));
#18578=CARTESIAN_POINT('Ctrl Pts',(26.48,0.956976228538287,0.80417442014319));
#18579=CARTESIAN_POINT('Origin',(26.48,0.,0.));
#18580=CARTESIAN_POINT('',(26.48,-1.082531754731,0.625));
#18581=CARTESIAN_POINT('',(26.48,-1.082531754731,0.625));
#18582=CARTESIAN_POINT('',(26.4799263573241,0.299169738002039,-0.960296952971633));
#18583=CARTESIAN_POINT('Ctrl Pts',(26.48,0.299165873930179,-0.960438829681521));
#18584=CARTESIAN_POINT('Ctrl Pts',(26.48,0.28312281539582,-0.965465660736469));
#18585=CARTESIAN_POINT('Ctrl Pts',(26.48,0.266819075223698,-0.970122449195917));
#18586=CARTESIAN_POINT('Ctrl Pts',(26.48,0.250214467165749,-0.974386330169429));
#18587=CARTESIAN_POINT('Ctrl Pts',(26.48,0.22635906714301,-0.980512134880837));
#18588=CARTESIAN_POINT('Ctrl Pts',(26.48,0.201882178115972,-0.985828929023409));
#18589=CARTESIAN_POINT('Ctrl Pts',(26.48,0.176676262857162,-0.990268554781819));
#18590=CARTESIAN_POINT('Ctrl Pts',(26.48,0.159925265242825,-0.993218979700894));
#18591=CARTESIAN_POINT('Ctrl Pts',(26.48,0.142852303253251,-0.995781004584336));
#18592=CARTESIAN_POINT('Ctrl Pts',(26.48,0.1254280189412,-0.997921901144576));
#18593=CARTESIAN_POINT('Ctrl Pts',(26.48,0.106806947823086,-1.00020984516516));
#18594=CARTESIAN_POINT('Ctrl Pts',(26.48,0.087776514520671,-1.0020162271941));
#18595=CARTESIAN_POINT('Ctrl Pts',(26.48,0.0683974909113733,-1.00328531223436));
#18596=CARTESIAN_POINT('Ctrl Pts',(26.48,0.0391293928497931,-1.00520200866632));
#18597=CARTESIAN_POINT('Ctrl Pts',(26.48,0.00906666890656565,-1.00589086154893));
#18598=CARTESIAN_POINT('Ctrl Pts',(26.48,-0.0215437351157509,-1.00519168337061));
#18599=CARTESIAN_POINT('Ctrl Pts',(26.48,-0.0481886343063174,-1.00458308205768));
#18600=CARTESIAN_POINT('Ctrl Pts',(26.48,-0.0752448170259378,-1.00292363113161));
#18601=CARTESIAN_POINT('Ctrl Pts',(26.48,-0.102542009190776,-1.00013317947925));
#18602=CARTESIAN_POINT('Ctrl Pts',(26.48,-0.131219127055196,-0.997201665115199));
#18603=CARTESIAN_POINT('Ctrl Pts',(26.48,-0.160161370119554,-0.993019741605458));
#18604=CARTESIAN_POINT('Ctrl Pts',(26.48,-0.189092775340995,-0.987540095371076));
#18605=CARTESIAN_POINT('Ctrl Pts',(26.48,-0.217536691483223,-0.98215278021003));
#18606=CARTESIAN_POINT('Ctrl Pts',(26.48,-0.245969377079973,-0.975511179037565));
#18607=CARTESIAN_POINT('Ctrl Pts',(26.48,-0.274127555915594,-0.967619521056985));
#18608=CARTESIAN_POINT('Ctrl Pts',(26.48,-0.290036541633927,-0.963160842289444));
#18609=CARTESIAN_POINT('Ctrl Pts',(26.48,-0.305854987209035,-0.958305057016084));
#18610=CARTESIAN_POINT('Ctrl Pts',(26.48,-0.321547816938486,-0.953056006990891));
#18611=CARTESIAN_POINT('Ctrl Pts',(26.48,-0.354061646781041,-0.94218054843456));
#18612=CARTESIAN_POINT('Ctrl Pts',(26.48,-0.386053020747235,-0.929613078171765));
#18613=CARTESIAN_POINT('Ctrl Pts',(26.48,-0.417347274845933,-0.91534542779146));
#18614=CARTESIAN_POINT('Ctrl Pts',(26.48,-0.443935398451674,-0.903223392523304));
#18615=CARTESIAN_POINT('Ctrl Pts',(26.48,-0.470020191345163,-0.889873838305286));
#18616=CARTESIAN_POINT('Ctrl Pts',(26.48,-0.495521901499934,-0.875357685473186));
#18617=CARTESIAN_POINT('Ctrl Pts',(26.48,-0.513450745658883,-0.865152180025328));
#18618=CARTESIAN_POINT('Ctrl Pts',(26.48,-0.531097296304518,-0.854365555490116));
#18619=CARTESIAN_POINT('Ctrl Pts',(26.48,-0.548395974066936,-0.843044270906004));
#18620=CARTESIAN_POINT('Ctrl Pts',(26.48,-0.57349785717507,-0.826616104189026));
#18621=CARTESIAN_POINT('Ctrl Pts',(26.48,-0.597861150258046,-0.809063033772212));
#18622=CARTESIAN_POINT('Ctrl Pts',(26.48,-0.621289762137012,-0.790576020950967));
#18623=CARTESIAN_POINT('Ctrl Pts',(26.48,-0.638271052917386,-0.777176450289253));
#18624=CARTESIAN_POINT('Ctrl Pts',(26.48,-0.654761904303153,-0.763287200299691));
#18625=CARTESIAN_POINT('Ctrl Pts',(26.48,-0.670699818177876,-0.748992955275881));
#18626=CARTESIAN_POINT('Ctrl Pts',(26.48,-0.685159587578794,-0.73602441444744));
#18627=CARTESIAN_POINT('Ctrl Pts',(26.48,-0.699159320961954,-0.722728245271615));
#18628=CARTESIAN_POINT('Ctrl Pts',(26.48,-0.712689959359925,-0.709142457287416));
#18629=CARTESIAN_POINT('Ctrl Pts',(26.48,-0.741675752047894,-0.680038521284534));
#18630=CARTESIAN_POINT('Ctrl Pts',(26.48,-0.768514174430042,-0.649603184718264));
#18631=CARTESIAN_POINT('Ctrl Pts',(26.48,-0.793165072752985,-0.61813614173595));
#18632=CARTESIAN_POINT('Ctrl Pts',(26.48,-0.804848277504714,-0.603222449696109));
#18633=CARTESIAN_POINT('Ctrl Pts',(26.48,-0.816040312388025,-0.588076248214693));
#18634=CARTESIAN_POINT('Ctrl Pts',(26.48,-0.826737803251188,-0.572725579677889));
#18635=CARTESIAN_POINT('Ctrl Pts',(26.48,-0.839252376721775,-0.554767436812069));
#18636=CARTESIAN_POINT('Ctrl Pts',(26.48,-0.851086810827611,-0.536538087002317));
#18637=CARTESIAN_POINT('Ctrl Pts',(26.48,-0.862283582369594,-0.517991203487763));
#18638=CARTESIAN_POINT('Ctrl Pts',(26.48,-0.875652514133851,-0.495846246862011));
#18639=CARTESIAN_POINT('Ctrl Pts',(26.48,-0.888114184637538,-0.473248637986891));
#18640=CARTESIAN_POINT('Ctrl Pts',(26.48,-0.899697335364076,-0.45008966299909));
#18641=CARTESIAN_POINT('Ctrl Pts',(26.48,-0.907516953536694,-0.434455372645004));
#18642=CARTESIAN_POINT('Ctrl Pts',(26.48,-0.914935139614922,-0.418564567576599));
#18643=CARTESIAN_POINT('Ctrl Pts',(26.48,-0.921961425695318,-0.402384956514707));
#18644=CARTESIAN_POINT('Ctrl Pts',(26.48,-0.927972444434527,-0.388543227872672));
#18645=CARTESIAN_POINT('Ctrl Pts',(26.48,-0.933698695491516,-0.374483334307272));
#18646=CARTESIAN_POINT('Ctrl Pts',(26.48,-0.939125947132214,-0.360221022028348));
#18647=CARTESIAN_POINT('Ctrl Pts',(26.48,-0.950750727055155,-0.329672182134602));
#18648=CARTESIAN_POINT('Ctrl Pts',(26.48,-0.960996612202744,-0.298202563482207));
#18649=CARTESIAN_POINT('Ctrl Pts',(26.48,-0.969723021334668,-0.266062967888056));
#18650=CARTESIAN_POINT('Ctrl Pts',(26.48,-0.976571193622196,-0.240840968259932));
#18651=CARTESIAN_POINT('Ctrl Pts',(26.48,-0.982484355231731,-0.215207226664101));
#18652=CARTESIAN_POINT('Ctrl Pts',(26.48,-0.987413304183645,-0.189294788555209));
#18653=CARTESIAN_POINT('Ctrl Pts',(26.48,-0.995623316750138,-0.146133164327012));
#18654=CARTESIAN_POINT('Ctrl Pts',(26.48,-1.00110756323152,-0.102194463140761));
#18655=CARTESIAN_POINT('Ctrl Pts',(26.48,-1.00372609935242,-0.057857128426423));
#18656=CARTESIAN_POINT('Ctrl Pts',(26.48,-1.00518150971684,-0.0332139638893522));
#18657=CARTESIAN_POINT('Ctrl Pts',(26.48,-1.00575153192558,-0.00844851123841294));
#18658=CARTESIAN_POINT('Ctrl Pts',(26.48,-1.00541187048368,0.0163701440036105));
#18659=CARTESIAN_POINT('Ctrl Pts',(26.48,-1.00518113428977,0.0332297616765972));
#18660=CARTESIAN_POINT('Ctrl Pts',(26.48,-1.00453040362454,0.0501168621315424));
#18661=CARTESIAN_POINT('Ctrl Pts',(26.48,-1.00345271164585,0.0669993261012208));
#18662=CARTESIAN_POINT('Ctrl Pts',(26.48,-1.00154962283086,0.0968119525153273));
#18663=CARTESIAN_POINT('Ctrl Pts',(26.48,-0.998312161314223,0.126597561590713));
#18664=CARTESIAN_POINT('Ctrl Pts',(26.48,-0.993741374083221,0.156094322123882));
#18665=CARTESIAN_POINT('Ctrl Pts',(26.48,-0.990679445388345,0.175853933087574));
#18666=CARTESIAN_POINT('Ctrl Pts',(26.48,-0.987020222988573,0.195483943145631));
#18667=CARTESIAN_POINT('Ctrl Pts',(26.48,-0.982776892962407,0.214908302908513));
#18668=CARTESIAN_POINT('Ctrl Pts',(26.48,-0.979330409756623,0.230684999345762));
#18669=CARTESIAN_POINT('Ctrl Pts',(26.48,-0.975498863804595,0.246325981007969));
#18670=CARTESIAN_POINT('Ctrl Pts',(26.48,-0.971306281242836,0.261795413288413));
#18671=CARTESIAN_POINT('Ctrl Pts',(26.48,-0.964182057014329,0.288081766062669));
#18672=CARTESIAN_POINT('Ctrl Pts',(26.48,-0.956018523881081,0.313881868010713));
#18673=CARTESIAN_POINT('Ctrl Pts',(26.48,-0.946844595399094,0.339276864237371));
#18674=CARTESIAN_POINT('Ctrl Pts',(26.48,-0.937561817050851,0.364973175429396));
#18675=CARTESIAN_POINT('Ctrl Pts',(26.48,-0.927244222465897,0.390255339892911));
#18676=CARTESIAN_POINT('Ctrl Pts',(26.48,-0.915871127948933,0.415191450231033));
#18677=CARTESIAN_POINT('Ctrl Pts',(26.48,-0.908944434263715,0.430378591932469));
#18678=CARTESIAN_POINT('Ctrl Pts',(26.48,-0.901625262147177,0.445437023251559));
#18679=CARTESIAN_POINT('Ctrl Pts',(26.48,-0.8939005627167,0.460377710173327));
#18680=CARTESIAN_POINT('Ctrl Pts',(26.48,0.301306390501209,-0.959765445450956));
#18681=CARTESIAN_POINT('Ctrl Pts',(26.4799732521317,0.300594091921396,-0.959942135954256));
#18682=CARTESIAN_POINT('Ctrl Pts',(26.4799465042634,0.299881646280774,-0.960118045048617));
#18683=CARTESIAN_POINT('Ctrl Pts',(26.4799197563952,0.299169055382355,-0.960293172620655));
#18684=CARTESIAN_POINT('Origin',(26.48,0.,0.));
#18685=CARTESIAN_POINT('Origin',(26.48,-1.082531754731,0.625));
#18686=CARTESIAN_POINT('',(26.48,-1.082531754731,0.625));
#18687=CARTESIAN_POINT('Origin',(32.48,0.,0.));
#18688=CARTESIAN_POINT('Ctrl Pts',(28.05053792796,0.4083111129797,-0.9194117875127));
#18689=CARTESIAN_POINT('Ctrl Pts',(28.03432447383,0.2001723500546,-1.011846288678));
#18690=CARTESIAN_POINT('Ctrl Pts',(28.00189756559,-0.2804297640578,-1.049445986524));
#18691=CARTESIAN_POINT('Ctrl Pts',(27.95325720323,-0.8775530509839,-0.6404167031148));
#18692=CARTESIAN_POINT('Ctrl Pts',(27.90461684086,-1.085053538068,0.05289845296993));
#18693=CARTESIAN_POINT('Ctrl Pts',(27.85597647849,-0.8110736778472,0.722716801219));
#18694=CARTESIAN_POINT('Ctrl Pts',(27.80733611613,-0.1771401075638,1.071811347771));
#18695=CARTESIAN_POINT('Ctrl Pts',(27.75869575376,0.5354018004738,0.9452525615612));
#18696=CARTESIAN_POINT('Ctrl Pts',(27.7100553914,1.010342345254,0.3992070424407));
#18697=CARTESIAN_POINT('Ctrl Pts',(27.66141502903,1.036909749886,-0.3239999391312));
#18698=CARTESIAN_POINT('Ctrl Pts',(27.61277466667,0.6033141627449,-0.9034211828672));
#18699=CARTESIAN_POINT('Ctrl Pts',(27.5641343043,-0.09802209198353,-1.081919350877));
#18700=CARTESIAN_POINT('Ctrl Pts',(27.51549394194,-0.7558577907832,-0.7802799567664));
#18701=CARTESIAN_POINT('Ctrl Pts',(27.46685357957,-1.078256551794,-0.1323654788032));
#18702=CARTESIAN_POINT('Ctrl Pts',(27.41821321721,-0.9221432409161,0.5742905662964));
#18703=CARTESIAN_POINT('Ctrl Pts',(27.36957285484,-0.3567983129049,1.026086144158));
#18704=CARTESIAN_POINT('Ctrl Pts',(27.32093249248,0.3668876885504,1.022521997474));
#18705=CARTESIAN_POINT('Ctrl Pts',(27.27229213011,0.9277551218377,0.5651798344144));
#18706=CARTESIAN_POINT('Ctrl Pts',(27.22365176775,1.076900479802,-0.1429796066949));
#18707=CARTESIAN_POINT('Ctrl Pts',(27.17501140538,0.7481355680915,-0.7876871098868));
#18708=CARTESIAN_POINT('Ctrl Pts',(27.12637104301,0.08736070952101,-1.082832359018));
#18709=CARTESIAN_POINT('Ctrl Pts',(27.07773068065,-0.6121833585662,-0.8974348705957));
#18710=CARTESIAN_POINT('Ctrl Pts',(27.02909031828,-1.040050777064,-0.3137709227251));
#18711=CARTESIAN_POINT('Ctrl Pts',(26.98044995592,-1.006361203543,0.4091392676381));
#18712=CARTESIAN_POINT('Ctrl Pts',(26.93180959355,-0.5260654973531,0.9504803549345));
#18713=CARTESIAN_POINT('Ctrl Pts',(26.88316923119,0.1876891886185,1.07001427955));
#18714=CARTESIAN_POINT('Ctrl Pts',(26.83452886882,0.8181506349976,0.7146939595389));
#18715=CARTESIAN_POINT('Ctrl Pts',(26.78588850646,1.08553041707,0.04220434462485));
#18716=CARTESIAN_POINT('Ctrl Pts',(26.73724814409,0.8711708986611,-0.6490142126668));
#18717=CARTESIAN_POINT('Ctrl Pts',(26.68860778173,0.2701974812614,-1.052213574699));
#18718=CARTESIAN_POINT('Ctrl Pts',(26.63996741936,-0.4506740207088,-0.9884494695529));
#18719=CARTESIAN_POINT('Ctrl Pts',(26.591327057,-0.971585047505,-0.4860611138367));
#18720=CARTESIAN_POINT('Ctrl Pts',(26.54268669463,-1.061169801454,0.2321559469013));
#18721=CARTESIAN_POINT('Ctrl Pts',(26.51025978639,-0.8073213367869,0.641976744755));
#18722=CARTESIAN_POINT('Ctrl Pts',(26.49404633227,-0.6297166412204,0.7845335886819));
#18723=CARTESIAN_POINT('Ctrl Pts',(27.96513432978,0.4083111129797,-0.9194117875127));
#18724=CARTESIAN_POINT('Ctrl Pts',(27.94892087565,0.2001723500546,-1.011846288678));
#18725=CARTESIAN_POINT('Ctrl Pts',(27.91649396741,-0.2804297640578,-1.049445986524));
#18726=CARTESIAN_POINT('Ctrl Pts',(27.86785360505,-0.8775530509839,-0.6404167031148));
#18727=CARTESIAN_POINT('Ctrl Pts',(27.81921324268,-1.085053538068,0.05289845296993));
#18728=CARTESIAN_POINT('Ctrl Pts',(27.77057288031,-0.8110736778472,0.722716801219));
#18729=CARTESIAN_POINT('Ctrl Pts',(27.72193251795,-0.1771401075638,1.071811347771));
#18730=CARTESIAN_POINT('Ctrl Pts',(27.67329215558,0.5354018004738,0.9452525615612));
#18731=CARTESIAN_POINT('Ctrl Pts',(27.62465179322,1.010342345254,0.3992070424407));
#18732=CARTESIAN_POINT('Ctrl Pts',(27.57601143085,1.036909749886,-0.3239999391312));
#18733=CARTESIAN_POINT('Ctrl Pts',(27.52737106849,0.6033141627449,-0.9034211828672));
#18734=CARTESIAN_POINT('Ctrl Pts',(27.47873070612,-0.09802209198353,-1.081919350877));
#18735=CARTESIAN_POINT('Ctrl Pts',(27.43009034376,-0.7558577907832,-0.7802799567664));
#18736=CARTESIAN_POINT('Ctrl Pts',(27.38144998139,-1.078256551794,-0.1323654788032));
#18737=CARTESIAN_POINT('Ctrl Pts',(27.33280961903,-0.9221432409161,0.5742905662964));
#18738=CARTESIAN_POINT('Ctrl Pts',(27.28416925666,-0.3567983129049,1.026086144158));
#18739=CARTESIAN_POINT('Ctrl Pts',(27.2355288943,0.3668876885504,1.022521997474));
#18740=CARTESIAN_POINT('Ctrl Pts',(27.18688853193,0.9277551218377,0.5651798344144));
#18741=CARTESIAN_POINT('Ctrl Pts',(27.13824816957,1.076900479802,-0.1429796066949));
#18742=CARTESIAN_POINT('Ctrl Pts',(27.0896078072,0.7481355680915,-0.7876871098868));
#18743=CARTESIAN_POINT('Ctrl Pts',(27.04096744483,0.08736070952101,-1.082832359018));
#18744=CARTESIAN_POINT('Ctrl Pts',(26.99232708247,-0.6121833585662,-0.8974348705957));
#18745=CARTESIAN_POINT('Ctrl Pts',(26.9436867201,-1.040050777064,-0.3137709227251));
#18746=CARTESIAN_POINT('Ctrl Pts',(26.89504635774,-1.006361203543,0.4091392676381));
#18747=CARTESIAN_POINT('Ctrl Pts',(26.84640599537,-0.5260654973531,0.9504803549345));
#18748=CARTESIAN_POINT('Ctrl Pts',(26.79776563301,0.1876891886185,1.07001427955));
#18749=CARTESIAN_POINT('Ctrl Pts',(26.74912527064,0.8181506349976,0.7146939595389));
#18750=CARTESIAN_POINT('Ctrl Pts',(26.70048490828,1.08553041707,0.04220434462485));
#18751=CARTESIAN_POINT('Ctrl Pts',(26.65184454591,0.8711708986611,-0.6490142126668));
#18752=CARTESIAN_POINT('Ctrl Pts',(26.60320418355,0.2701974812614,-1.052213574699));
#18753=CARTESIAN_POINT('Ctrl Pts',(26.55456382118,-0.4506740207088,-0.9884494695529));
#18754=CARTESIAN_POINT('Ctrl Pts',(26.50592345882,-0.971585047505,-0.4860611138367));
#18755=CARTESIAN_POINT('Ctrl Pts',(26.45728309645,-1.061169801454,0.2321559469013));
#18756=CARTESIAN_POINT('Ctrl Pts',(26.42485618821,-0.8073213367869,0.641976744755));
#18757=CARTESIAN_POINT('Ctrl Pts',(26.40864273409,-0.6297166412204,0.7845335886819));
#18758=CARTESIAN_POINT('Ctrl Pts',(27.8797307316,0.4083111129797,-0.9194117875127));
#18759=CARTESIAN_POINT('Ctrl Pts',(27.86351727747,0.2001723500546,-1.011846288678));
#18760=CARTESIAN_POINT('Ctrl Pts',(27.83109036923,-0.2804297640578,-1.049445986524));
#18761=CARTESIAN_POINT('Ctrl Pts',(27.78245000687,-0.8775530509839,-0.6404167031148));
#18762=CARTESIAN_POINT('Ctrl Pts',(27.7338096445,-1.085053538068,0.05289845296993));
#18763=CARTESIAN_POINT('Ctrl Pts',(27.68516928214,-0.8110736778472,0.722716801219));
#18764=CARTESIAN_POINT('Ctrl Pts',(27.63652891977,-0.1771401075638,1.071811347771));
#18765=CARTESIAN_POINT('Ctrl Pts',(27.5878885574,0.5354018004738,0.9452525615612));
#18766=CARTESIAN_POINT('Ctrl Pts',(27.53924819504,1.010342345254,0.3992070424407));
#18767=CARTESIAN_POINT('Ctrl Pts',(27.49060783267,1.036909749886,-0.3239999391312));
#18768=CARTESIAN_POINT('Ctrl Pts',(27.44196747031,0.6033141627449,-0.9034211828672));
#18769=CARTESIAN_POINT('Ctrl Pts',(27.39332710794,-0.09802209198353,-1.081919350877));
#18770=CARTESIAN_POINT('Ctrl Pts',(27.34468674558,-0.7558577907832,-0.7802799567664));
#18771=CARTESIAN_POINT('Ctrl Pts',(27.29604638321,-1.078256551794,-0.1323654788032));
#18772=CARTESIAN_POINT('Ctrl Pts',(27.24740602085,-0.9221432409161,0.5742905662964));
#18773=CARTESIAN_POINT('Ctrl Pts',(27.19876565848,-0.3567983129049,1.026086144158));
#18774=CARTESIAN_POINT('Ctrl Pts',(27.15012529612,0.3668876885504,1.022521997474));
#18775=CARTESIAN_POINT('Ctrl Pts',(27.10148493375,0.9277551218377,0.5651798344144));
#18776=CARTESIAN_POINT('Ctrl Pts',(27.05284457139,1.076900479802,-0.1429796066949));
#18777=CARTESIAN_POINT('Ctrl Pts',(27.00420420902,0.7481355680915,-0.7876871098868));
#18778=CARTESIAN_POINT('Ctrl Pts',(26.95556384666,0.08736070952101,-1.082832359018));
#18779=CARTESIAN_POINT('Ctrl Pts',(26.90692348429,-0.6121833585662,-0.8974348705957));
#18780=CARTESIAN_POINT('Ctrl Pts',(26.85828312192,-1.040050777064,-0.3137709227251));
#18781=CARTESIAN_POINT('Ctrl Pts',(26.80964275956,-1.006361203543,0.4091392676381));
#18782=CARTESIAN_POINT('Ctrl Pts',(26.76100239719,-0.5260654973531,0.9504803549345));
#18783=CARTESIAN_POINT('Ctrl Pts',(26.71236203483,0.1876891886185,1.07001427955));
#18784=CARTESIAN_POINT('Ctrl Pts',(26.66372167246,0.8181506349976,0.7146939595389));
#18785=CARTESIAN_POINT('Ctrl Pts',(26.6150813101,1.08553041707,0.04220434462485));
#18786=CARTESIAN_POINT('Ctrl Pts',(26.56644094773,0.8711708986611,-0.6490142126668));
#18787=CARTESIAN_POINT('Ctrl Pts',(26.51780058537,0.2701974812614,-1.052213574699));
#18788=CARTESIAN_POINT('Ctrl Pts',(26.469160223,-0.4506740207088,-0.9884494695529));
#18789=CARTESIAN_POINT('Ctrl Pts',(26.42051986064,-0.971585047505,-0.4860611138367));
#18790=CARTESIAN_POINT('Ctrl Pts',(26.37187949827,-1.061169801454,0.2321559469013));
#18791=CARTESIAN_POINT('Ctrl Pts',(26.33945259003,-0.8073213367869,0.641976744755));
#18792=CARTESIAN_POINT('Ctrl Pts',(26.32323913591,-0.6297166412204,0.7845335886819));
#18793=CARTESIAN_POINT('Ctrl Pts',(27.79432713342,0.4083111129797,-0.9194117875127));
#18794=CARTESIAN_POINT('Ctrl Pts',(27.7781136793,0.2001723500546,-1.011846288678));
#18795=CARTESIAN_POINT('Ctrl Pts',(27.74568677105,-0.2804297640578,-1.049445986524));
#18796=CARTESIAN_POINT('Ctrl Pts',(27.69704640869,-0.8775530509839,-0.6404167031148));
#18797=CARTESIAN_POINT('Ctrl Pts',(27.64840604632,-1.085053538068,0.05289845296993));
#18798=CARTESIAN_POINT('Ctrl Pts',(27.59976568396,-0.8110736778472,0.722716801219));
#18799=CARTESIAN_POINT('Ctrl Pts',(27.55112532159,-0.1771401075638,1.071811347771));
#18800=CARTESIAN_POINT('Ctrl Pts',(27.50248495923,0.5354018004738,0.9452525615612));
#18801=CARTESIAN_POINT('Ctrl Pts',(27.45384459686,1.010342345254,0.3992070424407));
#18802=CARTESIAN_POINT('Ctrl Pts',(27.40520423449,1.036909749886,-0.3239999391312));
#18803=CARTESIAN_POINT('Ctrl Pts',(27.35656387213,0.6033141627449,-0.9034211828672));
#18804=CARTESIAN_POINT('Ctrl Pts',(27.30792350976,-0.09802209198353,-1.081919350877));
#18805=CARTESIAN_POINT('Ctrl Pts',(27.2592831474,-0.7558577907832,-0.7802799567664));
#18806=CARTESIAN_POINT('Ctrl Pts',(27.21064278503,-1.078256551794,-0.1323654788032));
#18807=CARTESIAN_POINT('Ctrl Pts',(27.16200242267,-0.9221432409161,0.5742905662964));
#18808=CARTESIAN_POINT('Ctrl Pts',(27.1133620603,-0.3567983129049,1.026086144158));
#18809=CARTESIAN_POINT('Ctrl Pts',(27.06472169794,0.3668876885504,1.022521997474));
#18810=CARTESIAN_POINT('Ctrl Pts',(27.01608133557,0.9277551218377,0.5651798344144));
#18811=CARTESIAN_POINT('Ctrl Pts',(26.96744097321,1.076900479802,-0.1429796066949));
#18812=CARTESIAN_POINT('Ctrl Pts',(26.91880061084,0.7481355680915,-0.7876871098868));
#18813=CARTESIAN_POINT('Ctrl Pts',(26.87016024848,0.08736070952101,-1.082832359018));
#18814=CARTESIAN_POINT('Ctrl Pts',(26.82151988611,-0.6121833585662,-0.8974348705957));
#18815=CARTESIAN_POINT('Ctrl Pts',(26.77287952375,-1.040050777064,-0.3137709227251));
#18816=CARTESIAN_POINT('Ctrl Pts',(26.72423916138,-1.006361203543,0.4091392676381));
#18817=CARTESIAN_POINT('Ctrl Pts',(26.67559879901,-0.5260654973531,0.9504803549345));
#18818=CARTESIAN_POINT('Ctrl Pts',(26.62695843665,0.1876891886185,1.07001427955));
#18819=CARTESIAN_POINT('Ctrl Pts',(26.57831807428,0.8181506349976,0.7146939595389));
#18820=CARTESIAN_POINT('Ctrl Pts',(26.52967771192,1.08553041707,0.04220434462485));
#18821=CARTESIAN_POINT('Ctrl Pts',(26.48103734955,0.8711708986611,-0.6490142126668));
#18822=CARTESIAN_POINT('Ctrl Pts',(26.43239698719,0.2701974812614,-1.052213574699));
#18823=CARTESIAN_POINT('Ctrl Pts',(26.38375662482,-0.4506740207088,-0.9884494695529));
#18824=CARTESIAN_POINT('Ctrl Pts',(26.33511626246,-0.971585047505,-0.4860611138367));
#18825=CARTESIAN_POINT('Ctrl Pts',(26.28647590009,-1.061169801454,0.2321559469013));
#18826=CARTESIAN_POINT('Ctrl Pts',(26.25404899185,-0.8073213367869,0.641976744755));
#18827=CARTESIAN_POINT('Ctrl Pts',(26.23783553773,-0.6297166412204,0.7845335886819));
#18828=CARTESIAN_POINT('',(27.97662653432,-3.364114380046E-14,-1.006));
#18829=CARTESIAN_POINT('Ctrl Pts',(29.55060539727,0.5913119638062,0.8138710963412));
#18830=CARTESIAN_POINT('Ctrl Pts',(29.53435539727,0.7759734579399,0.6797066675681));
#18831=CARTESIAN_POINT('Ctrl Pts',(29.50185539727,1.049589852444,0.2813441556141));
#18832=CARTESIAN_POINT('Ctrl Pts',(29.45310539727,0.9928036170159,-0.4420327897627));
#18833=CARTESIAN_POINT('Ctrl Pts',(29.40435539727,0.4933560618227,-0.9682753741689));
#18834=CARTESIAN_POINT('Ctrl Pts',(29.35560539727,-0.2259412078788,-1.062981093563));
#18835=CARTESIAN_POINT('Ctrl Pts',(29.30685539727,-0.8445461960836,-0.6838991696093));
#18836=CARTESIAN_POINT('Ctrl Pts',(29.25810539727,-1.086727031141,-1.08376590563E-7));
#18837=CARTESIAN_POINT('Ctrl Pts',(29.20935539727,-0.8445456793518,0.6838996031158));
#18838=CARTESIAN_POINT('Ctrl Pts',(29.16060539727,-0.2259432748058,1.06297957629));
#18839=CARTESIAN_POINT('Ctrl Pts',(29.11185539727,0.4933638127993,0.9682810097529));
#18840=CARTESIAN_POINT('Ctrl Pts',(29.06310539727,0.9927746800368,0.4420117646993));
#18841=CARTESIAN_POINT('Ctrl Pts',(29.01435539727,1.049697849384,-0.2812656909448));
#18842=CARTESIAN_POINT('Ctrl Pts',(28.96560539727,0.6387622099061,-0.8791807571591));
#18843=CARTESIAN_POINT('Ctrl Pts',(28.91685539727,-0.05687490617148,-1.085237858466));
#18844=CARTESIAN_POINT('Ctrl Pts',(28.86810539727,-0.7271624171027,-0.807595680755));
#18845=CARTESIAN_POINT('Ctrl Pts',(28.81935539727,-1.0733477654,-0.1700015850954));
#18846=CARTESIAN_POINT('Ctrl Pts',(28.77060539727,-0.9411333451298,0.5433635901541));
#18847=CARTESIAN_POINT('Ctrl Pts',(28.72185539727,-0.3894481913236,1.014547224479));
#18848=CARTESIAN_POINT('Ctrl Pts',(28.67310539727,0.3358171669691,1.033538966266));
#18849=CARTESIAN_POINT('Ctrl Pts',(28.62435539727,0.9114061014946,0.5918740428154));
#18850=CARTESIAN_POINT('Ctrl Pts',(28.57560539727,1.080773975171,-0.1135939221767));
#18851=CARTESIAN_POINT('Ctrl Pts',(28.52685539727,0.7684321582634,-0.7684321583925));
#18852=CARTESIAN_POINT('Ctrl Pts',(28.47810539727,0.1135939230171,-1.080773975495));
#18853=CARTESIAN_POINT('Ctrl Pts',(28.42935539727,-0.5918740460484,-0.9114061000685));
#18854=CARTESIAN_POINT('Ctrl Pts',(28.38060539727,-1.033538954174,-0.3358171723489));
#18855=CARTESIAN_POINT('Ctrl Pts',(28.33185539727,-1.014547269612,0.3894482114172));
#18856=CARTESIAN_POINT('Ctrl Pts',(28.28310539727,-0.5433634217136,0.9411332701358));
#18857=CARTESIAN_POINT('Ctrl Pts',(28.23435539727,0.170000956467,1.073348045283));
#18858=CARTESIAN_POINT('Ctrl Pts',(28.18560539727,0.8075980268285,0.7271613725661));
#18859=CARTESIAN_POINT('Ctrl Pts',(28.13685539727,1.0852291028,0.05687880443492));
#18860=CARTESIAN_POINT('Ctrl Pts',(28.08810539727,0.8792134337481,-0.6387767584236));
#18861=CARTESIAN_POINT('Ctrl Pts',(28.03935539727,0.281143740254,-1.049643553578));
#18862=CARTESIAN_POINT('Ctrl Pts',(28.00685539727,-0.2006565122658,-1.011866061022));
#18863=CARTESIAN_POINT('Ctrl Pts',(27.99060539727,-0.4091770629343,-0.9190267303884));
#18864=CARTESIAN_POINT('Ctrl Pts',(29.46520179909,0.5913119638062,0.8138710963412));
#18865=CARTESIAN_POINT('Ctrl Pts',(29.44895179909,0.7759734579399,0.6797066675681));
#18866=CARTESIAN_POINT('Ctrl Pts',(29.41645179909,1.049589852444,0.2813441556141));
#18867=CARTESIAN_POINT('Ctrl Pts',(29.36770179909,0.9928036170159,-0.4420327897627));
#18868=CARTESIAN_POINT('Ctrl Pts',(29.31895179909,0.4933560618227,-0.9682753741689));
#18869=CARTESIAN_POINT('Ctrl Pts',(29.27020179909,-0.2259412078788,-1.062981093563));
#18870=CARTESIAN_POINT('Ctrl Pts',(29.22145179909,-0.8445461960836,-0.6838991696093));
#18871=CARTESIAN_POINT('Ctrl Pts',(29.17270179909,-1.086727031141,-1.08376590563E-7));
#18872=CARTESIAN_POINT('Ctrl Pts',(29.12395179909,-0.8445456793518,0.6838996031158));
#18873=CARTESIAN_POINT('Ctrl Pts',(29.07520179909,-0.2259432748058,1.06297957629));
#18874=CARTESIAN_POINT('Ctrl Pts',(29.02645179909,0.4933638127993,0.9682810097529));
#18875=CARTESIAN_POINT('Ctrl Pts',(28.97770179909,0.9927746800368,0.4420117646993));
#18876=CARTESIAN_POINT('Ctrl Pts',(28.92895179909,1.049697849384,-0.2812656909448));
#18877=CARTESIAN_POINT('Ctrl Pts',(28.88020179909,0.6387622099061,-0.8791807571591));
#18878=CARTESIAN_POINT('Ctrl Pts',(28.83145179909,-0.05687490617148,-1.085237858466));
#18879=CARTESIAN_POINT('Ctrl Pts',(28.78270179909,-0.7271624171027,-0.807595680755));
#18880=CARTESIAN_POINT('Ctrl Pts',(28.73395179909,-1.0733477654,-0.1700015850954));
#18881=CARTESIAN_POINT('Ctrl Pts',(28.68520179909,-0.9411333451298,0.5433635901541));
#18882=CARTESIAN_POINT('Ctrl Pts',(28.63645179909,-0.3894481913236,1.014547224479));
#18883=CARTESIAN_POINT('Ctrl Pts',(28.58770179909,0.3358171669691,1.033538966266));
#18884=CARTESIAN_POINT('Ctrl Pts',(28.53895179909,0.9114061014946,0.5918740428154));
#18885=CARTESIAN_POINT('Ctrl Pts',(28.49020179909,1.080773975171,-0.1135939221767));
#18886=CARTESIAN_POINT('Ctrl Pts',(28.44145179909,0.7684321582634,-0.7684321583925));
#18887=CARTESIAN_POINT('Ctrl Pts',(28.39270179909,0.1135939230171,-1.080773975495));
#18888=CARTESIAN_POINT('Ctrl Pts',(28.34395179909,-0.5918740460484,-0.9114061000685));
#18889=CARTESIAN_POINT('Ctrl Pts',(28.29520179909,-1.033538954174,-0.3358171723489));
#18890=CARTESIAN_POINT('Ctrl Pts',(28.24645179909,-1.014547269612,0.3894482114172));
#18891=CARTESIAN_POINT('Ctrl Pts',(28.19770179909,-0.5433634217136,0.9411332701358));
#18892=CARTESIAN_POINT('Ctrl Pts',(28.14895179909,0.170000956467,1.073348045283));
#18893=CARTESIAN_POINT('Ctrl Pts',(28.10020179909,0.8075980268285,0.7271613725661));
#18894=CARTESIAN_POINT('Ctrl Pts',(28.05145179909,1.0852291028,0.05687880443492));
#18895=CARTESIAN_POINT('Ctrl Pts',(28.00270179909,0.8792134337481,-0.6387767584236));
#18896=CARTESIAN_POINT('Ctrl Pts',(27.95395179909,0.281143740254,-1.049643553578));
#18897=CARTESIAN_POINT('Ctrl Pts',(27.92145179909,-0.2006565122658,-1.011866061022));
#18898=CARTESIAN_POINT('Ctrl Pts',(27.90520179909,-0.4091770629343,-0.9190267303884));
#18899=CARTESIAN_POINT('Ctrl Pts',(29.37979820091,0.5913119638062,0.8138710963412));
#18900=CARTESIAN_POINT('Ctrl Pts',(29.36354820091,0.7759734579399,0.6797066675681));
#18901=CARTESIAN_POINT('Ctrl Pts',(29.33104820091,1.049589852444,0.2813441556141));
#18902=CARTESIAN_POINT('Ctrl Pts',(29.28229820091,0.9928036170159,-0.4420327897627));
#18903=CARTESIAN_POINT('Ctrl Pts',(29.23354820091,0.4933560618227,-0.9682753741689));
#18904=CARTESIAN_POINT('Ctrl Pts',(29.18479820091,-0.2259412078788,-1.062981093563));
#18905=CARTESIAN_POINT('Ctrl Pts',(29.13604820091,-0.8445461960836,-0.6838991696093));
#18906=CARTESIAN_POINT('Ctrl Pts',(29.08729820091,-1.086727031141,-1.083765901744E-7));
#18907=CARTESIAN_POINT('Ctrl Pts',(29.03854820091,-0.8445456793518,0.6838996031158));
#18908=CARTESIAN_POINT('Ctrl Pts',(28.98979820091,-0.2259432748058,1.06297957629));
#18909=CARTESIAN_POINT('Ctrl Pts',(28.94104820091,0.4933638127993,0.9682810097529));
#18910=CARTESIAN_POINT('Ctrl Pts',(28.89229820091,0.9927746800368,0.4420117646993));
#18911=CARTESIAN_POINT('Ctrl Pts',(28.84354820091,1.049697849384,-0.2812656909448));
#18912=CARTESIAN_POINT('Ctrl Pts',(28.79479820091,0.6387622099061,-0.8791807571591));
#18913=CARTESIAN_POINT('Ctrl Pts',(28.74604820091,-0.05687490617148,-1.085237858466));
#18914=CARTESIAN_POINT('Ctrl Pts',(28.69729820091,-0.7271624171027,-0.807595680755));
#18915=CARTESIAN_POINT('Ctrl Pts',(28.64854820091,-1.0733477654,-0.1700015850954));
#18916=CARTESIAN_POINT('Ctrl Pts',(28.59979820091,-0.9411333451298,0.5433635901541));
#18917=CARTESIAN_POINT('Ctrl Pts',(28.55104820091,-0.3894481913236,1.014547224479));
#18918=CARTESIAN_POINT('Ctrl Pts',(28.50229820091,0.3358171669691,1.033538966266));
#18919=CARTESIAN_POINT('Ctrl Pts',(28.45354820091,0.9114061014946,0.5918740428154));
#18920=CARTESIAN_POINT('Ctrl Pts',(28.40479820091,1.080773975171,-0.1135939221767));
#18921=CARTESIAN_POINT('Ctrl Pts',(28.35604820091,0.7684321582634,-0.7684321583925));
#18922=CARTESIAN_POINT('Ctrl Pts',(28.30729820091,0.1135939230171,-1.080773975495));
#18923=CARTESIAN_POINT('Ctrl Pts',(28.25854820091,-0.5918740460484,-0.9114061000685));
#18924=CARTESIAN_POINT('Ctrl Pts',(28.20979820091,-1.033538954174,-0.3358171723489));
#18925=CARTESIAN_POINT('Ctrl Pts',(28.16104820091,-1.014547269612,0.3894482114172));
#18926=CARTESIAN_POINT('Ctrl Pts',(28.11229820091,-0.5433634217136,0.9411332701358));
#18927=CARTESIAN_POINT('Ctrl Pts',(28.06354820091,0.170000956467,1.073348045283));
#18928=CARTESIAN_POINT('Ctrl Pts',(28.01479820091,0.8075980268285,0.7271613725661));
#18929=CARTESIAN_POINT('Ctrl Pts',(27.96604820091,1.0852291028,0.05687880443492));
#18930=CARTESIAN_POINT('Ctrl Pts',(27.91729820091,0.8792134337481,-0.6387767584236));
#18931=CARTESIAN_POINT('Ctrl Pts',(27.86854820091,0.281143740254,-1.049643553578));
#18932=CARTESIAN_POINT('Ctrl Pts',(27.83604820091,-0.2006565122658,-1.011866061022));
#18933=CARTESIAN_POINT('Ctrl Pts',(27.81979820091,-0.4091770629343,-0.9190267303884));
#18934=CARTESIAN_POINT('Ctrl Pts',(29.29439460273,0.5913119638062,0.8138710963412));
#18935=CARTESIAN_POINT('Ctrl Pts',(29.27814460273,0.7759734579399,0.6797066675681));
#18936=CARTESIAN_POINT('Ctrl Pts',(29.24564460273,1.049589852444,0.2813441556141));
#18937=CARTESIAN_POINT('Ctrl Pts',(29.19689460273,0.9928036170159,-0.4420327897627));
#18938=CARTESIAN_POINT('Ctrl Pts',(29.14814460273,0.4933560618227,-0.9682753741689));
#18939=CARTESIAN_POINT('Ctrl Pts',(29.09939460273,-0.2259412078788,-1.062981093563));
#18940=CARTESIAN_POINT('Ctrl Pts',(29.05064460273,-0.8445461960836,-0.6838991696093));
#18941=CARTESIAN_POINT('Ctrl Pts',(29.00189460273,-1.086727031141,-1.083765901744E-7));
#18942=CARTESIAN_POINT('Ctrl Pts',(28.95314460273,-0.8445456793518,0.6838996031158));
#18943=CARTESIAN_POINT('Ctrl Pts',(28.90439460273,-0.2259432748058,1.06297957629));
#18944=CARTESIAN_POINT('Ctrl Pts',(28.85564460273,0.4933638127993,0.9682810097529));
#18945=CARTESIAN_POINT('Ctrl Pts',(28.80689460273,0.9927746800368,0.4420117646993));
#18946=CARTESIAN_POINT('Ctrl Pts',(28.75814460273,1.049697849384,-0.2812656909448));
#18947=CARTESIAN_POINT('Ctrl Pts',(28.70939460273,0.6387622099061,-0.8791807571591));
#18948=CARTESIAN_POINT('Ctrl Pts',(28.66064460273,-0.05687490617148,-1.085237858466));
#18949=CARTESIAN_POINT('Ctrl Pts',(28.61189460273,-0.7271624171027,-0.807595680755));
#18950=CARTESIAN_POINT('Ctrl Pts',(28.56314460273,-1.0733477654,-0.1700015850954));
#18951=CARTESIAN_POINT('Ctrl Pts',(28.51439460273,-0.9411333451298,0.5433635901541));
#18952=CARTESIAN_POINT('Ctrl Pts',(28.46564460273,-0.3894481913236,1.014547224479));
#18953=CARTESIAN_POINT('Ctrl Pts',(28.41689460273,0.3358171669691,1.033538966266));
#18954=CARTESIAN_POINT('Ctrl Pts',(28.36814460273,0.9114061014946,0.5918740428154));
#18955=CARTESIAN_POINT('Ctrl Pts',(28.31939460273,1.080773975171,-0.1135939221767));
#18956=CARTESIAN_POINT('Ctrl Pts',(28.27064460273,0.7684321582634,-0.7684321583925));
#18957=CARTESIAN_POINT('Ctrl Pts',(28.22189460273,0.1135939230171,-1.080773975495));
#18958=CARTESIAN_POINT('Ctrl Pts',(28.17314460273,-0.5918740460484,-0.9114061000685));
#18959=CARTESIAN_POINT('Ctrl Pts',(28.12439460273,-1.033538954174,-0.3358171723489));
#18960=CARTESIAN_POINT('Ctrl Pts',(28.07564460273,-1.014547269612,0.3894482114172));
#18961=CARTESIAN_POINT('Ctrl Pts',(28.02689460273,-0.5433634217136,0.9411332701358));
#18962=CARTESIAN_POINT('Ctrl Pts',(27.97814460273,0.170000956467,1.073348045283));
#18963=CARTESIAN_POINT('Ctrl Pts',(27.92939460273,0.8075980268285,0.7271613725661));
#18964=CARTESIAN_POINT('Ctrl Pts',(27.88064460273,1.0852291028,0.05687880443492));
#18965=CARTESIAN_POINT('Ctrl Pts',(27.83189460273,0.8792134337481,-0.6387767584236));
#18966=CARTESIAN_POINT('Ctrl Pts',(27.78314460273,0.281143740254,-1.049643553578));
#18967=CARTESIAN_POINT('Ctrl Pts',(27.75064460273,-0.2006565122658,-1.011866061022));
#18968=CARTESIAN_POINT('Ctrl Pts',(27.73439460273,-0.4091770629343,-0.9190267303884));
#18969=CARTESIAN_POINT('Origin',(-1.12,0.,0.));
#18970=CARTESIAN_POINT('',(-1.12,3.5,0.));
#18971=CARTESIAN_POINT('Origin',(-1.12,0.,0.));
#18972=CARTESIAN_POINT('Origin',(-1.12,0.,0.));
#18973=CARTESIAN_POINT('',(-2.12,0.,3.5));
#18974=CARTESIAN_POINT('',(-2.12,3.5,-4.28626379701574E-16));
#18975=CARTESIAN_POINT('Origin',(-2.12,0.,0.));
#18976=CARTESIAN_POINT('Origin',(-2.12,0.,0.));
#18977=CARTESIAN_POINT('',(-1.12,3.5,-4.28626379701574E-16));
#18978=CARTESIAN_POINT('Origin',(9.88,0.,0.));
#18979=CARTESIAN_POINT('',(-2.62,9.37349864163661E-32,7.65404249467096E-16));
#18980=CARTESIAN_POINT('Origin',(9.88,0.,0.));
#18981=CARTESIAN_POINT('',(0.,0.,0.));
#18982=CARTESIAN_POINT('Origin',(0.,0.,0.));
#18983=CARTESIAN_POINT('',(0.,-2.230075362775,-3.641968441152));
#18984=CARTESIAN_POINT('',(0.,-2.511327206573,-3.454041967251));
#18985=CARTESIAN_POINT('Origin',(0.,0.,0.));
#18986=CARTESIAN_POINT('',(0.,-3.171966420818,-3.865052266814));
#18987=CARTESIAN_POINT('Origin',(0.,-6.004488071588,1.424259701479));
#18988=CARTESIAN_POINT('',(0.,-3.877279201205,-4.074519142905));
#18989=CARTESIAN_POINT('Origin',(0.,-4.033525089594,-2.256219876458));
#18990=CARTESIAN_POINT('',(0.,-4.074519142905,-3.877279201205));
#18991=CARTESIAN_POINT('Origin',(0.,0.,0.));
#18992=CARTESIAN_POINT('',(0.,-3.865052266814,-3.171966420818));
#18993=CARTESIAN_POINT('Origin',(0.,-2.256219876458,-4.033525089594));
#18994=CARTESIAN_POINT('',(0.,-3.454041967251,-2.511327206573));
#18995=CARTESIAN_POINT('Origin',(0.,1.424259701479,-6.004488071588));
#18996=CARTESIAN_POINT('',(0.,-3.641968441152,-2.230075362775));
#18997=CARTESIAN_POINT('Origin',(0.,0.,0.));
#18998=CARTESIAN_POINT('',(0.,-4.409606321742,-2.35698368413));
#18999=CARTESIAN_POINT('Origin',(0.,-5.002383041407,3.613662492007));
#19000=CARTESIAN_POINT('',(0.,-5.14138986667,-2.280594328));
#19001=CARTESIAN_POINT('Origin',(0.,-4.58990924064,-0.5409121388882));
#19002=CARTESIAN_POINT('',(0.,-5.24813535391,-2.022887924981));
#19003=CARTESIAN_POINT('Origin',(0.,0.,0.));
#19004=CARTESIAN_POINT('',(0.,-4.784701678661,-1.451423386272));
#19005=CARTESIAN_POINT('Origin',(0.,-3.628038590521,-2.863073307653));
#19006=CARTESIAN_POINT('',(0.,-4.152161993181,-0.9983591700307));
#19007=CARTESIAN_POINT('Origin',(0.,-0.9819737176534,-6.092464223689));
#19008=CARTESIAN_POINT('',(0.,-4.218152995092,-0.6666));
#19009=CARTESIAN_POINT('Origin',(0.,0.,0.));
#19010=CARTESIAN_POINT('',(0.,-4.975923633361,-0.4900857016478));
#19011=CARTESIAN_POINT('Origin',(0.,-3.238710539887,5.25291792606));
#19012=CARTESIAN_POINT('',(0.,-5.622770531748,-0.1394697002966));
#19013=CARTESIAN_POINT('Origin',(0.,-4.447521317429,1.256744568447));
#19014=CARTESIAN_POINT('',(0.,-5.622770531748,0.1394697002966));
#19015=CARTESIAN_POINT('Origin',(0.,0.,0.));
#19016=CARTESIAN_POINT('',(0.,-4.975923633361,0.4900857016478));
#19017=CARTESIAN_POINT('Origin',(0.,-4.447521317429,-1.256744568447));
#19018=CARTESIAN_POINT('',(0.,-4.218152995092,0.6666));
#19019=CARTESIAN_POINT('Origin',(0.,-3.238710539887,-5.25291792606));
#19020=CARTESIAN_POINT('',(0.,-4.152161993181,0.9983591700307));
#19021=CARTESIAN_POINT('Origin',(0.,0.,0.));
#19022=CARTESIAN_POINT('',(0.,-4.784701678661,1.451423386272));
#19023=CARTESIAN_POINT('Origin',(0.,-0.9819737176534,6.092464223689));
#19024=CARTESIAN_POINT('',(0.,-5.24813535391,2.022887924981));
#19025=CARTESIAN_POINT('Origin',(0.,-3.628038590521,2.863073307653));
#19026=CARTESIAN_POINT('',(0.,-5.14138986667,2.280594328));
#19027=CARTESIAN_POINT('Origin',(0.,0.,0.));
#19028=CARTESIAN_POINT('',(0.,-4.409606321742,2.35698368413));
#19029=CARTESIAN_POINT('Origin',(0.,-4.58990924064,0.5409121388882));
#19030=CARTESIAN_POINT('',(0.,-3.641968441152,2.230075362775));
#19031=CARTESIAN_POINT('Origin',(0.,-5.002383041407,-3.613662492007));
#19032=CARTESIAN_POINT('',(0.,-3.454041967251,2.511327206573));
#19033=CARTESIAN_POINT('Origin',(0.,0.,0.));
#19034=CARTESIAN_POINT('',(0.,-3.865052266814,3.171966420818));
#19035=CARTESIAN_POINT('Origin',(0.,1.424259701479,6.004488071588));
#19036=CARTESIAN_POINT('',(0.,-4.074519142905,3.877279201205));
#19037=CARTESIAN_POINT('Origin',(0.,-2.256219876458,4.033525089594));
#19038=CARTESIAN_POINT('',(0.,-3.877279201205,4.074519142905));
#19039=CARTESIAN_POINT('Origin',(0.,0.,0.));
#19040=CARTESIAN_POINT('',(0.,-3.171966420818,3.865052266814));
#19041=CARTESIAN_POINT('Origin',(0.,-4.033525089594,2.256219876458));
#19042=CARTESIAN_POINT('',(0.,-2.511327206573,3.454041967251));
#19043=CARTESIAN_POINT('Origin',(0.,-6.004488071588,-1.424259701479));
#19044=CARTESIAN_POINT('',(0.,-2.230075362775,3.641968441152));
#19045=CARTESIAN_POINT('Origin',(0.,0.,0.));
#19046=CARTESIAN_POINT('',(0.,-2.35698368413,4.409606321742));
#19047=CARTESIAN_POINT('Origin',(0.,3.613662492007,5.002383041407));
#19048=CARTESIAN_POINT('',(0.,-2.280594328,5.14138986667));
#19049=CARTESIAN_POINT('Origin',(0.,-0.5409121388882,4.58990924064));
#19050=CARTESIAN_POINT('',(0.,-2.022887924981,5.24813535391));
#19051=CARTESIAN_POINT('Origin',(0.,0.,0.));
#19052=CARTESIAN_POINT('',(0.,-1.451423386272,4.784701678661));
#19053=CARTESIAN_POINT('Origin',(0.,-2.863073307653,3.628038590521));
#19054=CARTESIAN_POINT('',(0.,-0.9983591700307,4.152161993181));
#19055=CARTESIAN_POINT('Origin',(0.,-6.092464223689,0.9819737176534));
#19056=CARTESIAN_POINT('',(0.,-0.6666,4.218152995092));
#19057=CARTESIAN_POINT('Origin',(0.,0.,0.));
#19058=CARTESIAN_POINT('',(0.,-0.4900857016478,4.975923633361));
#19059=CARTESIAN_POINT('Origin',(0.,5.25291792606,3.238710539887));
#19060=CARTESIAN_POINT('',(0.,-0.1394697002966,5.622770531748));
#19061=CARTESIAN_POINT('Origin',(0.,1.256744568447,4.447521317429));
#19062=CARTESIAN_POINT('',(0.,0.1394697002966,5.622770531748));
#19063=CARTESIAN_POINT('Origin',(0.,0.,0.));
#19064=CARTESIAN_POINT('',(0.,0.4900857016478,4.975923633361));
#19065=CARTESIAN_POINT('Origin',(0.,-1.256744568447,4.447521317429));
#19066=CARTESIAN_POINT('',(0.,0.6666,4.218152995092));
#19067=CARTESIAN_POINT('Origin',(0.,-5.25291792606,3.238710539887));
#19068=CARTESIAN_POINT('',(0.,0.9983591700307,4.152161993181));
#19069=CARTESIAN_POINT('Origin',(0.,0.,0.));
#19070=CARTESIAN_POINT('',(0.,1.451423386272,4.784701678661));
#19071=CARTESIAN_POINT('Origin',(0.,6.092464223689,0.9819737176533));
#19072=CARTESIAN_POINT('',(0.,2.022887924981,5.24813535391));
#19073=CARTESIAN_POINT('Origin',(0.,2.863073307653,3.628038590521));
#19074=CARTESIAN_POINT('',(0.,2.280594328,5.14138986667));
#19075=CARTESIAN_POINT('Origin',(0.,0.,0.));
#19076=CARTESIAN_POINT('',(0.,2.35698368413,4.409606321742));
#19077=CARTESIAN_POINT('Origin',(0.,0.5409121388882,4.58990924064));
#19078=CARTESIAN_POINT('',(0.,2.230075362775,3.641968441152));
#19079=CARTESIAN_POINT('Origin',(0.,-3.613662492007,5.002383041407));
#19080=CARTESIAN_POINT('',(0.,2.511327206573,3.454041967251));
#19081=CARTESIAN_POINT('Origin',(0.,0.,0.));
#19082=CARTESIAN_POINT('',(0.,3.171966420818,3.865052266814));
#19083=CARTESIAN_POINT('Origin',(0.,6.004488071588,-1.424259701479));
#19084=CARTESIAN_POINT('',(0.,3.877279201205,4.074519142905));
#19085=CARTESIAN_POINT('Origin',(0.,4.033525089594,2.256219876458));
#19086=CARTESIAN_POINT('',(0.,4.074519142905,3.877279201205));
#19087=CARTESIAN_POINT('Origin',(0.,0.,0.));
#19088=CARTESIAN_POINT('',(0.,3.865052266814,3.171966420818));
#19089=CARTESIAN_POINT('Origin',(0.,2.256219876458,4.033525089594));
#19090=CARTESIAN_POINT('',(0.,3.454041967251,2.511327206573));
#19091=CARTESIAN_POINT('Origin',(0.,-1.424259701479,6.004488071588));
#19092=CARTESIAN_POINT('',(0.,3.641968441152,2.230075362775));
#19093=CARTESIAN_POINT('Origin',(0.,0.,0.));
#19094=CARTESIAN_POINT('',(0.,4.409606321742,2.35698368413));
#19095=CARTESIAN_POINT('Origin',(0.,5.002383041407,-3.613662492007));
#19096=CARTESIAN_POINT('',(0.,5.14138986667,2.280594328));
#19097=CARTESIAN_POINT('Origin',(0.,4.58990924064,0.5409121388882));
#19098=CARTESIAN_POINT('',(0.,5.24813535391,2.022887924981));
#19099=CARTESIAN_POINT('Origin',(0.,0.,0.));
#19100=CARTESIAN_POINT('',(0.,4.784701678661,1.451423386272));
#19101=CARTESIAN_POINT('Origin',(0.,3.628038590521,2.863073307653));
#19102=CARTESIAN_POINT('',(0.,4.152161993181,0.9983591700307));
#19103=CARTESIAN_POINT('Origin',(0.,0.9819737176534,6.092464223689));
#19104=CARTESIAN_POINT('',(0.,4.218152995092,0.6666));
#19105=CARTESIAN_POINT('Origin',(0.,0.,0.));
#19106=CARTESIAN_POINT('',(0.,4.975923633361,0.4900857016478));
#19107=CARTESIAN_POINT('Origin',(0.,3.238710539887,-5.25291792606));
#19108=CARTESIAN_POINT('',(0.,5.622770531748,0.1394697002966));
#19109=CARTESIAN_POINT('Origin',(0.,4.447521317429,-1.256744568447));
#19110=CARTESIAN_POINT('',(0.,5.622770531748,-0.1394697002966));
#19111=CARTESIAN_POINT('Origin',(0.,0.,0.));
#19112=CARTESIAN_POINT('',(0.,4.975923633361,-0.4900857016478));
#19113=CARTESIAN_POINT('Origin',(0.,4.447521317429,1.256744568447));
#19114=CARTESIAN_POINT('',(0.,4.218152995092,-0.6666));
#19115=CARTESIAN_POINT('Origin',(0.,3.238710539887,5.25291792606));
#19116=CARTESIAN_POINT('',(0.,4.152161993181,-0.9983591700307));
#19117=CARTESIAN_POINT('Origin',(0.,0.,0.));
#19118=CARTESIAN_POINT('',(0.,4.784701678661,-1.451423386272));
#19119=CARTESIAN_POINT('Origin',(0.,0.9819737176534,-6.092464223689));
#19120=CARTESIAN_POINT('',(0.,5.24813535391,-2.022887924981));
#19121=CARTESIAN_POINT('Origin',(0.,3.628038590521,-2.863073307653));
#19122=CARTESIAN_POINT('',(0.,5.14138986667,-2.280594328));
#19123=CARTESIAN_POINT('Origin',(0.,0.,0.));
#19124=CARTESIAN_POINT('',(0.,4.409606321742,-2.35698368413));
#19125=CARTESIAN_POINT('Origin',(0.,4.58990924064,-0.5409121388882));
#19126=CARTESIAN_POINT('',(0.,3.641968441152,-2.230075362775));
#19127=CARTESIAN_POINT('Origin',(0.,5.002383041407,3.613662492007));
#19128=CARTESIAN_POINT('',(0.,3.454041967251,-2.511327206573));
#19129=CARTESIAN_POINT('Origin',(0.,0.,0.));
#19130=CARTESIAN_POINT('',(0.,3.865052266814,-3.171966420818));
#19131=CARTESIAN_POINT('Origin',(0.,-1.424259701479,-6.004488071588));
#19132=CARTESIAN_POINT('',(0.,4.074519142905,-3.877279201205));
#19133=CARTESIAN_POINT('Origin',(0.,2.256219876458,-4.033525089594));
#19134=CARTESIAN_POINT('',(0.,3.877279201205,-4.074519142905));
#19135=CARTESIAN_POINT('Origin',(0.,0.,0.));
#19136=CARTESIAN_POINT('',(0.,3.171966420818,-3.865052266814));
#19137=CARTESIAN_POINT('Origin',(0.,4.033525089594,-2.256219876458));
#19138=CARTESIAN_POINT('',(0.,2.511327206573,-3.454041967251));
#19139=CARTESIAN_POINT('Origin',(0.,6.004488071588,1.424259701479));
#19140=CARTESIAN_POINT('',(0.,2.230075362775,-3.641968441152));
#19141=CARTESIAN_POINT('Origin',(0.,0.,0.));
#19142=CARTESIAN_POINT('',(0.,2.35698368413,-4.409606321742));
#19143=CARTESIAN_POINT('Origin',(0.,-3.613662492007,-5.002383041407));
#19144=CARTESIAN_POINT('',(0.,2.280594328,-5.14138986667));
#19145=CARTESIAN_POINT('Origin',(0.,0.5409121388882,-4.58990924064));
#19146=CARTESIAN_POINT('',(0.,2.022887924981,-5.24813535391));
#19147=CARTESIAN_POINT('Origin',(0.,0.,0.));
#19148=CARTESIAN_POINT('',(0.,1.451423386272,-4.784701678661));
#19149=CARTESIAN_POINT('Origin',(0.,2.863073307653,-3.628038590521));
#19150=CARTESIAN_POINT('',(0.,0.9983591700307,-4.152161993181));
#19151=CARTESIAN_POINT('Origin',(0.,6.092464223689,-0.9819737176534));
#19152=CARTESIAN_POINT('',(0.,0.6666,-4.218152995092));
#19153=CARTESIAN_POINT('Origin',(0.,0.,0.));
#19154=CARTESIAN_POINT('',(0.,0.4900857016478,-4.975923633361));
#19155=CARTESIAN_POINT('Origin',(0.,-5.25291792606,-3.238710539887));
#19156=CARTESIAN_POINT('',(0.,0.1394697002966,-5.622770531748));
#19157=CARTESIAN_POINT('Origin',(0.,-1.256744568447,-4.447521317429));
#19158=CARTESIAN_POINT('',(0.,-0.1394697002966,-5.622770531748));
#19159=CARTESIAN_POINT('Origin',(0.,0.,0.));
#19160=CARTESIAN_POINT('',(0.,-0.4900857016478,-4.975923633361));
#19161=CARTESIAN_POINT('Origin',(0.,1.256744568447,-4.447521317429));
#19162=CARTESIAN_POINT('',(0.,-0.6666,-4.218152995092));
#19163=CARTESIAN_POINT('Origin',(0.,5.25291792606,-3.238710539887));
#19164=CARTESIAN_POINT('',(0.,-0.9983591700307,-4.152161993181));
#19165=CARTESIAN_POINT('Origin',(0.,0.,0.));
#19166=CARTESIAN_POINT('',(0.,-1.451423386272,-4.784701678661));
#19167=CARTESIAN_POINT('Origin',(0.,-6.092464223689,-0.9819737176534));
#19168=CARTESIAN_POINT('',(0.,-2.022887924981,-5.24813535391));
#19169=CARTESIAN_POINT('Origin',(0.,-2.863073307653,-3.628038590521));
#19170=CARTESIAN_POINT('',(0.,-2.280594328,-5.14138986667));
#19171=CARTESIAN_POINT('Origin',(0.,0.,0.));
#19172=CARTESIAN_POINT('',(0.,-2.35698368413,-4.409606321742));
#19173=CARTESIAN_POINT('Origin',(0.,-0.5409121388882,-4.58990924064));
#19174=CARTESIAN_POINT('Origin',(0.,3.613662492007,-5.002383041407));
#19175=CARTESIAN_POINT('',(0.,-2.540341184434,0.));
#19176=CARTESIAN_POINT('',(0.,-1.270170592217,2.2));
#19177=CARTESIAN_POINT('',(0.,-2.540341184434,0.));
#19178=CARTESIAN_POINT('',(0.,-1.270170592217,-2.2));
#19179=CARTESIAN_POINT('',(0.,-1.270170592217,-2.2));
#19180=CARTESIAN_POINT('',(0.,1.270170592217,-2.2));
#19181=CARTESIAN_POINT('',(0.,1.270170592217,-2.2));
#19182=CARTESIAN_POINT('',(0.,2.540341184434,0.));
#19183=CARTESIAN_POINT('',(0.,2.540341184434,0.));
#19184=CARTESIAN_POINT('',(0.,1.270170592217,2.2));
#19185=CARTESIAN_POINT('',(0.,1.270170592217,2.2));
#19186=CARTESIAN_POINT('',(0.,-1.270170592217,2.2));
#19187=CARTESIAN_POINT('Origin',(0.,-2.540341184434,0.));
#19188=CARTESIAN_POINT('',(4.4,-1.270170592217,2.2));
#19189=CARTESIAN_POINT('',(0.,-1.270170592217,2.2));
#19190=CARTESIAN_POINT('',(4.4,-2.540341184434,0.));
#19191=CARTESIAN_POINT('',(4.4,-2.540341184434,0.));
#19192=CARTESIAN_POINT('',(0.,-2.540341184434,0.));
#19193=CARTESIAN_POINT('Origin',(0.,-1.270170592217,-2.2));
#19194=CARTESIAN_POINT('',(4.4,-1.270170592217,-2.2));
#19195=CARTESIAN_POINT('',(4.4,-1.270170592217,-2.2));
#19196=CARTESIAN_POINT('',(0.,-1.270170592217,-2.2));
#19197=CARTESIAN_POINT('Origin',(0.,1.270170592217,-2.2));
#19198=CARTESIAN_POINT('',(4.4,1.270170592217,-2.2));
#19199=CARTESIAN_POINT('',(4.4,1.270170592217,-2.2));
#19200=CARTESIAN_POINT('',(0.,1.270170592217,-2.2));
#19201=CARTESIAN_POINT('Origin',(0.,2.540341184434,0.));
#19202=CARTESIAN_POINT('',(4.4,2.540341184434,0.));
#19203=CARTESIAN_POINT('',(4.4,2.540341184434,0.));
#19204=CARTESIAN_POINT('',(0.,2.540341184434,0.));
#19205=CARTESIAN_POINT('Origin',(0.,1.270170592217,2.2));
#19206=CARTESIAN_POINT('',(4.4,1.270170592217,2.2));
#19207=CARTESIAN_POINT('',(4.4,1.270170592217,2.2));
#19208=CARTESIAN_POINT('',(0.,1.270170592217,2.2));
#19209=CARTESIAN_POINT('Origin',(0.,-1.270170592217,2.2));
#19210=CARTESIAN_POINT('',(4.4,-1.270170592217,2.2));
#19211=CARTESIAN_POINT('Origin',(4.4,0.,0.));
#19212=CARTESIAN_POINT('',(4.4,3.5,4.28626379701574E-16));
#19213=CARTESIAN_POINT('Origin',(4.4,0.,0.));
#19214=CARTESIAN_POINT('Origin',(4.4,0.,0.));
#19215=CARTESIAN_POINT('',(5.8,3.5,4.28626379701574E-16));
#19216=CARTESIAN_POINT('',(4.4,3.5,4.28626379701574E-16));
#19217=CARTESIAN_POINT('Origin',(5.8,0.,0.));
#19218=CARTESIAN_POINT('Origin',(5.8,0.,0.));
#19219=CARTESIAN_POINT('',(5.8,-0.9983591700307,-4.152161993181));
#19220=CARTESIAN_POINT('',(5.8,-0.6666,-4.218152995092));
#19221=CARTESIAN_POINT('Origin',(5.8,0.,0.));
#19222=CARTESIAN_POINT('',(5.8,-0.4900857016478,-4.975923633361));
#19223=CARTESIAN_POINT('Origin',(5.8,5.25291792606,-3.238710539887));
#19224=CARTESIAN_POINT('',(5.8,-0.1394697002966,-5.622770531748));
#19225=CARTESIAN_POINT('Origin',(5.8,1.256744568447,-4.447521317429));
#19226=CARTESIAN_POINT('',(5.8,0.1394697002966,-5.622770531748));
#19227=CARTESIAN_POINT('Origin',(5.8,0.,0.));
#19228=CARTESIAN_POINT('',(5.8,0.4900857016478,-4.975923633361));
#19229=CARTESIAN_POINT('Origin',(5.8,-1.256744568447,-4.447521317429));
#19230=CARTESIAN_POINT('',(5.8,0.6666,-4.218152995092));
#19231=CARTESIAN_POINT('Origin',(5.8,-5.25291792606,-3.238710539887));
#19232=CARTESIAN_POINT('',(5.8,0.9983591700307,-4.152161993181));
#19233=CARTESIAN_POINT('Origin',(5.8,0.,0.));
#19234=CARTESIAN_POINT('',(5.8,1.451423386272,-4.784701678661));
#19235=CARTESIAN_POINT('Origin',(5.8,6.092464223689,-0.9819737176534));
#19236=CARTESIAN_POINT('',(5.8,2.022887924981,-5.24813535391));
#19237=CARTESIAN_POINT('Origin',(5.8,2.863073307653,-3.628038590521));
#19238=CARTESIAN_POINT('',(5.8,2.280594328,-5.14138986667));
#19239=CARTESIAN_POINT('Origin',(5.8,0.,0.));
#19240=CARTESIAN_POINT('',(5.8,2.35698368413,-4.409606321742));
#19241=CARTESIAN_POINT('Origin',(5.8,0.5409121388882,-4.58990924064));
#19242=CARTESIAN_POINT('',(5.8,2.230075362775,-3.641968441152));
#19243=CARTESIAN_POINT('Origin',(5.8,-3.613662492007,-5.002383041407));
#19244=CARTESIAN_POINT('',(5.8,2.511327206573,-3.454041967251));
#19245=CARTESIAN_POINT('Origin',(5.8,0.,0.));
#19246=CARTESIAN_POINT('',(5.8,3.171966420818,-3.865052266814));
#19247=CARTESIAN_POINT('Origin',(5.8,6.004488071588,1.424259701479));
#19248=CARTESIAN_POINT('',(5.8,3.877279201205,-4.074519142905));
#19249=CARTESIAN_POINT('Origin',(5.8,4.033525089594,-2.256219876458));
#19250=CARTESIAN_POINT('',(5.8,4.074519142905,-3.877279201205));
#19251=CARTESIAN_POINT('Origin',(5.8,0.,0.));
#19252=CARTESIAN_POINT('',(5.8,3.865052266814,-3.171966420818));
#19253=CARTESIAN_POINT('Origin',(5.8,2.256219876458,-4.033525089594));
#19254=CARTESIAN_POINT('',(5.8,3.454041967251,-2.511327206573));
#19255=CARTESIAN_POINT('Origin',(5.8,-1.424259701479,-6.004488071588));
#19256=CARTESIAN_POINT('',(5.8,3.641968441152,-2.230075362775));
#19257=CARTESIAN_POINT('Origin',(5.8,0.,0.));
#19258=CARTESIAN_POINT('',(5.8,4.409606321742,-2.35698368413));
#19259=CARTESIAN_POINT('Origin',(5.8,5.002383041407,3.613662492007));
#19260=CARTESIAN_POINT('',(5.8,5.14138986667,-2.280594328));
#19261=CARTESIAN_POINT('Origin',(5.8,4.58990924064,-0.5409121388882));
#19262=CARTESIAN_POINT('',(5.8,5.24813535391,-2.022887924981));
#19263=CARTESIAN_POINT('Origin',(5.8,0.,0.));
#19264=CARTESIAN_POINT('',(5.8,4.784701678661,-1.451423386272));
#19265=CARTESIAN_POINT('Origin',(5.8,3.628038590521,-2.863073307653));
#19266=CARTESIAN_POINT('',(5.8,4.152161993181,-0.9983591700307));
#19267=CARTESIAN_POINT('Origin',(5.8,0.9819737176534,-6.092464223689));
#19268=CARTESIAN_POINT('',(5.8,4.218152995092,-0.6666));
#19269=CARTESIAN_POINT('Origin',(5.8,0.,0.));
#19270=CARTESIAN_POINT('',(5.8,4.975923633361,-0.4900857016478));
#19271=CARTESIAN_POINT('Origin',(5.8,3.238710539887,5.25291792606));
#19272=CARTESIAN_POINT('',(5.8,5.622770531748,-0.1394697002966));
#19273=CARTESIAN_POINT('Origin',(5.8,4.447521317429,1.256744568447));
#19274=CARTESIAN_POINT('',(5.8,5.622770531748,0.1394697002966));
#19275=CARTESIAN_POINT('Origin',(5.8,0.,0.));
#19276=CARTESIAN_POINT('',(5.8,4.975923633361,0.4900857016478));
#19277=CARTESIAN_POINT('Origin',(5.8,4.447521317429,-1.256744568447));
#19278=CARTESIAN_POINT('',(5.8,4.218152995092,0.6666));
#19279=CARTESIAN_POINT('Origin',(5.8,3.238710539887,-5.25291792606));
#19280=CARTESIAN_POINT('',(5.8,4.152161993181,0.9983591700307));
#19281=CARTESIAN_POINT('Origin',(5.8,0.,0.));
#19282=CARTESIAN_POINT('',(5.8,4.784701678661,1.451423386272));
#19283=CARTESIAN_POINT('Origin',(5.8,0.9819737176534,6.092464223689));
#19284=CARTESIAN_POINT('',(5.8,5.24813535391,2.022887924981));
#19285=CARTESIAN_POINT('Origin',(5.8,3.628038590521,2.863073307653));
#19286=CARTESIAN_POINT('',(5.8,5.14138986667,2.280594328));
#19287=CARTESIAN_POINT('Origin',(5.8,0.,0.));
#19288=CARTESIAN_POINT('',(5.8,4.409606321742,2.35698368413));
#19289=CARTESIAN_POINT('Origin',(5.8,4.58990924064,0.5409121388882));
#19290=CARTESIAN_POINT('',(5.8,3.641968441152,2.230075362775));
#19291=CARTESIAN_POINT('Origin',(5.8,5.002383041407,-3.613662492007));
#19292=CARTESIAN_POINT('',(5.8,3.454041967251,2.511327206573));
#19293=CARTESIAN_POINT('Origin',(5.8,0.,0.));
#19294=CARTESIAN_POINT('',(5.8,3.865052266814,3.171966420818));
#19295=CARTESIAN_POINT('Origin',(5.8,-1.424259701479,6.004488071588));
#19296=CARTESIAN_POINT('',(5.8,4.074519142905,3.877279201205));
#19297=CARTESIAN_POINT('Origin',(5.8,2.256219876458,4.033525089594));
#19298=CARTESIAN_POINT('',(5.8,3.877279201205,4.074519142905));
#19299=CARTESIAN_POINT('Origin',(5.8,0.,0.));
#19300=CARTESIAN_POINT('',(5.8,3.171966420818,3.865052266814));
#19301=CARTESIAN_POINT('Origin',(5.8,4.033525089594,2.256219876458));
#19302=CARTESIAN_POINT('',(5.8,2.511327206573,3.454041967251));
#19303=CARTESIAN_POINT('Origin',(5.8,6.004488071588,-1.424259701479));
#19304=CARTESIAN_POINT('',(5.8,2.230075362775,3.641968441152));
#19305=CARTESIAN_POINT('Origin',(5.8,0.,0.));
#19306=CARTESIAN_POINT('',(5.8,2.35698368413,4.409606321742));
#19307=CARTESIAN_POINT('Origin',(5.8,-3.613662492007,5.002383041407));
#19308=CARTESIAN_POINT('',(5.8,2.280594328,5.14138986667));
#19309=CARTESIAN_POINT('Origin',(5.8,0.5409121388882,4.58990924064));
#19310=CARTESIAN_POINT('',(5.8,2.022887924981,5.24813535391));
#19311=CARTESIAN_POINT('Origin',(5.8,0.,0.));
#19312=CARTESIAN_POINT('',(5.8,1.451423386272,4.784701678661));
#19313=CARTESIAN_POINT('Origin',(5.8,2.863073307653,3.628038590521));
#19314=CARTESIAN_POINT('',(5.8,0.9983591700307,4.152161993181));
#19315=CARTESIAN_POINT('Origin',(5.8,6.092464223689,0.9819737176533));
#19316=CARTESIAN_POINT('',(5.8,0.6666,4.218152995092));
#19317=CARTESIAN_POINT('Origin',(5.8,0.,0.));
#19318=CARTESIAN_POINT('',(5.8,0.4900857016478,4.975923633361));
#19319=CARTESIAN_POINT('Origin',(5.8,-5.25291792606,3.238710539887));
#19320=CARTESIAN_POINT('',(5.8,0.1394697002966,5.622770531748));
#19321=CARTESIAN_POINT('Origin',(5.8,-1.256744568447,4.447521317429));
#19322=CARTESIAN_POINT('',(5.8,-0.1394697002966,5.622770531748));
#19323=CARTESIAN_POINT('Origin',(5.8,0.,0.));
#19324=CARTESIAN_POINT('',(5.8,-0.4900857016478,4.975923633361));
#19325=CARTESIAN_POINT('Origin',(5.8,1.256744568447,4.447521317429));
#19326=CARTESIAN_POINT('',(5.8,-0.6666,4.218152995092));
#19327=CARTESIAN_POINT('Origin',(5.8,5.25291792606,3.238710539887));
#19328=CARTESIAN_POINT('',(5.8,-0.9983591700307,4.152161993181));
#19329=CARTESIAN_POINT('Origin',(5.8,0.,0.));
#19330=CARTESIAN_POINT('',(5.8,-1.451423386272,4.784701678661));
#19331=CARTESIAN_POINT('Origin',(5.8,-6.092464223689,0.9819737176534));
#19332=CARTESIAN_POINT('',(5.8,-2.022887924981,5.24813535391));
#19333=CARTESIAN_POINT('Origin',(5.8,-2.863073307653,3.628038590521));
#19334=CARTESIAN_POINT('',(5.8,-2.280594328,5.14138986667));
#19335=CARTESIAN_POINT('Origin',(5.8,0.,0.));
#19336=CARTESIAN_POINT('',(5.8,-2.35698368413,4.409606321742));
#19337=CARTESIAN_POINT('Origin',(5.8,-0.5409121388882,4.58990924064));
#19338=CARTESIAN_POINT('',(5.8,-2.230075362775,3.641968441152));
#19339=CARTESIAN_POINT('Origin',(5.8,3.613662492007,5.002383041407));
#19340=CARTESIAN_POINT('',(5.8,-2.511327206573,3.454041967251));
#19341=CARTESIAN_POINT('Origin',(5.8,0.,0.));
#19342=CARTESIAN_POINT('',(5.8,-3.171966420818,3.865052266814));
#19343=CARTESIAN_POINT('Origin',(5.8,-6.004488071588,-1.424259701479));
#19344=CARTESIAN_POINT('',(5.8,-3.877279201205,4.074519142905));
#19345=CARTESIAN_POINT('Origin',(5.8,-4.033525089594,2.256219876458));
#19346=CARTESIAN_POINT('',(5.8,-4.074519142905,3.877279201205));
#19347=CARTESIAN_POINT('Origin',(5.8,0.,0.));
#19348=CARTESIAN_POINT('',(5.8,-3.865052266814,3.171966420818));
#19349=CARTESIAN_POINT('Origin',(5.8,-2.256219876458,4.033525089594));
#19350=CARTESIAN_POINT('',(5.8,-3.454041967251,2.511327206573));
#19351=CARTESIAN_POINT('Origin',(5.8,1.424259701479,6.004488071588));
#19352=CARTESIAN_POINT('',(5.8,-3.641968441152,2.230075362775));
#19353=CARTESIAN_POINT('Origin',(5.8,0.,0.));
#19354=CARTESIAN_POINT('',(5.8,-4.409606321742,2.35698368413));
#19355=CARTESIAN_POINT('Origin',(5.8,-5.002383041407,-3.613662492007));
#19356=CARTESIAN_POINT('',(5.8,-5.14138986667,2.280594328));
#19357=CARTESIAN_POINT('Origin',(5.8,-4.58990924064,0.5409121388882));
#19358=CARTESIAN_POINT('',(5.8,-5.24813535391,2.022887924981));
#19359=CARTESIAN_POINT('Origin',(5.8,0.,0.));
#19360=CARTESIAN_POINT('',(5.8,-4.784701678661,1.451423386272));
#19361=CARTESIAN_POINT('Origin',(5.8,-3.628038590521,2.863073307653));
#19362=CARTESIAN_POINT('',(5.8,-4.152161993181,0.9983591700307));
#19363=CARTESIAN_POINT('Origin',(5.8,-0.9819737176534,6.092464223689));
#19364=CARTESIAN_POINT('',(5.8,-4.218152995092,0.6666));
#19365=CARTESIAN_POINT('Origin',(5.8,0.,0.));
#19366=CARTESIAN_POINT('',(5.8,-4.975923633361,0.4900857016478));
#19367=CARTESIAN_POINT('Origin',(5.8,-3.238710539887,-5.25291792606));
#19368=CARTESIAN_POINT('',(5.8,-5.622770531748,0.1394697002966));
#19369=CARTESIAN_POINT('Origin',(5.8,-4.447521317429,-1.256744568447));
#19370=CARTESIAN_POINT('',(5.8,-5.622770531748,-0.1394697002966));
#19371=CARTESIAN_POINT('Origin',(5.8,0.,0.));
#19372=CARTESIAN_POINT('',(5.8,-4.975923633361,-0.4900857016478));
#19373=CARTESIAN_POINT('Origin',(5.8,-4.447521317429,1.256744568447));
#19374=CARTESIAN_POINT('',(5.8,-4.218152995092,-0.6666));
#19375=CARTESIAN_POINT('Origin',(5.8,-3.238710539887,5.25291792606));
#19376=CARTESIAN_POINT('',(5.8,-4.152161993181,-0.9983591700307));
#19377=CARTESIAN_POINT('Origin',(5.8,0.,0.));
#19378=CARTESIAN_POINT('',(5.8,-4.784701678661,-1.451423386272));
#19379=CARTESIAN_POINT('Origin',(5.8,-0.9819737176534,-6.092464223689));
#19380=CARTESIAN_POINT('',(5.8,-5.24813535391,-2.022887924981));
#19381=CARTESIAN_POINT('Origin',(5.8,-3.628038590521,-2.863073307653));
#19382=CARTESIAN_POINT('',(5.8,-5.14138986667,-2.280594328));
#19383=CARTESIAN_POINT('Origin',(5.8,0.,0.));
#19384=CARTESIAN_POINT('',(5.8,-4.409606321742,-2.35698368413));
#19385=CARTESIAN_POINT('Origin',(5.8,-4.58990924064,-0.5409121388882));
#19386=CARTESIAN_POINT('',(5.8,-3.641968441152,-2.230075362775));
#19387=CARTESIAN_POINT('Origin',(5.8,-5.002383041407,3.613662492007));
#19388=CARTESIAN_POINT('',(5.8,-3.454041967251,-2.511327206573));
#19389=CARTESIAN_POINT('Origin',(5.8,0.,0.));
#19390=CARTESIAN_POINT('',(5.8,-3.865052266814,-3.171966420818));
#19391=CARTESIAN_POINT('Origin',(5.8,1.424259701479,-6.004488071588));
#19392=CARTESIAN_POINT('',(5.8,-4.074519142905,-3.877279201205));
#19393=CARTESIAN_POINT('Origin',(5.8,-2.256219876458,-4.033525089594));
#19394=CARTESIAN_POINT('',(5.8,-3.877279201205,-4.074519142905));
#19395=CARTESIAN_POINT('Origin',(5.8,0.,0.));
#19396=CARTESIAN_POINT('',(5.8,-3.171966420818,-3.865052266814));
#19397=CARTESIAN_POINT('Origin',(5.8,-4.033525089594,-2.256219876458));
#19398=CARTESIAN_POINT('',(5.8,-2.511327206573,-3.454041967251));
#19399=CARTESIAN_POINT('Origin',(5.8,-6.004488071588,1.424259701479));
#19400=CARTESIAN_POINT('',(5.8,-2.230075362775,-3.641968441152));
#19401=CARTESIAN_POINT('Origin',(5.8,0.,0.));
#19402=CARTESIAN_POINT('',(5.8,-2.35698368413,-4.409606321742));
#19403=CARTESIAN_POINT('Origin',(5.8,3.613662492007,-5.002383041407));
#19404=CARTESIAN_POINT('',(5.8,-2.280594328,-5.14138986667));
#19405=CARTESIAN_POINT('Origin',(5.8,-0.5409121388882,-4.58990924064));
#19406=CARTESIAN_POINT('',(5.8,-2.022887924981,-5.24813535391));
#19407=CARTESIAN_POINT('Origin',(5.8,0.,0.));
#19408=CARTESIAN_POINT('',(5.8,-1.451423386272,-4.784701678661));
#19409=CARTESIAN_POINT('Origin',(5.8,-2.863073307653,-3.628038590521));
#19410=CARTESIAN_POINT('Origin',(5.8,-6.092464223689,-0.9819737176534));
#19411=CARTESIAN_POINT('Origin',(0.,0.,0.));
#19412=CARTESIAN_POINT('',(5.8,0.9983591700307,-4.152161993181));
#19413=CARTESIAN_POINT('',(5.8,0.6666,-4.218152995092));
#19414=CARTESIAN_POINT('Origin',(0.,0.,0.));
#19415=CARTESIAN_POINT('',(5.8,2.511327206573,-3.454041967251));
#19416=CARTESIAN_POINT('',(5.8,2.230075362775,-3.641968441152));
#19417=CARTESIAN_POINT('Origin',(0.,0.,0.));
#19418=CARTESIAN_POINT('',(5.8,3.641968441152,-2.230075362775));
#19419=CARTESIAN_POINT('',(5.8,3.454041967251,-2.511327206573));
#19420=CARTESIAN_POINT('Origin',(0.,0.,0.));
#19421=CARTESIAN_POINT('',(5.8,4.218152995092,-0.6666));
#19422=CARTESIAN_POINT('',(5.8,4.152161993181,-0.9983591700307));
#19423=CARTESIAN_POINT('Origin',(0.,0.,0.));
#19424=CARTESIAN_POINT('',(5.8,4.152161993181,0.9983591700307));
#19425=CARTESIAN_POINT('',(5.8,4.218152995092,0.6666));
#19426=CARTESIAN_POINT('Origin',(0.,0.,0.));
#19427=CARTESIAN_POINT('',(5.8,3.454041967251,2.511327206573));
#19428=CARTESIAN_POINT('',(5.8,3.641968441152,2.230075362775));
#19429=CARTESIAN_POINT('Origin',(0.,0.,0.));
#19430=CARTESIAN_POINT('',(5.8,2.230075362775,3.641968441152));
#19431=CARTESIAN_POINT('',(5.8,2.511327206573,3.454041967251));
#19432=CARTESIAN_POINT('Origin',(0.,0.,0.));
#19433=CARTESIAN_POINT('',(5.8,0.6666,4.218152995092));
#19434=CARTESIAN_POINT('',(5.8,0.9983591700307,4.152161993181));
#19435=CARTESIAN_POINT('Origin',(0.,0.,0.));
#19436=CARTESIAN_POINT('',(5.8,-0.9983591700307,4.152161993181));
#19437=CARTESIAN_POINT('',(5.8,-0.6666,4.218152995092));
#19438=CARTESIAN_POINT('Origin',(0.,0.,0.));
#19439=CARTESIAN_POINT('',(5.8,-2.511327206573,3.454041967251));
#19440=CARTESIAN_POINT('',(5.8,-2.230075362775,3.641968441152));
#19441=CARTESIAN_POINT('Origin',(0.,0.,0.));
#19442=CARTESIAN_POINT('',(5.8,-3.641968441152,2.230075362775));
#19443=CARTESIAN_POINT('',(5.8,-3.454041967251,2.511327206573));
#19444=CARTESIAN_POINT('Origin',(0.,0.,0.));
#19445=CARTESIAN_POINT('',(5.8,-4.218152995092,0.6666));
#19446=CARTESIAN_POINT('',(5.8,-4.152161993181,0.9983591700307));
#19447=CARTESIAN_POINT('Origin',(0.,0.,0.));
#19448=CARTESIAN_POINT('',(5.8,-4.152161993181,-0.9983591700307));
#19449=CARTESIAN_POINT('',(5.8,-4.218152995092,-0.6666));
#19450=CARTESIAN_POINT('Origin',(0.,0.,0.));
#19451=CARTESIAN_POINT('',(5.8,-3.454041967251,-2.511327206573));
#19452=CARTESIAN_POINT('',(5.8,-3.641968441152,-2.230075362775));
#19453=CARTESIAN_POINT('Origin',(0.,0.,0.));
#19454=CARTESIAN_POINT('',(5.8,-0.9983591700307,-4.152161993181));
#19455=CARTESIAN_POINT('',(5.8,-0.6666,-4.218152995092));
#19456=CARTESIAN_POINT('Origin',(0.,0.,0.));
#19457=CARTESIAN_POINT('',(5.8,-2.230075362775,-3.641968441152));
#19458=CARTESIAN_POINT('',(5.8,-2.511327206573,-3.454041967251));
#19459=CARTESIAN_POINT('Origin',(0.,6.092464223689,-0.9819737176534));
#19460=CARTESIAN_POINT('',(0.,1.451423386272,-4.784701678661));
#19461=CARTESIAN_POINT('Origin',(0.,2.863073307653,-3.628038590521));
#19462=CARTESIAN_POINT('',(1.486313498852,2.022887924981,-5.24813535391));
#19463=CARTESIAN_POINT('',(4.313686501148,2.022887924981,-5.24813535391));
#19464=CARTESIAN_POINT('Ctrl Pts',(1.48631349885215,2.02288792498104,-5.24813535391027));
#19465=CARTESIAN_POINT('Ctrl Pts',(1.66118098688097,1.87008428427961,-5.16889108391505));
#19466=CARTESIAN_POINT('Ctrl Pts',(1.88121857570601,1.75588316418942,-5.08191986723504));
#19467=CARTESIAN_POINT('Ctrl Pts',(2.37244120406315,1.60793578184472,-4.95658861428298));
#19468=CARTESIAN_POINT('Ctrl Pts',(2.64520960921169,1.57573256670641,-4.92163003170291));
#19469=CARTESIAN_POINT('Ctrl Pts',(3.15479039078831,1.57573256670641,-4.92163003170291));
#19470=CARTESIAN_POINT('Ctrl Pts',(3.42755879593685,1.60793578184472,-4.95658861428298));
#19471=CARTESIAN_POINT('Ctrl Pts',(3.91878142429399,1.75588316418942,-5.08191986723504));
#19472=CARTESIAN_POINT('Ctrl Pts',(4.13881901311903,1.87008428427961,-5.16889108391505));
#19473=CARTESIAN_POINT('Ctrl Pts',(4.31368650114785,2.02288792498104,-5.24813535391027));
#19474=CARTESIAN_POINT('',(4.313686501148,2.022887924981,-5.24813535391));
#19475=CARTESIAN_POINT('',(0.,2.022887924981,-5.24813535391));
#19476=CARTESIAN_POINT('Origin',(2.9,1.216381379543,-7.614099837768));
#19477=CARTESIAN_POINT('',(1.486313498852,2.280594328,-5.14138986667));
#19478=CARTESIAN_POINT('Origin',(4.18857238240928,1.37199249389726,-3.31228288622663));
#19479=CARTESIAN_POINT('',(4.313686501148,2.280594328,-5.14138986667));
#19480=CARTESIAN_POINT('Ctrl Pts',(4.31368650114836,2.2805943280003,-5.14138986666972));
#19481=CARTESIAN_POINT('Ctrl Pts',(4.2421366487679,2.30187682976273,-5.07425280417236));
#19482=CARTESIAN_POINT('Ctrl Pts',(4.16493748660748,2.31714303849307,-5.01237860886288));
#19483=CARTESIAN_POINT('Ctrl Pts',(3.92608589772523,2.35153180152409,-4.84636481388562));
#19484=CARTESIAN_POINT('Ctrl Pts',(3.73056477719277,2.35999656858893,-4.74968617002381));
#19485=CARTESIAN_POINT('Ctrl Pts',(3.31778929268131,2.36668478817641,-4.62382504158597));
#19486=CARTESIAN_POINT('Ctrl Pts',(3.10064734052491,2.36590678665386,-4.59432915316309));
#19487=CARTESIAN_POINT('Ctrl Pts',(2.69935265947509,2.36590678665386,-4.59432915316309));
#19488=CARTESIAN_POINT('Ctrl Pts',(2.48221070731869,2.36668478817641,-4.62382504158597));
#19489=CARTESIAN_POINT('Ctrl Pts',(2.06943522280723,2.35999656858893,-4.74968617002381));
#19490=CARTESIAN_POINT('Ctrl Pts',(1.87391410227477,2.35153180152409,-4.84636481388562));
#19491=CARTESIAN_POINT('Ctrl Pts',(1.63506251339252,2.31714303849307,-5.01237860886288));
#19492=CARTESIAN_POINT('Ctrl Pts',(1.5578633512321,2.30187682976273,-5.07425280417236));
#19493=CARTESIAN_POINT('Ctrl Pts',(1.48631349885164,2.2805943280003,-5.14138986666971));
#19494=CARTESIAN_POINT('Origin',(1.61142761759064,1.37199249389664,-3.31228288622489));
#19495=CARTESIAN_POINT('Origin',(0.,0.,0.));
#19496=CARTESIAN_POINT('',(0.,2.280594328,-5.14138986667));
#19497=CARTESIAN_POINT('Origin',(0.,0.,0.));
#19498=CARTESIAN_POINT('',(4.313686501148,2.280594328,-5.14138986667));
#19499=CARTESIAN_POINT('Origin',(0.,0.5409121388882,-4.58990924064));
#19500=CARTESIAN_POINT('',(0.,2.35698368413,-4.409606321742));
#19501=CARTESIAN_POINT('Origin',(0.,-3.613662492007,-5.002383041407));
#19502=CARTESIAN_POINT('Origin',(0.,-5.25291792606,-3.238710539887));
#19503=CARTESIAN_POINT('',(0.,0.4900857016478,-4.975923633361));
#19504=CARTESIAN_POINT('Origin',(0.,-1.256744568447,-4.447521317429));
#19505=CARTESIAN_POINT('',(4.313686501148,0.1394697002966,-5.622770531748));
#19506=CARTESIAN_POINT('',(1.486313498852,0.1394697002966,-5.622770531748));
#19507=CARTESIAN_POINT('Ctrl Pts',(4.31368650114762,0.139469700296212,-5.62277053174818));
#19508=CARTESIAN_POINT('Ctrl Pts',(4.13881901311883,0.250316387196373,-5.49108295092936));
#19509=CARTESIAN_POINT('Ctrl Pts',(3.91878142429387,0.322542020921459,-5.36702914730511));
#19510=CARTESIAN_POINT('Ctrl Pts',(3.42755879593682,0.411265385296034,-5.19462115583365));
#19511=CARTESIAN_POINT('Ctrl Pts',(3.1547903907883,0.427639206271016,-5.15));
#19512=CARTESIAN_POINT('Ctrl Pts',(2.9,0.427639206271016,-5.15));
#19513=CARTESIAN_POINT('Ctrl Pts',(2.6452096092117,0.427639206271016,-5.15));
#19514=CARTESIAN_POINT('Ctrl Pts',(2.37244120406318,0.411265385296034,-5.19462115583365));
#19515=CARTESIAN_POINT('Ctrl Pts',(1.88121857570613,0.322542020921459,-5.36702914730511));
#19516=CARTESIAN_POINT('Ctrl Pts',(1.66118098688117,0.250316387196373,-5.49108295092936));
#19517=CARTESIAN_POINT('Ctrl Pts',(1.48631349885238,0.139469700296212,-5.62277053174818));
#19518=CARTESIAN_POINT('',(0.,0.1394697002966,-5.622770531748));
#19519=CARTESIAN_POINT('',(4.313686501148,0.1394697002966,-5.622770531748));
#19520=CARTESIAN_POINT('Origin',(2.9,-1.79,-7.5));
#19521=CARTESIAN_POINT('',(1.486313498852,-0.1394697002966,-5.622770531748));
#19522=CARTESIAN_POINT('',(4.313686501148,-0.1394697002966,-5.622770531748));
#19523=CARTESIAN_POINT('Ctrl Pts',(1.48631349885238,-0.139469700296214,
-5.62277053174818));
#19524=CARTESIAN_POINT('Ctrl Pts',(1.55786335123272,-0.18482440959043,-5.56888843465785));
#19525=CARTESIAN_POINT('Ctrl Pts',(1.63506251339297,-0.222606776811207,
-5.51756625717708));
#19526=CARTESIAN_POINT('Ctrl Pts',(1.87391410227503,-0.317908580005743,
-5.37734951975473));
#19527=CARTESIAN_POINT('Ctrl Pts',(2.06943522280744,-0.362726320313873,
-5.29126942557444));
#19528=CARTESIAN_POINT('Ctrl Pts',(2.4822107073188,-0.417070398131636,-5.17754837590016));
#19529=CARTESIAN_POINT('Ctrl Pts',(2.69935265947514,-0.427639206271016,
-5.15));
#19530=CARTESIAN_POINT('Ctrl Pts',(3.10064734052485,-0.427639206271016,
-5.15));
#19531=CARTESIAN_POINT('Ctrl Pts',(3.3177892926812,-0.417070398131636,-5.17754837590016));
#19532=CARTESIAN_POINT('Ctrl Pts',(3.73056477719256,-0.362726320313873,
-5.29126942557444));
#19533=CARTESIAN_POINT('Ctrl Pts',(3.92608589772497,-0.317908580005744,
-5.37734951975473));
#19534=CARTESIAN_POINT('Ctrl Pts',(4.16493748660703,-0.222606776811208,
-5.51756625717708));
#19535=CARTESIAN_POINT('Ctrl Pts',(4.24213664876728,-0.18482440959043,-5.56888843465785));
#19536=CARTESIAN_POINT('Ctrl Pts',(4.31368650114762,-0.139469700296214,
-5.62277053174818));
#19537=CARTESIAN_POINT('Origin',(4.1885723820417,-8.86270223876551E-14,
-3.58518916149213));
#19538=CARTESIAN_POINT('Origin',(1.61142761795821,4.57273108267486E-14,
-3.58518916149182));
#19539=CARTESIAN_POINT('Origin',(0.,1.256744568447,-4.447521317429));
#19540=CARTESIAN_POINT('',(4.313686501148,-0.1394697002966,-5.622770531748));
#19541=CARTESIAN_POINT('',(0.,-0.4900857016478,-4.975923633361));
#19542=CARTESIAN_POINT('',(0.,-0.1394697002966,-5.622770531748));
#19543=CARTESIAN_POINT('Origin',(0.,0.,0.));
#19544=CARTESIAN_POINT('Origin',(0.,0.,0.));
#19545=CARTESIAN_POINT('Origin',(0.,5.25291792606,-3.238710539887));
#19546=CARTESIAN_POINT('Origin',(0.,6.004488071588,1.424259701479));
#19547=CARTESIAN_POINT('',(0.,3.171966420818,-3.865052266814));
#19548=CARTESIAN_POINT('Origin',(0.,4.033525089594,-2.256219876458));
#19549=CARTESIAN_POINT('',(1.486313498852,3.877279201205,-4.074519142905));
#19550=CARTESIAN_POINT('',(4.313686501148,3.877279201205,-4.074519142905));
#19551=CARTESIAN_POINT('Ctrl Pts',(1.48631349885213,3.87727920120514,-4.07451914290497));
#19552=CARTESIAN_POINT('Ctrl Pts',(1.66118098688094,3.7057815758309,-4.05978240548905));
#19553=CARTESIAN_POINT('Ctrl Pts',(1.88121857570595,3.56699105467367,-4.02313435509682));
#19554=CARTESIAN_POINT('Ctrl Pts',(2.37244120406308,3.38234330217447,-3.96396038779548));
#19555=CARTESIAN_POINT('Ctrl Pts',(2.64520960921165,3.33921334045477,-3.94398650576646));
#19556=CARTESIAN_POINT('Ctrl Pts',(3.15479039078834,3.33921334045477,-3.94398650576646));
#19557=CARTESIAN_POINT('Ctrl Pts',(3.42755879593693,3.38234330217447,-3.96396038779548));
#19558=CARTESIAN_POINT('Ctrl Pts',(3.91878142429406,3.56699105467367,-4.02313435509682));
#19559=CARTESIAN_POINT('Ctrl Pts',(4.13881901311906,3.7057815758309,-4.05978240548905));
#19560=CARTESIAN_POINT('Ctrl Pts',(4.31368650114787,3.87727920120514,-4.07451914290497));
#19561=CARTESIAN_POINT('',(4.313686501148,3.877279201205,-4.074519142905));
#19562=CARTESIAN_POINT('',(0.,3.877279201205,-4.074519142905));
#19563=CARTESIAN_POINT('Origin',(2.9,4.037579720575,-6.569021997223));
#19564=CARTESIAN_POINT('',(1.486313498852,4.074519142905,-3.877279201205));
#19565=CARTESIAN_POINT('Origin',(4.18857238224087,2.53511156782161,-2.53511156782161));
#19566=CARTESIAN_POINT('',(4.313686501148,4.074519142905,-3.877279201205));
#19567=CARTESIAN_POINT('Ctrl Pts',(4.31368650114787,4.07451914290497,-3.87727920120514));
#19568=CARTESIAN_POINT('Ctrl Pts',(4.24213664876753,4.06848936916851,-3.80710818246732));
#19569=CARTESIAN_POINT('Ctrl Pts',(4.16493748660728,4.05891527751768,-3.74410175467432));
#19570=CARTESIAN_POINT('Ctrl Pts',(3.9260858977252,4.0271556229486,-3.57756499750892));
#19571=CARTESIAN_POINT('Ctrl Pts',(3.73056477719275,3.99797873271785,-3.48500625109951));
#19572=CARTESIAN_POINT('Ctrl Pts',(3.3177892926813,3.95599287327173,-3.36616625976887));
#19573=CARTESIAN_POINT('Ctrl Pts',(3.1006473405249,3.94398650576646,-3.33921334045477));
#19574=CARTESIAN_POINT('Ctrl Pts',(2.6993526594751,3.94398650576646,-3.33921334045477));
#19575=CARTESIAN_POINT('Ctrl Pts',(2.4822107073187,3.95599287327173,-3.36616625976887));
#19576=CARTESIAN_POINT('Ctrl Pts',(2.06943522280725,3.99797873271785,-3.48500625109951));
#19577=CARTESIAN_POINT('Ctrl Pts',(1.8739141022748,4.0271556229486,-3.57756499750892));
#19578=CARTESIAN_POINT('Ctrl Pts',(1.63506251339272,4.05891527751768,-3.74410175467432));
#19579=CARTESIAN_POINT('Ctrl Pts',(1.55786335123247,4.06848936916851,-3.80710818246732));
#19580=CARTESIAN_POINT('Ctrl Pts',(1.48631349885214,4.07451914290497,-3.87727920120514));
#19581=CARTESIAN_POINT('Origin',(1.61142761775721,2.53511156782107,-2.535111567821));
#19582=CARTESIAN_POINT('Origin',(0.,0.,0.));
#19583=CARTESIAN_POINT('',(0.,4.074519142905,-3.877279201205));
#19584=CARTESIAN_POINT('Origin',(0.,0.,0.));
#19585=CARTESIAN_POINT('',(4.313686501148,4.074519142905,-3.877279201205));
#19586=CARTESIAN_POINT('Origin',(0.,2.256219876458,-4.033525089594));
#19587=CARTESIAN_POINT('',(0.,3.865052266814,-3.171966420818));
#19588=CARTESIAN_POINT('Origin',(0.,-1.424259701479,-6.004488071588));
#19589=CARTESIAN_POINT('Origin',(0.,5.002383041407,3.613662492007));
#19590=CARTESIAN_POINT('',(0.,4.409606321742,-2.35698368413));
#19591=CARTESIAN_POINT('Origin',(0.,4.58990924064,-0.5409121388882));
#19592=CARTESIAN_POINT('',(1.486313498852,5.14138986667,-2.280594328));
#19593=CARTESIAN_POINT('',(4.313686501148,5.14138986667,-2.280594328));
#19594=CARTESIAN_POINT('Ctrl Pts',(1.48631349885156,5.14138986666964,-2.28059432800033));
#19595=CARTESIAN_POINT('Ctrl Pts',(1.66118098688046,4.9773072154557,-2.33260865784654));
#19596=CARTESIAN_POINT('Ctrl Pts',(1.88121857570565,4.83505689193818,-2.35186310719892));
#19597=CARTESIAN_POINT('Ctrl Pts',(2.37244120406304,4.64181971576632,-2.3678551256566));
#19598=CARTESIAN_POINT('Ctrl Pts',(2.64520960921164,4.59432915316297,-2.36590678665386));
#19599=CARTESIAN_POINT('Ctrl Pts',(3.15479039078836,4.59432915316297,-2.36590678665386));
#19600=CARTESIAN_POINT('Ctrl Pts',(3.42755879593696,4.64181971576632,-2.3678551256566));
#19601=CARTESIAN_POINT('Ctrl Pts',(3.91878142429434,4.83505689193819,-2.35186310719892));
#19602=CARTESIAN_POINT('Ctrl Pts',(4.13881901311954,4.9773072154557,-2.33260865784654));
#19603=CARTESIAN_POINT('Ctrl Pts',(4.31368650114844,5.14138986666964,-2.28059432800033));
#19604=CARTESIAN_POINT('',(4.313686501148,5.14138986667,-2.280594328));
#19605=CARTESIAN_POINT('',(0.,5.14138986667,-2.280594328));
#19606=CARTESIAN_POINT('Origin',(2.9,6.244093149901,-4.523870105933));
#19607=CARTESIAN_POINT('',(1.486313498852,5.24813535391,-2.022887924981));
#19608=CARTESIAN_POINT('Origin',(4.18857238256757,3.31228288611555,-1.37199249385133));
#19609=CARTESIAN_POINT('',(4.313686501148,5.24813535391,-2.022887924981));
#19610=CARTESIAN_POINT('Ctrl Pts',(4.31368650114793,5.24813535391023,-2.02288792498097));
#19611=CARTESIAN_POINT('Ctrl Pts',(4.24213664876754,5.21571128306628,-1.96036585150342));
#19612=CARTESIAN_POINT('Ctrl Pts',(4.16493748660722,5.18275445969878,-1.90581934870347));
#19613=CARTESIAN_POINT('Ctrl Pts',(3.92608589772509,5.08968150703577,-1.76411334096875));
#19614=CARTESIAN_POINT('Ctrl Pts',(3.73056477719266,5.0273048765579,-1.68976572210544));
#19615=CARTESIAN_POINT('Ctrl Pts',(3.31778929268125,4.94303690457612,-1.59603917927489));
#19616=CARTESIAN_POINT('Ctrl Pts',(3.10064734052488,4.92163003170282,-1.57573256670632));
#19617=CARTESIAN_POINT('Ctrl Pts',(2.69935265947512,4.92163003170282,-1.57573256670632));
#19618=CARTESIAN_POINT('Ctrl Pts',(2.48221070731875,4.94303690457612,-1.59603917927489));
#19619=CARTESIAN_POINT('Ctrl Pts',(2.06943522280734,5.02730487655791,-1.68976572210544));
#19620=CARTESIAN_POINT('Ctrl Pts',(1.87391410227491,5.08968150703577,-1.76411334096875));
#19621=CARTESIAN_POINT('Ctrl Pts',(1.63506251339278,5.18275445969878,-1.90581934870347));
#19622=CARTESIAN_POINT('Ctrl Pts',(1.55786335123246,5.21571128306628,-1.96036585150342));
#19623=CARTESIAN_POINT('Ctrl Pts',(1.48631349885208,5.24813535391023,-2.02288792498097));
#19624=CARTESIAN_POINT('Origin',(1.61142761743281,3.31228288611595,-1.37199249385144));
#19625=CARTESIAN_POINT('Origin',(0.,0.,0.));
#19626=CARTESIAN_POINT('',(0.,5.24813535391,-2.022887924981));
#19627=CARTESIAN_POINT('Origin',(0.,0.,0.));
#19628=CARTESIAN_POINT('',(4.313686501148,5.24813535391,-2.022887924981));
#19629=CARTESIAN_POINT('Origin',(0.,3.628038590521,-2.863073307653));
#19630=CARTESIAN_POINT('',(0.,4.784701678661,-1.451423386272));
#19631=CARTESIAN_POINT('Origin',(0.,0.9819737176534,-6.092464223689));
#19632=CARTESIAN_POINT('Origin',(0.,3.238710539887,5.25291792606));
#19633=CARTESIAN_POINT('',(0.,4.975923633361,-0.4900857016478));
#19634=CARTESIAN_POINT('Origin',(0.,4.447521317429,1.256744568447));
#19635=CARTESIAN_POINT('',(1.486313498852,5.622770531748,-0.1394697002966));
#19636=CARTESIAN_POINT('',(4.313686501148,5.622770531748,-0.1394697002966));
#19637=CARTESIAN_POINT('Ctrl Pts',(1.48631349885238,5.62277053174818,-0.139469700296212));
#19638=CARTESIAN_POINT('Ctrl Pts',(1.66118098688117,5.49108295092936,-0.250316387196373));
#19639=CARTESIAN_POINT('Ctrl Pts',(1.88121857570613,5.36702914730511,-0.322542020921459));
#19640=CARTESIAN_POINT('Ctrl Pts',(2.37244120406318,5.19462115583365,-0.411265385296034));
#19641=CARTESIAN_POINT('Ctrl Pts',(2.64520960921171,5.15,-0.427639206271016));
#19642=CARTESIAN_POINT('Ctrl Pts',(3.1547903907883,5.15,-0.427639206271016));
#19643=CARTESIAN_POINT('Ctrl Pts',(3.42755879593682,5.19462115583365,-0.411265385296034));
#19644=CARTESIAN_POINT('Ctrl Pts',(3.91878142429387,5.36702914730511,-0.322542020921459));
#19645=CARTESIAN_POINT('Ctrl Pts',(4.13881901311883,5.49108295092936,-0.250316387196373));
#19646=CARTESIAN_POINT('Ctrl Pts',(4.31368650114762,5.62277053174818,-0.139469700296212));
#19647=CARTESIAN_POINT('',(4.313686501148,5.622770531748,-0.1394697002966));
#19648=CARTESIAN_POINT('',(0.,5.622770531748,-0.1394697002966));
#19649=CARTESIAN_POINT('Origin',(2.9,7.5,-1.79));
#19650=CARTESIAN_POINT('',(1.486313498852,5.622770531748,0.1394697002966));
#19651=CARTESIAN_POINT('Origin',(4.1885723820417,3.58518916149213,8.01442245901285E-15));
#19652=CARTESIAN_POINT('',(4.313686501148,5.622770531748,0.1394697002966));
#19653=CARTESIAN_POINT('Ctrl Pts',(4.31368650114762,5.62277053174818,0.139469700296214));
#19654=CARTESIAN_POINT('Ctrl Pts',(4.24213664876728,5.56888843465785,0.18482440959043));
#19655=CARTESIAN_POINT('Ctrl Pts',(4.16493748660703,5.51756625717708,0.222606776811208));
#19656=CARTESIAN_POINT('Ctrl Pts',(3.92608589772497,5.37734951975473,0.317908580005744));
#19657=CARTESIAN_POINT('Ctrl Pts',(3.73056477719256,5.29126942557444,0.362726320313873));
#19658=CARTESIAN_POINT('Ctrl Pts',(3.3177892926812,5.17754837590016,0.417070398131636));
#19659=CARTESIAN_POINT('Ctrl Pts',(3.10064734052485,5.15,0.427639206271016));
#19660=CARTESIAN_POINT('Ctrl Pts',(2.69935265947514,5.15,0.427639206271016));
#19661=CARTESIAN_POINT('Ctrl Pts',(2.4822107073188,5.17754837590016,0.417070398131637));
#19662=CARTESIAN_POINT('Ctrl Pts',(2.06943522280744,5.29126942557444,0.362726320313874));
#19663=CARTESIAN_POINT('Ctrl Pts',(1.87391410227503,5.37734951975473,0.317908580005744));
#19664=CARTESIAN_POINT('Ctrl Pts',(1.63506251339297,5.51756625717708,0.222606776811207));
#19665=CARTESIAN_POINT('Ctrl Pts',(1.55786335123272,5.56888843465785,0.18482440959043));
#19666=CARTESIAN_POINT('Ctrl Pts',(1.48631349885238,5.62277053174818,0.139469700296214));
#19667=CARTESIAN_POINT('Origin',(1.61142761795821,3.58518916149182,1.35308431126191E-14));
#19668=CARTESIAN_POINT('Origin',(0.,0.,0.));
#19669=CARTESIAN_POINT('',(0.,5.622770531748,0.1394697002966));
#19670=CARTESIAN_POINT('Origin',(0.,0.,0.));
#19671=CARTESIAN_POINT('',(4.313686501148,5.622770531748,0.1394697002966));
#19672=CARTESIAN_POINT('Origin',(0.,4.447521317429,-1.256744568447));
#19673=CARTESIAN_POINT('',(0.,4.975923633361,0.4900857016478));
#19674=CARTESIAN_POINT('Origin',(0.,3.238710539887,-5.25291792606));
#19675=CARTESIAN_POINT('Origin',(0.,0.9819737176534,6.092464223689));
#19676=CARTESIAN_POINT('',(0.,4.784701678661,1.451423386272));
#19677=CARTESIAN_POINT('Origin',(0.,3.628038590521,2.863073307653));
#19678=CARTESIAN_POINT('',(1.486313498852,5.24813535391,2.022887924981));
#19679=CARTESIAN_POINT('',(4.313686501148,5.24813535391,2.022887924981));
#19680=CARTESIAN_POINT('Ctrl Pts',(1.48631349885215,5.24813535391027,2.02288792498104));
#19681=CARTESIAN_POINT('Ctrl Pts',(1.66118098688097,5.16889108391505,1.87008428427961));
#19682=CARTESIAN_POINT('Ctrl Pts',(1.88121857570601,5.08191986723504,1.75588316418942));
#19683=CARTESIAN_POINT('Ctrl Pts',(2.37244120406315,4.95658861428298,1.60793578184472));
#19684=CARTESIAN_POINT('Ctrl Pts',(2.64520960921169,4.92163003170291,1.57573256670641));
#19685=CARTESIAN_POINT('Ctrl Pts',(3.15479039078831,4.92163003170291,1.57573256670641));
#19686=CARTESIAN_POINT('Ctrl Pts',(3.42755879593685,4.95658861428298,1.60793578184472));
#19687=CARTESIAN_POINT('Ctrl Pts',(3.91878142429399,5.08191986723504,1.75588316418942));
#19688=CARTESIAN_POINT('Ctrl Pts',(4.13881901311903,5.16889108391505,1.87008428427961));
#19689=CARTESIAN_POINT('Ctrl Pts',(4.31368650114785,5.24813535391027,2.02288792498104));
#19690=CARTESIAN_POINT('',(4.313686501148,5.24813535391,2.022887924981));
#19691=CARTESIAN_POINT('',(0.,5.24813535391,2.022887924981));
#19692=CARTESIAN_POINT('Origin',(2.9,7.614099837768,1.216381379543));
#19693=CARTESIAN_POINT('',(1.486313498852,5.14138986667,2.280594328));
#19694=CARTESIAN_POINT('Origin',(4.18857238240935,3.31228288622615,1.37199249389717));
#19695=CARTESIAN_POINT('',(4.313686501148,5.14138986667,2.280594328));
#19696=CARTESIAN_POINT('Ctrl Pts',(4.31368650114836,5.14138986666972,2.2805943280003));
#19697=CARTESIAN_POINT('Ctrl Pts',(4.2421366487679,5.07425280417236,2.30187682976273));
#19698=CARTESIAN_POINT('Ctrl Pts',(4.16493748660748,5.01237860886288,2.31714303849307));
#19699=CARTESIAN_POINT('Ctrl Pts',(3.92608589772523,4.84636481388562,2.35153180152409));
#19700=CARTESIAN_POINT('Ctrl Pts',(3.73056477719277,4.74968617002381,2.35999656858893));
#19701=CARTESIAN_POINT('Ctrl Pts',(3.31778929268131,4.62382504158597,2.36668478817641));
#19702=CARTESIAN_POINT('Ctrl Pts',(3.10064734052491,4.59432915316309,2.36590678665386));
#19703=CARTESIAN_POINT('Ctrl Pts',(2.69935265947509,4.59432915316309,2.36590678665386));
#19704=CARTESIAN_POINT('Ctrl Pts',(2.48221070731869,4.62382504158597,2.36668478817641));
#19705=CARTESIAN_POINT('Ctrl Pts',(2.06943522280723,4.74968617002381,2.35999656858893));
#19706=CARTESIAN_POINT('Ctrl Pts',(1.87391410227477,4.84636481388562,2.35153180152409));
#19707=CARTESIAN_POINT('Ctrl Pts',(1.63506251339252,5.01237860886288,2.31714303849307));
#19708=CARTESIAN_POINT('Ctrl Pts',(1.5578633512321,5.07425280417236,2.30187682976273));
#19709=CARTESIAN_POINT('Ctrl Pts',(1.48631349885164,5.14138986666971,2.2805943280003));
#19710=CARTESIAN_POINT('Origin',(1.61142761759052,3.31228288622493,1.37199249389661));
#19711=CARTESIAN_POINT('Origin',(0.,0.,0.));
#19712=CARTESIAN_POINT('',(0.,5.14138986667,2.280594328));
#19713=CARTESIAN_POINT('Origin',(0.,0.,0.));
#19714=CARTESIAN_POINT('',(4.313686501148,5.14138986667,2.280594328));
#19715=CARTESIAN_POINT('Origin',(0.,4.58990924064,0.5409121388882));
#19716=CARTESIAN_POINT('',(0.,4.409606321742,2.35698368413));
#19717=CARTESIAN_POINT('Origin',(0.,5.002383041407,-3.613662492007));
#19718=CARTESIAN_POINT('Origin',(0.,-1.424259701479,6.004488071588));
#19719=CARTESIAN_POINT('',(0.,3.865052266814,3.171966420818));
#19720=CARTESIAN_POINT('Origin',(0.,2.256219876458,4.033525089594));
#19721=CARTESIAN_POINT('',(1.486313498852,4.074519142905,3.877279201205));
#19722=CARTESIAN_POINT('',(4.313686501148,4.074519142905,3.877279201205));
#19723=CARTESIAN_POINT('Ctrl Pts',(1.48631349885213,4.07451914290497,3.87727920120514));
#19724=CARTESIAN_POINT('Ctrl Pts',(1.66118098688094,4.05978240548905,3.7057815758309));
#19725=CARTESIAN_POINT('Ctrl Pts',(1.88121857570594,4.02313435509682,3.56699105467367));
#19726=CARTESIAN_POINT('Ctrl Pts',(2.37244120406308,3.96396038779548,3.38234330217447));
#19727=CARTESIAN_POINT('Ctrl Pts',(2.64520960921165,3.94398650576646,3.33921334045477));
#19728=CARTESIAN_POINT('Ctrl Pts',(3.15479039078834,3.94398650576646,3.33921334045477));
#19729=CARTESIAN_POINT('Ctrl Pts',(3.42755879593693,3.96396038779548,3.38234330217447));
#19730=CARTESIAN_POINT('Ctrl Pts',(3.91878142429406,4.02313435509682,3.56699105467368));
#19731=CARTESIAN_POINT('Ctrl Pts',(4.13881901311905,4.05978240548905,3.7057815758309));
#19732=CARTESIAN_POINT('Ctrl Pts',(4.31368650114787,4.07451914290497,3.87727920120514));
#19733=CARTESIAN_POINT('',(4.313686501148,4.074519142905,3.877279201205));
#19734=CARTESIAN_POINT('',(0.,4.074519142905,3.877279201205));
#19735=CARTESIAN_POINT('Origin',(2.9,6.569021997223,4.037579720575));
#19736=CARTESIAN_POINT('',(1.486313498852,3.877279201205,4.074519142905));
#19737=CARTESIAN_POINT('Origin',(4.18857238224087,2.53511156782161,2.53511156782161));
#19738=CARTESIAN_POINT('',(4.313686501148,3.877279201205,4.074519142905));
#19739=CARTESIAN_POINT('Ctrl Pts',(4.31368650114786,3.87727920120514,4.07451914290497));
#19740=CARTESIAN_POINT('Ctrl Pts',(4.24213664876753,3.80710818246732,4.06848936916851));
#19741=CARTESIAN_POINT('Ctrl Pts',(4.16493748660728,3.74410175467432,4.05891527751768));
#19742=CARTESIAN_POINT('Ctrl Pts',(3.9260858977252,3.57756499750892,4.0271556229486));
#19743=CARTESIAN_POINT('Ctrl Pts',(3.73056477719275,3.48500625109951,3.99797873271785));
#19744=CARTESIAN_POINT('Ctrl Pts',(3.3177892926813,3.36616625976887,3.95599287327173));
#19745=CARTESIAN_POINT('Ctrl Pts',(3.1006473405249,3.33921334045477,3.94398650576646));
#19746=CARTESIAN_POINT('Ctrl Pts',(2.6993526594751,3.33921334045477,3.94398650576646));
#19747=CARTESIAN_POINT('Ctrl Pts',(2.4822107073187,3.36616625976887,3.95599287327173));
#19748=CARTESIAN_POINT('Ctrl Pts',(2.06943522280725,3.48500625109951,3.99797873271785));
#19749=CARTESIAN_POINT('Ctrl Pts',(1.8739141022748,3.57756499750892,4.0271556229486));
#19750=CARTESIAN_POINT('Ctrl Pts',(1.63506251339272,3.74410175467432,4.05891527751768));
#19751=CARTESIAN_POINT('Ctrl Pts',(1.55786335123247,3.80710818246732,4.06848936916851));
#19752=CARTESIAN_POINT('Ctrl Pts',(1.48631349885214,3.87727920120514,4.07451914290497));
#19753=CARTESIAN_POINT('Origin',(1.61142761775721,2.535111567821,2.53511156782107));
#19754=CARTESIAN_POINT('Origin',(0.,0.,0.));
#19755=CARTESIAN_POINT('',(0.,3.877279201205,4.074519142905));
#19756=CARTESIAN_POINT('Origin',(0.,0.,0.));
#19757=CARTESIAN_POINT('',(4.313686501148,3.877279201205,4.074519142905));
#19758=CARTESIAN_POINT('Origin',(0.,4.033525089594,2.256219876458));
#19759=CARTESIAN_POINT('',(0.,3.171966420818,3.865052266814));
#19760=CARTESIAN_POINT('Origin',(0.,6.004488071588,-1.424259701479));
#19761=CARTESIAN_POINT('Origin',(0.,-3.613662492007,5.002383041407));
#19762=CARTESIAN_POINT('',(0.,2.35698368413,4.409606321742));
#19763=CARTESIAN_POINT('Origin',(0.,0.5409121388882,4.58990924064));
#19764=CARTESIAN_POINT('',(1.486313498852,2.280594328,5.14138986667));
#19765=CARTESIAN_POINT('',(4.313686501148,2.280594328,5.14138986667));
#19766=CARTESIAN_POINT('Ctrl Pts',(1.48631349885156,2.28059432800033,5.14138986666964));
#19767=CARTESIAN_POINT('Ctrl Pts',(1.66118098688046,2.33260865784654,4.9773072154557));
#19768=CARTESIAN_POINT('Ctrl Pts',(1.88121857570565,2.35186310719892,4.83505689193819));
#19769=CARTESIAN_POINT('Ctrl Pts',(2.37244120406304,2.3678551256566,4.64181971576632));
#19770=CARTESIAN_POINT('Ctrl Pts',(2.64520960921164,2.36590678665386,4.59432915316297));
#19771=CARTESIAN_POINT('Ctrl Pts',(3.15479039078836,2.36590678665386,4.59432915316297));
#19772=CARTESIAN_POINT('Ctrl Pts',(3.42755879593696,2.3678551256566,4.64181971576632));
#19773=CARTESIAN_POINT('Ctrl Pts',(3.91878142429434,2.35186310719892,4.83505689193819));
#19774=CARTESIAN_POINT('Ctrl Pts',(4.13881901311954,2.33260865784654,4.9773072154557));
#19775=CARTESIAN_POINT('Ctrl Pts',(4.31368650114844,2.28059432800033,5.14138986666964));
#19776=CARTESIAN_POINT('',(4.313686501148,2.280594328,5.14138986667));
#19777=CARTESIAN_POINT('',(0.,2.280594328,5.14138986667));
#19778=CARTESIAN_POINT('Origin',(2.9,4.523870105933,6.244093149901));
#19779=CARTESIAN_POINT('',(1.486313498852,2.022887924981,5.24813535391));
#19780=CARTESIAN_POINT('Origin',(4.18857238256757,1.37199249385133,3.31228288611555));
#19781=CARTESIAN_POINT('',(4.313686501148,2.022887924981,5.24813535391));
#19782=CARTESIAN_POINT('Ctrl Pts',(4.31368650114793,2.02288792498097,5.24813535391023));
#19783=CARTESIAN_POINT('Ctrl Pts',(4.24213664876754,1.96036585150342,5.21571128306628));
#19784=CARTESIAN_POINT('Ctrl Pts',(4.16493748660722,1.90581934870347,5.18275445969878));
#19785=CARTESIAN_POINT('Ctrl Pts',(3.92608589772509,1.76411334096875,5.08968150703577));
#19786=CARTESIAN_POINT('Ctrl Pts',(3.73056477719266,1.68976572210544,5.0273048765579));
#19787=CARTESIAN_POINT('Ctrl Pts',(3.31778929268125,1.59603917927489,4.94303690457612));
#19788=CARTESIAN_POINT('Ctrl Pts',(3.10064734052488,1.57573256670632,4.92163003170282));
#19789=CARTESIAN_POINT('Ctrl Pts',(2.69935265947512,1.57573256670632,4.92163003170282));
#19790=CARTESIAN_POINT('Ctrl Pts',(2.48221070731875,1.59603917927489,4.94303690457612));
#19791=CARTESIAN_POINT('Ctrl Pts',(2.06943522280734,1.68976572210544,5.02730487655791));
#19792=CARTESIAN_POINT('Ctrl Pts',(1.87391410227491,1.76411334096875,5.08968150703577));
#19793=CARTESIAN_POINT('Ctrl Pts',(1.63506251339278,1.90581934870347,5.18275445969878));
#19794=CARTESIAN_POINT('Ctrl Pts',(1.55786335123246,1.96036585150342,5.21571128306628));
#19795=CARTESIAN_POINT('Ctrl Pts',(1.48631349885207,2.02288792498097,5.24813535391023));
#19796=CARTESIAN_POINT('Origin',(1.61142761743281,1.37199249385144,3.31228288611595));
#19797=CARTESIAN_POINT('Origin',(0.,0.,0.));
#19798=CARTESIAN_POINT('',(0.,2.022887924981,5.24813535391));
#19799=CARTESIAN_POINT('Origin',(0.,0.,0.));
#19800=CARTESIAN_POINT('',(4.313686501148,2.022887924981,5.24813535391));
#19801=CARTESIAN_POINT('Origin',(0.,2.863073307653,3.628038590521));
#19802=CARTESIAN_POINT('',(0.,1.451423386272,4.784701678661));
#19803=CARTESIAN_POINT('Origin',(0.,6.092464223689,0.9819737176533));
#19804=CARTESIAN_POINT('Origin',(0.,-5.25291792606,3.238710539887));
#19805=CARTESIAN_POINT('',(0.,0.4900857016478,4.975923633361));
#19806=CARTESIAN_POINT('Origin',(0.,-1.256744568447,4.447521317429));
#19807=CARTESIAN_POINT('',(1.486313498852,0.1394697002966,5.622770531748));
#19808=CARTESIAN_POINT('',(4.313686501148,0.1394697002966,5.622770531748));
#19809=CARTESIAN_POINT('Ctrl Pts',(1.48631349885238,0.139469700296212,5.62277053174818));
#19810=CARTESIAN_POINT('Ctrl Pts',(1.66118098688117,0.250316387196373,5.49108295092936));
#19811=CARTESIAN_POINT('Ctrl Pts',(1.88121857570613,0.322542020921459,5.36702914730511));
#19812=CARTESIAN_POINT('Ctrl Pts',(2.37244120406318,0.411265385296034,5.19462115583365));
#19813=CARTESIAN_POINT('Ctrl Pts',(2.64520960921171,0.427639206271016,5.15));
#19814=CARTESIAN_POINT('Ctrl Pts',(3.1547903907883,0.427639206271016,5.15));
#19815=CARTESIAN_POINT('Ctrl Pts',(3.42755879593682,0.411265385296034,5.19462115583365));
#19816=CARTESIAN_POINT('Ctrl Pts',(3.91878142429387,0.322542020921459,5.36702914730511));
#19817=CARTESIAN_POINT('Ctrl Pts',(4.13881901311883,0.250316387196373,5.49108295092936));
#19818=CARTESIAN_POINT('Ctrl Pts',(4.31368650114762,0.139469700296212,5.62277053174818));
#19819=CARTESIAN_POINT('',(4.313686501148,0.1394697002966,5.622770531748));
#19820=CARTESIAN_POINT('',(0.,0.1394697002966,5.622770531748));
#19821=CARTESIAN_POINT('Origin',(2.9,1.79,7.5));
#19822=CARTESIAN_POINT('',(1.486313498852,-0.1394697002966,5.622770531748));
#19823=CARTESIAN_POINT('Origin',(4.1885723820417,8.86270223876551E-14,3.58518916149213));
#19824=CARTESIAN_POINT('',(4.313686501148,-0.1394697002966,5.622770531748));
#19825=CARTESIAN_POINT('Ctrl Pts',(4.31368650114762,-0.139469700296214,
5.62277053174818));
#19826=CARTESIAN_POINT('Ctrl Pts',(4.24213664876728,-0.18482440959043,5.56888843465785));
#19827=CARTESIAN_POINT('Ctrl Pts',(4.16493748660703,-0.222606776811208,
5.51756625717708));
#19828=CARTESIAN_POINT('Ctrl Pts',(3.92608589772497,-0.317908580005744,
5.37734951975473));
#19829=CARTESIAN_POINT('Ctrl Pts',(3.73056477719256,-0.362726320313873,
5.29126942557444));
#19830=CARTESIAN_POINT('Ctrl Pts',(3.3177892926812,-0.417070398131636,5.17754837590016));
#19831=CARTESIAN_POINT('Ctrl Pts',(3.10064734052485,-0.427639206271016,
5.15));
#19832=CARTESIAN_POINT('Ctrl Pts',(2.69935265947514,-0.427639206271016,
5.15));
#19833=CARTESIAN_POINT('Ctrl Pts',(2.4822107073188,-0.417070398131636,5.17754837590016));
#19834=CARTESIAN_POINT('Ctrl Pts',(2.06943522280744,-0.362726320313873,
5.29126942557444));
#19835=CARTESIAN_POINT('Ctrl Pts',(1.87391410227503,-0.317908580005743,
5.37734951975473));
#19836=CARTESIAN_POINT('Ctrl Pts',(1.63506251339297,-0.222606776811207,
5.51756625717708));
#19837=CARTESIAN_POINT('Ctrl Pts',(1.55786335123272,-0.18482440959043,5.56888843465785));
#19838=CARTESIAN_POINT('Ctrl Pts',(1.48631349885238,-0.139469700296214,
5.62277053174818));
#19839=CARTESIAN_POINT('Origin',(1.61142761795821,-4.57273108267486E-14,
3.58518916149182));
#19840=CARTESIAN_POINT('Origin',(0.,0.,0.));
#19841=CARTESIAN_POINT('',(0.,-0.1394697002966,5.622770531748));
#19842=CARTESIAN_POINT('Origin',(0.,0.,0.));
#19843=CARTESIAN_POINT('',(4.313686501148,-0.1394697002966,5.622770531748));
#19844=CARTESIAN_POINT('Origin',(0.,1.256744568447,4.447521317429));
#19845=CARTESIAN_POINT('',(0.,-0.4900857016478,4.975923633361));
#19846=CARTESIAN_POINT('Origin',(0.,5.25291792606,3.238710539887));
#19847=CARTESIAN_POINT('Origin',(0.,-6.092464223689,0.9819737176534));
#19848=CARTESIAN_POINT('',(0.,-1.451423386272,4.784701678661));
#19849=CARTESIAN_POINT('Origin',(0.,-2.863073307653,3.628038590521));
#19850=CARTESIAN_POINT('',(1.486313498852,-2.022887924981,5.24813535391));
#19851=CARTESIAN_POINT('',(4.313686501148,-2.022887924981,5.24813535391));
#19852=CARTESIAN_POINT('Ctrl Pts',(1.48631349885215,-2.02288792498104,5.24813535391027));
#19853=CARTESIAN_POINT('Ctrl Pts',(1.66118098688097,-1.87008428427961,5.16889108391505));
#19854=CARTESIAN_POINT('Ctrl Pts',(1.88121857570601,-1.75588316418942,5.08191986723504));
#19855=CARTESIAN_POINT('Ctrl Pts',(2.37244120406315,-1.60793578184472,4.95658861428298));
#19856=CARTESIAN_POINT('Ctrl Pts',(2.64520960921169,-1.57573256670641,4.92163003170291));
#19857=CARTESIAN_POINT('Ctrl Pts',(3.15479039078831,-1.57573256670641,4.92163003170291));
#19858=CARTESIAN_POINT('Ctrl Pts',(3.42755879593685,-1.60793578184472,4.95658861428298));
#19859=CARTESIAN_POINT('Ctrl Pts',(3.91878142429399,-1.75588316418942,5.08191986723504));
#19860=CARTESIAN_POINT('Ctrl Pts',(4.13881901311903,-1.87008428427961,5.16889108391505));
#19861=CARTESIAN_POINT('Ctrl Pts',(4.31368650114785,-2.02288792498104,5.24813535391027));
#19862=CARTESIAN_POINT('',(4.313686501148,-2.022887924981,5.24813535391));
#19863=CARTESIAN_POINT('',(0.,-2.022887924981,5.24813535391));
#19864=CARTESIAN_POINT('Origin',(2.9,-1.216381379543,7.614099837768));
#19865=CARTESIAN_POINT('',(1.486313498852,-2.280594328,5.14138986667));
#19866=CARTESIAN_POINT('Origin',(4.18857238240928,-1.37199249389726,3.31228288622663));
#19867=CARTESIAN_POINT('',(4.313686501148,-2.280594328,5.14138986667));
#19868=CARTESIAN_POINT('Ctrl Pts',(4.31368650114836,-2.2805943280003,5.14138986666972));
#19869=CARTESIAN_POINT('Ctrl Pts',(4.2421366487679,-2.30187682976273,5.07425280417236));
#19870=CARTESIAN_POINT('Ctrl Pts',(4.16493748660748,-2.31714303849307,5.01237860886288));
#19871=CARTESIAN_POINT('Ctrl Pts',(3.92608589772523,-2.35153180152409,4.84636481388562));
#19872=CARTESIAN_POINT('Ctrl Pts',(3.73056477719277,-2.35999656858893,4.74968617002381));
#19873=CARTESIAN_POINT('Ctrl Pts',(3.31778929268131,-2.36668478817641,4.62382504158597));
#19874=CARTESIAN_POINT('Ctrl Pts',(3.10064734052491,-2.36590678665386,4.59432915316309));
#19875=CARTESIAN_POINT('Ctrl Pts',(2.69935265947509,-2.36590678665386,4.59432915316309));
#19876=CARTESIAN_POINT('Ctrl Pts',(2.48221070731869,-2.36668478817641,4.62382504158597));
#19877=CARTESIAN_POINT('Ctrl Pts',(2.06943522280723,-2.35999656858893,4.74968617002381));
#19878=CARTESIAN_POINT('Ctrl Pts',(1.87391410227477,-2.35153180152409,4.84636481388562));
#19879=CARTESIAN_POINT('Ctrl Pts',(1.63506251339252,-2.31714303849307,5.01237860886288));
#19880=CARTESIAN_POINT('Ctrl Pts',(1.5578633512321,-2.30187682976273,5.07425280417236));
#19881=CARTESIAN_POINT('Ctrl Pts',(1.48631349885164,-2.2805943280003,5.14138986666971));
#19882=CARTESIAN_POINT('Origin',(1.61142761759064,-1.37199249389664,3.31228288622489));
#19883=CARTESIAN_POINT('Origin',(0.,0.,0.));
#19884=CARTESIAN_POINT('',(0.,-2.280594328,5.14138986667));
#19885=CARTESIAN_POINT('Origin',(0.,0.,0.));
#19886=CARTESIAN_POINT('',(4.313686501148,-2.280594328,5.14138986667));
#19887=CARTESIAN_POINT('Origin',(0.,-0.5409121388882,4.58990924064));
#19888=CARTESIAN_POINT('',(0.,-2.35698368413,4.409606321742));
#19889=CARTESIAN_POINT('Origin',(0.,3.613662492007,5.002383041407));
#19890=CARTESIAN_POINT('Origin',(0.,-6.004488071588,-1.424259701479));
#19891=CARTESIAN_POINT('',(0.,-3.171966420818,3.865052266814));
#19892=CARTESIAN_POINT('Origin',(0.,-4.033525089594,2.256219876458));
#19893=CARTESIAN_POINT('',(1.486313498852,-3.877279201205,4.074519142905));
#19894=CARTESIAN_POINT('',(4.313686501148,-3.877279201205,4.074519142905));
#19895=CARTESIAN_POINT('Ctrl Pts',(1.48631349885213,-3.87727920120514,4.07451914290497));
#19896=CARTESIAN_POINT('Ctrl Pts',(1.66118098688094,-3.7057815758309,4.05978240548905));
#19897=CARTESIAN_POINT('Ctrl Pts',(1.88121857570595,-3.56699105467367,4.02313435509682));
#19898=CARTESIAN_POINT('Ctrl Pts',(2.37244120406308,-3.38234330217447,3.96396038779548));
#19899=CARTESIAN_POINT('Ctrl Pts',(2.64520960921165,-3.33921334045477,3.94398650576646));
#19900=CARTESIAN_POINT('Ctrl Pts',(3.15479039078834,-3.33921334045477,3.94398650576646));
#19901=CARTESIAN_POINT('Ctrl Pts',(3.42755879593693,-3.38234330217447,3.96396038779548));
#19902=CARTESIAN_POINT('Ctrl Pts',(3.91878142429406,-3.56699105467367,4.02313435509682));
#19903=CARTESIAN_POINT('Ctrl Pts',(4.13881901311906,-3.7057815758309,4.05978240548905));
#19904=CARTESIAN_POINT('Ctrl Pts',(4.31368650114787,-3.87727920120514,4.07451914290497));
#19905=CARTESIAN_POINT('',(4.313686501148,-3.877279201205,4.074519142905));
#19906=CARTESIAN_POINT('',(0.,-3.877279201205,4.074519142905));
#19907=CARTESIAN_POINT('Origin',(2.9,-4.037579720575,6.569021997223));
#19908=CARTESIAN_POINT('',(1.486313498852,-4.074519142905,3.877279201205));
#19909=CARTESIAN_POINT('Origin',(4.18857238224087,-2.53511156782161,2.53511156782161));
#19910=CARTESIAN_POINT('',(4.313686501148,-4.074519142905,3.877279201205));
#19911=CARTESIAN_POINT('Ctrl Pts',(4.31368650114787,-4.07451914290497,3.87727920120514));
#19912=CARTESIAN_POINT('Ctrl Pts',(4.24213664876753,-4.06848936916851,3.80710818246732));
#19913=CARTESIAN_POINT('Ctrl Pts',(4.16493748660728,-4.05891527751768,3.74410175467432));
#19914=CARTESIAN_POINT('Ctrl Pts',(3.9260858977252,-4.0271556229486,3.57756499750892));
#19915=CARTESIAN_POINT('Ctrl Pts',(3.73056477719275,-3.99797873271785,3.48500625109951));
#19916=CARTESIAN_POINT('Ctrl Pts',(3.3177892926813,-3.95599287327173,3.36616625976887));
#19917=CARTESIAN_POINT('Ctrl Pts',(3.1006473405249,-3.94398650576646,3.33921334045477));
#19918=CARTESIAN_POINT('Ctrl Pts',(2.6993526594751,-3.94398650576646,3.33921334045477));
#19919=CARTESIAN_POINT('Ctrl Pts',(2.4822107073187,-3.95599287327173,3.36616625976887));
#19920=CARTESIAN_POINT('Ctrl Pts',(2.06943522280725,-3.99797873271785,3.48500625109951));
#19921=CARTESIAN_POINT('Ctrl Pts',(1.8739141022748,-4.0271556229486,3.57756499750892));
#19922=CARTESIAN_POINT('Ctrl Pts',(1.63506251339272,-4.05891527751768,3.74410175467432));
#19923=CARTESIAN_POINT('Ctrl Pts',(1.55786335123247,-4.06848936916851,3.80710818246732));
#19924=CARTESIAN_POINT('Ctrl Pts',(1.48631349885214,-4.07451914290497,3.87727920120514));
#19925=CARTESIAN_POINT('Origin',(1.61142761775721,-2.53511156782107,2.535111567821));
#19926=CARTESIAN_POINT('Origin',(0.,0.,0.));
#19927=CARTESIAN_POINT('',(0.,-4.074519142905,3.877279201205));
#19928=CARTESIAN_POINT('Origin',(0.,0.,0.));
#19929=CARTESIAN_POINT('',(4.313686501148,-4.074519142905,3.877279201205));
#19930=CARTESIAN_POINT('Origin',(0.,-2.256219876458,4.033525089594));
#19931=CARTESIAN_POINT('',(0.,-3.865052266814,3.171966420818));
#19932=CARTESIAN_POINT('Origin',(0.,1.424259701479,6.004488071588));
#19933=CARTESIAN_POINT('Origin',(0.,-5.002383041407,-3.613662492007));
#19934=CARTESIAN_POINT('',(0.,-4.409606321742,2.35698368413));
#19935=CARTESIAN_POINT('Origin',(0.,-4.58990924064,0.5409121388882));
#19936=CARTESIAN_POINT('',(1.486313498852,-5.14138986667,2.280594328));
#19937=CARTESIAN_POINT('',(4.313686501148,-5.14138986667,2.280594328));
#19938=CARTESIAN_POINT('Ctrl Pts',(1.48631349885156,-5.14138986666964,2.28059432800033));
#19939=CARTESIAN_POINT('Ctrl Pts',(1.66118098688046,-4.9773072154557,2.33260865784654));
#19940=CARTESIAN_POINT('Ctrl Pts',(1.88121857570565,-4.83505689193818,2.35186310719892));
#19941=CARTESIAN_POINT('Ctrl Pts',(2.37244120406304,-4.64181971576632,2.3678551256566));
#19942=CARTESIAN_POINT('Ctrl Pts',(2.64520960921164,-4.59432915316297,2.36590678665386));
#19943=CARTESIAN_POINT('Ctrl Pts',(3.15479039078836,-4.59432915316297,2.36590678665386));
#19944=CARTESIAN_POINT('Ctrl Pts',(3.42755879593696,-4.64181971576632,2.3678551256566));
#19945=CARTESIAN_POINT('Ctrl Pts',(3.91878142429434,-4.83505689193819,2.35186310719892));
#19946=CARTESIAN_POINT('Ctrl Pts',(4.13881901311954,-4.9773072154557,2.33260865784654));
#19947=CARTESIAN_POINT('Ctrl Pts',(4.31368650114844,-5.14138986666964,2.28059432800033));
#19948=CARTESIAN_POINT('',(4.313686501148,-5.14138986667,2.280594328));
#19949=CARTESIAN_POINT('',(0.,-5.14138986667,2.280594328));
#19950=CARTESIAN_POINT('Origin',(2.9,-6.244093149901,4.523870105933));
#19951=CARTESIAN_POINT('',(1.486313498852,-5.24813535391,2.022887924981));
#19952=CARTESIAN_POINT('Origin',(4.18857238256757,-3.31228288611555,1.37199249385133));
#19953=CARTESIAN_POINT('',(4.313686501148,-5.24813535391,2.022887924981));
#19954=CARTESIAN_POINT('Ctrl Pts',(4.31368650114793,-5.24813535391023,2.02288792498097));
#19955=CARTESIAN_POINT('Ctrl Pts',(4.24213664876754,-5.21571128306628,1.96036585150342));
#19956=CARTESIAN_POINT('Ctrl Pts',(4.16493748660722,-5.18275445969878,1.90581934870347));
#19957=CARTESIAN_POINT('Ctrl Pts',(3.92608589772509,-5.08968150703577,1.76411334096875));
#19958=CARTESIAN_POINT('Ctrl Pts',(3.73056477719266,-5.0273048765579,1.68976572210544));
#19959=CARTESIAN_POINT('Ctrl Pts',(3.31778929268125,-4.94303690457612,1.59603917927489));
#19960=CARTESIAN_POINT('Ctrl Pts',(3.10064734052488,-4.92163003170282,1.57573256670632));
#19961=CARTESIAN_POINT('Ctrl Pts',(2.69935265947512,-4.92163003170282,1.57573256670632));
#19962=CARTESIAN_POINT('Ctrl Pts',(2.48221070731875,-4.94303690457612,1.59603917927489));
#19963=CARTESIAN_POINT('Ctrl Pts',(2.06943522280734,-5.02730487655791,1.68976572210544));
#19964=CARTESIAN_POINT('Ctrl Pts',(1.87391410227491,-5.08968150703577,1.76411334096875));
#19965=CARTESIAN_POINT('Ctrl Pts',(1.63506251339278,-5.18275445969878,1.90581934870347));
#19966=CARTESIAN_POINT('Ctrl Pts',(1.55786335123246,-5.21571128306628,1.96036585150342));
#19967=CARTESIAN_POINT('Ctrl Pts',(1.48631349885208,-5.24813535391023,2.02288792498097));
#19968=CARTESIAN_POINT('Origin',(1.61142761743281,-3.31228288611595,1.37199249385144));
#19969=CARTESIAN_POINT('Origin',(0.,0.,0.));
#19970=CARTESIAN_POINT('',(0.,-5.24813535391,2.022887924981));
#19971=CARTESIAN_POINT('Origin',(0.,0.,0.));
#19972=CARTESIAN_POINT('',(4.313686501148,-5.24813535391,2.022887924981));
#19973=CARTESIAN_POINT('Origin',(0.,-3.628038590521,2.863073307653));
#19974=CARTESIAN_POINT('',(0.,-4.784701678661,1.451423386272));
#19975=CARTESIAN_POINT('Origin',(0.,-0.9819737176534,6.092464223689));
#19976=CARTESIAN_POINT('Origin',(0.,-3.238710539887,-5.25291792606));
#19977=CARTESIAN_POINT('',(0.,-4.975923633361,0.4900857016478));
#19978=CARTESIAN_POINT('Origin',(0.,-4.447521317429,-1.256744568447));
#19979=CARTESIAN_POINT('',(1.486313498852,-5.622770531748,0.1394697002966));
#19980=CARTESIAN_POINT('',(4.313686501148,-5.622770531748,0.1394697002966));
#19981=CARTESIAN_POINT('Ctrl Pts',(1.48631349885238,-5.62277053174818,0.139469700296212));
#19982=CARTESIAN_POINT('Ctrl Pts',(1.66118098688117,-5.49108295092936,0.250316387196373));
#19983=CARTESIAN_POINT('Ctrl Pts',(1.88121857570613,-5.36702914730511,0.322542020921459));
#19984=CARTESIAN_POINT('Ctrl Pts',(2.37244120406318,-5.19462115583365,0.411265385296034));
#19985=CARTESIAN_POINT('Ctrl Pts',(2.64520960921171,-5.15,0.427639206271016));
#19986=CARTESIAN_POINT('Ctrl Pts',(3.1547903907883,-5.15,0.427639206271016));
#19987=CARTESIAN_POINT('Ctrl Pts',(3.42755879593682,-5.19462115583365,0.411265385296034));
#19988=CARTESIAN_POINT('Ctrl Pts',(3.91878142429387,-5.36702914730511,0.322542020921459));
#19989=CARTESIAN_POINT('Ctrl Pts',(4.13881901311883,-5.49108295092936,0.250316387196373));
#19990=CARTESIAN_POINT('Ctrl Pts',(4.31368650114762,-5.62277053174818,0.139469700296212));
#19991=CARTESIAN_POINT('',(4.313686501148,-5.622770531748,0.1394697002966));
#19992=CARTESIAN_POINT('',(0.,-5.622770531748,0.1394697002966));
#19993=CARTESIAN_POINT('Origin',(2.9,-7.5,1.79));
#19994=CARTESIAN_POINT('',(1.486313498852,-5.622770531748,-0.1394697002966));
#19995=CARTESIAN_POINT('Origin',(4.1885723820417,-3.58518916149213,2.41993924898765E-14));
#19996=CARTESIAN_POINT('',(4.313686501148,-5.622770531748,-0.1394697002966));
#19997=CARTESIAN_POINT('Ctrl Pts',(4.31368650114762,-5.62277053174818,-0.139469700296214));
#19998=CARTESIAN_POINT('Ctrl Pts',(4.24213664876728,-5.56888843465785,-0.18482440959043));
#19999=CARTESIAN_POINT('Ctrl Pts',(4.16493748660703,-5.51756625717708,-0.222606776811208));
#20000=CARTESIAN_POINT('Ctrl Pts',(3.92608589772497,-5.37734951975473,-0.317908580005744));
#20001=CARTESIAN_POINT('Ctrl Pts',(3.73056477719256,-5.29126942557444,-0.362726320313873));
#20002=CARTESIAN_POINT('Ctrl Pts',(3.3177892926812,-5.17754837590016,-0.417070398131636));
#20003=CARTESIAN_POINT('Ctrl Pts',(3.10064734052485,-5.15,-0.427639206271016));
#20004=CARTESIAN_POINT('Ctrl Pts',(2.69935265947514,-5.15,-0.427639206271016));
#20005=CARTESIAN_POINT('Ctrl Pts',(2.4822107073188,-5.17754837590016,-0.417070398131637));
#20006=CARTESIAN_POINT('Ctrl Pts',(2.06943522280744,-5.29126942557444,-0.362726320313874));
#20007=CARTESIAN_POINT('Ctrl Pts',(1.87391410227503,-5.37734951975473,-0.317908580005744));
#20008=CARTESIAN_POINT('Ctrl Pts',(1.63506251339297,-5.51756625717708,-0.222606776811207));
#20009=CARTESIAN_POINT('Ctrl Pts',(1.55786335123272,-5.56888843465785,-0.18482440959043));
#20010=CARTESIAN_POINT('Ctrl Pts',(1.48631349885238,-5.62277053174818,-0.139469700296214));
#20011=CARTESIAN_POINT('Origin',(1.61142761795821,-3.58518916149182,1.86829718362702E-14));
#20012=CARTESIAN_POINT('Origin',(0.,0.,0.));
#20013=CARTESIAN_POINT('',(0.,-5.622770531748,-0.1394697002966));
#20014=CARTESIAN_POINT('Origin',(0.,0.,0.));
#20015=CARTESIAN_POINT('',(4.313686501148,-5.622770531748,-0.1394697002966));
#20016=CARTESIAN_POINT('Origin',(0.,-4.447521317429,1.256744568447));
#20017=CARTESIAN_POINT('',(0.,-4.975923633361,-0.4900857016478));
#20018=CARTESIAN_POINT('Origin',(0.,-3.238710539887,5.25291792606));
#20019=CARTESIAN_POINT('Origin',(0.,-0.9819737176534,-6.092464223689));
#20020=CARTESIAN_POINT('',(0.,-4.784701678661,-1.451423386272));
#20021=CARTESIAN_POINT('Origin',(0.,-3.628038590521,-2.863073307653));
#20022=CARTESIAN_POINT('',(1.486313498852,-5.24813535391,-2.022887924981));
#20023=CARTESIAN_POINT('',(4.313686501148,-5.24813535391,-2.022887924981));
#20024=CARTESIAN_POINT('Ctrl Pts',(1.48631349885215,-5.24813535391027,-2.02288792498104));
#20025=CARTESIAN_POINT('Ctrl Pts',(1.66118098688097,-5.16889108391505,-1.87008428427961));
#20026=CARTESIAN_POINT('Ctrl Pts',(1.88121857570601,-5.08191986723504,-1.75588316418942));
#20027=CARTESIAN_POINT('Ctrl Pts',(2.37244120406315,-4.95658861428298,-1.60793578184472));
#20028=CARTESIAN_POINT('Ctrl Pts',(2.64520960921169,-4.92163003170291,-1.57573256670641));
#20029=CARTESIAN_POINT('Ctrl Pts',(3.15479039078831,-4.92163003170291,-1.57573256670641));
#20030=CARTESIAN_POINT('Ctrl Pts',(3.42755879593685,-4.95658861428298,-1.60793578184472));
#20031=CARTESIAN_POINT('Ctrl Pts',(3.91878142429399,-5.08191986723504,-1.75588316418942));
#20032=CARTESIAN_POINT('Ctrl Pts',(4.13881901311903,-5.16889108391505,-1.87008428427961));
#20033=CARTESIAN_POINT('Ctrl Pts',(4.31368650114785,-5.24813535391027,-2.02288792498104));
#20034=CARTESIAN_POINT('',(4.313686501148,-5.24813535391,-2.022887924981));
#20035=CARTESIAN_POINT('',(0.,-5.24813535391,-2.022887924981));
#20036=CARTESIAN_POINT('Origin',(2.9,-7.614099837768,-1.216381379543));
#20037=CARTESIAN_POINT('',(1.486313498852,-5.14138986667,-2.280594328));
#20038=CARTESIAN_POINT('Origin',(4.18857238240935,-3.31228288622615,-1.37199249389717));
#20039=CARTESIAN_POINT('',(4.313686501148,-5.14138986667,-2.280594328));
#20040=CARTESIAN_POINT('Ctrl Pts',(4.31368650114836,-5.14138986666972,-2.2805943280003));
#20041=CARTESIAN_POINT('Ctrl Pts',(4.2421366487679,-5.07425280417236,-2.30187682976273));
#20042=CARTESIAN_POINT('Ctrl Pts',(4.16493748660748,-5.01237860886288,-2.31714303849307));
#20043=CARTESIAN_POINT('Ctrl Pts',(3.92608589772523,-4.84636481388562,-2.35153180152409));
#20044=CARTESIAN_POINT('Ctrl Pts',(3.73056477719277,-4.74968617002381,-2.35999656858893));
#20045=CARTESIAN_POINT('Ctrl Pts',(3.31778929268131,-4.62382504158597,-2.36668478817641));
#20046=CARTESIAN_POINT('Ctrl Pts',(3.10064734052491,-4.59432915316309,-2.36590678665386));
#20047=CARTESIAN_POINT('Ctrl Pts',(2.69935265947509,-4.59432915316309,-2.36590678665386));
#20048=CARTESIAN_POINT('Ctrl Pts',(2.48221070731869,-4.62382504158597,-2.36668478817641));
#20049=CARTESIAN_POINT('Ctrl Pts',(2.06943522280723,-4.74968617002381,-2.35999656858893));
#20050=CARTESIAN_POINT('Ctrl Pts',(1.87391410227477,-4.84636481388562,-2.35153180152409));
#20051=CARTESIAN_POINT('Ctrl Pts',(1.63506251339252,-5.01237860886288,-2.31714303849307));
#20052=CARTESIAN_POINT('Ctrl Pts',(1.5578633512321,-5.07425280417236,-2.30187682976273));
#20053=CARTESIAN_POINT('Ctrl Pts',(1.48631349885164,-5.14138986666971,-2.2805943280003));
#20054=CARTESIAN_POINT('Origin',(1.61142761759052,-3.31228288622493,-1.37199249389661));
#20055=CARTESIAN_POINT('Origin',(0.,0.,0.));
#20056=CARTESIAN_POINT('',(0.,-5.14138986667,-2.280594328));
#20057=CARTESIAN_POINT('Origin',(0.,0.,0.));
#20058=CARTESIAN_POINT('',(4.313686501148,-5.14138986667,-2.280594328));
#20059=CARTESIAN_POINT('Origin',(0.,-4.58990924064,-0.5409121388882));
#20060=CARTESIAN_POINT('',(0.,-4.409606321742,-2.35698368413));
#20061=CARTESIAN_POINT('Origin',(0.,-5.002383041407,3.613662492007));
#20062=CARTESIAN_POINT('Origin',(0.,1.424259701479,-6.004488071588));
#20063=CARTESIAN_POINT('',(0.,-3.865052266814,-3.171966420818));
#20064=CARTESIAN_POINT('Origin',(0.,-2.256219876458,-4.033525089594));
#20065=CARTESIAN_POINT('',(1.486313498852,-4.074519142905,-3.877279201205));
#20066=CARTESIAN_POINT('',(4.313686501148,-4.074519142905,-3.877279201205));
#20067=CARTESIAN_POINT('Ctrl Pts',(1.48631349885213,-4.07451914290497,-3.87727920120514));
#20068=CARTESIAN_POINT('Ctrl Pts',(1.66118098688094,-4.05978240548905,-3.7057815758309));
#20069=CARTESIAN_POINT('Ctrl Pts',(1.88121857570594,-4.02313435509682,-3.56699105467367));
#20070=CARTESIAN_POINT('Ctrl Pts',(2.37244120406308,-3.96396038779548,-3.38234330217447));
#20071=CARTESIAN_POINT('Ctrl Pts',(2.64520960921165,-3.94398650576646,-3.33921334045477));
#20072=CARTESIAN_POINT('Ctrl Pts',(3.15479039078834,-3.94398650576646,-3.33921334045477));
#20073=CARTESIAN_POINT('Ctrl Pts',(3.42755879593693,-3.96396038779548,-3.38234330217447));
#20074=CARTESIAN_POINT('Ctrl Pts',(3.91878142429406,-4.02313435509682,-3.56699105467368));
#20075=CARTESIAN_POINT('Ctrl Pts',(4.13881901311905,-4.05978240548905,-3.7057815758309));
#20076=CARTESIAN_POINT('Ctrl Pts',(4.31368650114787,-4.07451914290497,-3.87727920120514));
#20077=CARTESIAN_POINT('',(4.313686501148,-4.074519142905,-3.877279201205));
#20078=CARTESIAN_POINT('',(0.,-4.074519142905,-3.877279201205));
#20079=CARTESIAN_POINT('Origin',(2.9,-6.569021997223,-4.037579720575));
#20080=CARTESIAN_POINT('',(1.486313498852,-3.877279201205,-4.074519142905));
#20081=CARTESIAN_POINT('Origin',(4.18857238224087,-2.53511156782161,-2.53511156782161));
#20082=CARTESIAN_POINT('',(4.313686501148,-3.877279201205,-4.074519142905));
#20083=CARTESIAN_POINT('Ctrl Pts',(4.31368650114786,-3.87727920120514,-4.07451914290497));
#20084=CARTESIAN_POINT('Ctrl Pts',(4.24213664876753,-3.80710818246732,-4.06848936916851));
#20085=CARTESIAN_POINT('Ctrl Pts',(4.16493748660728,-3.74410175467432,-4.05891527751768));
#20086=CARTESIAN_POINT('Ctrl Pts',(3.9260858977252,-3.57756499750892,-4.0271556229486));
#20087=CARTESIAN_POINT('Ctrl Pts',(3.73056477719275,-3.48500625109951,-3.99797873271785));
#20088=CARTESIAN_POINT('Ctrl Pts',(3.3177892926813,-3.36616625976887,-3.95599287327173));
#20089=CARTESIAN_POINT('Ctrl Pts',(3.1006473405249,-3.33921334045477,-3.94398650576646));
#20090=CARTESIAN_POINT('Ctrl Pts',(2.6993526594751,-3.33921334045477,-3.94398650576646));
#20091=CARTESIAN_POINT('Ctrl Pts',(2.4822107073187,-3.36616625976887,-3.95599287327173));
#20092=CARTESIAN_POINT('Ctrl Pts',(2.06943522280725,-3.48500625109951,-3.99797873271785));
#20093=CARTESIAN_POINT('Ctrl Pts',(1.8739141022748,-3.57756499750892,-4.0271556229486));
#20094=CARTESIAN_POINT('Ctrl Pts',(1.63506251339272,-3.74410175467432,-4.05891527751768));
#20095=CARTESIAN_POINT('Ctrl Pts',(1.55786335123247,-3.80710818246732,-4.06848936916851));
#20096=CARTESIAN_POINT('Ctrl Pts',(1.48631349885214,-3.87727920120514,-4.07451914290497));
#20097=CARTESIAN_POINT('Origin',(1.61142761775721,-2.535111567821,-2.53511156782107));
#20098=CARTESIAN_POINT('Origin',(0.,0.,0.));
#20099=CARTESIAN_POINT('',(0.,-3.877279201205,-4.074519142905));
#20100=CARTESIAN_POINT('Origin',(0.,0.,0.));
#20101=CARTESIAN_POINT('',(4.313686501148,-3.877279201205,-4.074519142905));
#20102=CARTESIAN_POINT('Origin',(0.,-4.033525089594,-2.256219876458));
#20103=CARTESIAN_POINT('',(0.,-3.171966420818,-3.865052266814));
#20104=CARTESIAN_POINT('Origin',(0.,-6.004488071588,1.424259701479));
#20105=CARTESIAN_POINT('Origin',(0.,-6.092464223689,-0.9819737176534));
#20106=CARTESIAN_POINT('',(0.,-1.451423386272,-4.784701678661));
#20107=CARTESIAN_POINT('Origin',(0.,-2.863073307653,-3.628038590521));
#20108=CARTESIAN_POINT('',(4.313686501148,-2.022887924981,-5.24813535391));
#20109=CARTESIAN_POINT('',(1.486313498852,-2.022887924981,-5.24813535391));
#20110=CARTESIAN_POINT('Ctrl Pts',(4.31368650114793,-2.02288792498097,-5.24813535391023));
#20111=CARTESIAN_POINT('Ctrl Pts',(4.1388190131191,-1.87008428427953,-5.168891083915));
#20112=CARTESIAN_POINT('Ctrl Pts',(3.91878142429405,-1.75588316418934,-5.08191986723497));
#20113=CARTESIAN_POINT('Ctrl Pts',(3.42755879593687,-1.60793578184463,-4.95658861428289));
#20114=CARTESIAN_POINT('Ctrl Pts',(3.15479039078832,-1.57573256670632,-4.92163003170282));
#20115=CARTESIAN_POINT('Ctrl Pts',(2.9,-1.57573256670632,-4.92163003170282));
#20116=CARTESIAN_POINT('Ctrl Pts',(2.64520960921168,-1.57573256670632,-4.92163003170282));
#20117=CARTESIAN_POINT('Ctrl Pts',(2.37244120406312,-1.60793578184463,-4.95658861428289));
#20118=CARTESIAN_POINT('Ctrl Pts',(1.88121857570595,-1.75588316418934,-5.08191986723497));
#20119=CARTESIAN_POINT('Ctrl Pts',(1.6611809868809,-1.87008428427953,-5.168891083915));
#20120=CARTESIAN_POINT('Ctrl Pts',(1.48631349885207,-2.02288792498097,-5.24813535391023));
#20121=CARTESIAN_POINT('',(0.,-2.022887924981,-5.24813535391));
#20122=CARTESIAN_POINT('',(4.313686501148,-2.022887924981,-5.24813535391));
#20123=CARTESIAN_POINT('Origin',(2.9,-4.523870105933,-6.244093149901));
#20124=CARTESIAN_POINT('',(1.486313498852,-2.280594328,-5.14138986667));
#20125=CARTESIAN_POINT('',(4.313686501148,-2.280594328,-5.14138986667));
#20126=CARTESIAN_POINT('Ctrl Pts',(1.48631349885156,-2.28059432800033,-5.14138986666964));
#20127=CARTESIAN_POINT('Ctrl Pts',(1.55786335123203,-2.30187682976275,-5.07425280417228));
#20128=CARTESIAN_POINT('Ctrl Pts',(1.63506251339245,-2.31714303849309,-5.01237860886279));
#20129=CARTESIAN_POINT('Ctrl Pts',(1.87391410227472,-2.35153180152411,-4.84636481388551));
#20130=CARTESIAN_POINT('Ctrl Pts',(2.06943522280718,-2.35999656858894,-4.7496861700237));
#20131=CARTESIAN_POINT('Ctrl Pts',(2.48221070731866,-2.36668478817641,-4.62382504158585));
#20132=CARTESIAN_POINT('Ctrl Pts',(2.69935265947508,-2.36590678665386,-4.59432915316297));
#20133=CARTESIAN_POINT('Ctrl Pts',(3.10064734052492,-2.36590678665386,-4.59432915316297));
#20134=CARTESIAN_POINT('Ctrl Pts',(3.31778929268134,-2.36668478817641,-4.62382504158585));
#20135=CARTESIAN_POINT('Ctrl Pts',(3.73056477719282,-2.35999656858894,-4.7496861700237));
#20136=CARTESIAN_POINT('Ctrl Pts',(3.92608589772528,-2.35153180152411,-4.84636481388551));
#20137=CARTESIAN_POINT('Ctrl Pts',(4.16493748660755,-2.31714303849309,-5.01237860886279));
#20138=CARTESIAN_POINT('Ctrl Pts',(4.24213664876797,-2.30187682976275,-5.07425280417228));
#20139=CARTESIAN_POINT('Ctrl Pts',(4.31368650114844,-2.28059432800033,-5.14138986666964));
#20140=CARTESIAN_POINT('Origin',(4.1885723823212,-1.37199249392222,-3.31228288628699));
#20141=CARTESIAN_POINT('Origin',(1.61142761767967,-1.37199249392214,-3.31228288628656));
#20142=CARTESIAN_POINT('Origin',(0.,-0.5409121388882,-4.58990924064));
#20143=CARTESIAN_POINT('',(4.313686501148,-2.280594328,-5.14138986667));
#20144=CARTESIAN_POINT('',(0.,-2.35698368413,-4.409606321742));
#20145=CARTESIAN_POINT('',(0.,-2.280594328,-5.14138986667));
#20146=CARTESIAN_POINT('Origin',(0.,0.,0.));
#20147=CARTESIAN_POINT('Origin',(0.,0.,0.));
#20148=CARTESIAN_POINT('Origin',(0.,3.613662492007,-5.002383041407));
#20149=CARTESIAN_POINT('',(0.,0.,0.));
#20150=CARTESIAN_POINT('Origin',(0.,0.,-27.8));
#20151=CARTESIAN_POINT('',(3.67394039744206E-16,3.,-27.8));
#20152=CARTESIAN_POINT('Origin',(0.,0.,-27.8));
#20153=CARTESIAN_POINT('',(-2.1,1.212435565298,-27.8));
#20154=CARTESIAN_POINT('',(0.,2.424871130596,-27.8));
#20155=CARTESIAN_POINT('',(-2.1,1.212435565298,-27.8));
#20156=CARTESIAN_POINT('',(-2.1,-1.212435565298,-27.8));
#20157=CARTESIAN_POINT('',(-2.1,-1.212435565298,-27.8));
#20158=CARTESIAN_POINT('',(0.,-2.424871130596,-27.8));
#20159=CARTESIAN_POINT('',(0.,-2.424871130596,-27.8));
#20160=CARTESIAN_POINT('',(2.1,-1.212435565298,-27.8));
#20161=CARTESIAN_POINT('',(2.1,-1.212435565298,-27.8));
#20162=CARTESIAN_POINT('',(2.1,1.212435565298,-27.8));
#20163=CARTESIAN_POINT('',(2.1,1.212435565298,-27.8));
#20164=CARTESIAN_POINT('',(0.,2.424871130596,-27.8));
#20165=CARTESIAN_POINT('Origin',(0.,0.,0.79));
#20166=CARTESIAN_POINT('',(3.67394039744206E-16,3.,-7.8));
#20167=CARTESIAN_POINT('',(3.67394039744206E-16,3.,0.79));
#20168=CARTESIAN_POINT('Origin',(0.,0.,-7.8));
#20169=CARTESIAN_POINT('Origin',(0.,0.,0.79));
#20170=CARTESIAN_POINT('',(0.,3.,-2.));
#20171=CARTESIAN_POINT('Origin',(0.,0.,-2.));
#20172=CARTESIAN_POINT('',(0.,3.,-1.));
#20173=CARTESIAN_POINT('',(3.67394039744206E-16,3.,0.79));
#20174=CARTESIAN_POINT('Origin',(0.,0.,-1.));
#20175=CARTESIAN_POINT('Origin',(0.,0.,-4.9));
#20176=CARTESIAN_POINT('Origin',(8.211256788283E-16,6.705,-4.9));
#20177=CARTESIAN_POINT('',(1.786057109949,0.9,-4.9));
#20178=CARTESIAN_POINT('Ctrl Pts',(2.08688079408944,-6.93889390390723E-17,
-5.8));
#20179=CARTESIAN_POINT('Ctrl Pts',(2.08688079408944,-0.101093267950358,
-5.8));
#20180=CARTESIAN_POINT('Ctrl Pts',(2.07606256936626,-0.200116780800449,
-5.78306010664896));
#20181=CARTESIAN_POINT('Ctrl Pts',(2.03456000012612,-0.400564730585056,
-5.7138100508258));
#20182=CARTESIAN_POINT('Ctrl Pts',(2.00198415673787,-0.497484683785943,
-5.65792591947954));
#20183=CARTESIAN_POINT('Ctrl Pts',(1.92762106375197,-0.672219726341367,
-5.51024657908061));
#20184=CARTESIAN_POINT('Ctrl Pts',(1.88521703073068,-0.747655625946073,
-5.41535484251112));
#20185=CARTESIAN_POINT('Ctrl Pts',(1.82963665913354,-0.837307075018212,
-5.23892457904444));
#20186=CARTESIAN_POINT('Ctrl Pts',(1.81154384378188,-0.863748989480202,
-5.16502186650821));
#20187=CARTESIAN_POINT('Ctrl Pts',(1.79307858729398,-0.890223641153724,
-5.04065959660885));
#20188=CARTESIAN_POINT('Ctrl Pts',(1.78858372602067,-0.896476659347317,
-4.99305285657899));
#20189=CARTESIAN_POINT('Ctrl Pts',(1.78533316749339,-0.901010715882009,
-4.90218285810826));
#20190=CARTESIAN_POINT('Ctrl Pts',(1.78599302794454,-0.900100579704181,
-4.85952137824838));
#20191=CARTESIAN_POINT('Ctrl Pts',(1.79231868802101,-0.891241854858108,
-4.76381818537325));
#20192=CARTESIAN_POINT('Ctrl Pts',(1.79916641606907,-0.881638078648367,
-4.71160904837683));
#20193=CARTESIAN_POINT('Ctrl Pts',(1.82686643689218,-0.84116912475279,-4.56481378587192));
#20194=CARTESIAN_POINT('Ctrl Pts',(1.85446030150783,-0.799437867210863,
-4.47550957740264));
#20195=CARTESIAN_POINT('Ctrl Pts',(1.91932437559004,-0.684995961096764,
-4.30636138511348));
#20196=CARTESIAN_POINT('Ctrl Pts',(1.95740679794227,-0.608819659462653,
-4.22838203723553));
#20197=CARTESIAN_POINT('Ctrl Pts',(2.02485323182035,-0.430006700487911,
-4.1016362333799));
#20198=CARTESIAN_POINT('Ctrl Pts',(2.05383693479979,-0.327023915525718,
-4.05368786483531));
#20199=CARTESIAN_POINT('Ctrl Pts',(2.08565111645498,-0.116269187541378,
-4.00170605857396));
#20200=CARTESIAN_POINT('Ctrl Pts',(2.09048597736785,-0.0135717077347775,
-3.99421211556224));
#20201=CARTESIAN_POINT('Ctrl Pts',(2.07776710291235,0.191484033440727,-4.01460189690483));
#20202=CARTESIAN_POINT('Ctrl Pts',(2.06053976427926,0.289671925625122,-4.04202503782963));
#20203=CARTESIAN_POINT('Ctrl Pts',(2.00671918893296,0.488728582767382,-4.13487097478375));
#20204=CARTESIAN_POINT('Ctrl Pts',(1.96758297172864,0.5844436089876,-4.20573850098139));
#20205=CARTESIAN_POINT('Ctrl Pts',(1.88908829229802,0.743279797016495,-4.37887910454814));
#20206=CARTESIAN_POINT('Ctrl Pts',(1.84955679967837,0.806500365822469,-4.48238860864025));
#20207=CARTESIAN_POINT('Ctrl Pts',(1.80880106698392,0.867867222875822,-4.65409622882472));
#20208=CARTESIAN_POINT('Ctrl Pts',(1.79841793711201,0.882619607672314,-4.7134689255317));
#20209=CARTESIAN_POINT('Ctrl Pts',(1.7880296495206,0.897274433692566,-4.81762265188009));
#20210=CARTESIAN_POINT('Ctrl Pts',(1.78590159063484,0.900216573916412,-4.86106047100695));
#20211=CARTESIAN_POINT('Ctrl Pts',(1.78623446722923,0.899753015094058,-4.94945829210191));
#20212=CARTESIAN_POINT('Ctrl Pts',(1.78880867985365,0.896191473409593,-4.99391013963609));
#20213=CARTESIAN_POINT('Ctrl Pts',(1.80063381565783,0.879464182449665,-5.10182083332412));
#20214=CARTESIAN_POINT('Ctrl Pts',(1.81229274734386,0.862820879832989,-5.16372701080558));
#20215=CARTESIAN_POINT('Ctrl Pts',(1.85616772350585,0.796015468290225,-5.33756367316692));
#20216=CARTESIAN_POINT('Ctrl Pts',(1.89697738935018,0.729525882843482,-5.44051832736629));
#20217=CARTESIAN_POINT('Ctrl Pts',(1.97477477835702,0.567312731060949,-5.60778248302471));
#20218=CARTESIAN_POINT('Ctrl Pts',(2.01201382633158,0.472866430429607,-5.67453279408918));
#20219=CARTESIAN_POINT('Ctrl Pts',(2.05457838510613,0.309311014743862,-5.74751544509335));
#20220=CARTESIAN_POINT('Ctrl Pts',(2.06663910190596,0.248843270470049,-5.76728897745186));
#20221=CARTESIAN_POINT('Ctrl Pts',(2.08273777581834,0.1251203935021,-5.79343657211952));
#20222=CARTESIAN_POINT('Ctrl Pts',(2.08688079408944,0.0628253026847131,
-5.8));
#20223=CARTESIAN_POINT('Ctrl Pts',(2.08688079408944,-1.27784594234186E-16,
-5.8));
#20224=CARTESIAN_POINT('',(-1.786057109949,-0.9,-4.9));
#20225=CARTESIAN_POINT('',(-1.78605710994918,0.9,-4.9));
#20226=CARTESIAN_POINT('Ctrl Pts',(-1.78605710994918,-0.9,-4.9));
#20227=CARTESIAN_POINT('Ctrl Pts',(-1.78605710994918,-0.9,-4.90157288708411));
#20228=CARTESIAN_POINT('Ctrl Pts',(-1.78606007091103,-0.899995876722818,
-4.90314607070815));
#20229=CARTESIAN_POINT('Ctrl Pts',(-1.78623446722923,-0.899753015094059,
-4.9494582921019));
#20230=CARTESIAN_POINT('Ctrl Pts',(-1.78880867985365,-0.896191473409595,
-4.99391013963609));
#20231=CARTESIAN_POINT('Ctrl Pts',(-1.80063381565783,-0.879464182449664,
-5.10182083332413));
#20232=CARTESIAN_POINT('Ctrl Pts',(-1.81229274734387,-0.862820879832981,
-5.1637270108056));
#20233=CARTESIAN_POINT('Ctrl Pts',(-1.85616772350585,-0.796015468290225,
-5.33756367316691));
#20234=CARTESIAN_POINT('Ctrl Pts',(-1.89697738935017,-0.729525882843488,
-5.44051832736628));
#20235=CARTESIAN_POINT('Ctrl Pts',(-1.97477477835702,-0.56731273106095,
-5.60778248302471));
#20236=CARTESIAN_POINT('Ctrl Pts',(-2.01201382633158,-0.472866430429608,
-5.67453279408918));
#20237=CARTESIAN_POINT('Ctrl Pts',(-2.05457838510613,-0.309311014743861,
-5.74751544509335));
#20238=CARTESIAN_POINT('Ctrl Pts',(-2.06663910190596,-0.248843270470049,
-5.76728897745186));
#20239=CARTESIAN_POINT('Ctrl Pts',(-2.08273777581834,-0.125120393502098,
-5.79343657211952));
#20240=CARTESIAN_POINT('Ctrl Pts',(-2.08688079408944,-0.0628253026847123,
-5.8));
#20241=CARTESIAN_POINT('Ctrl Pts',(-2.08688079408944,-1.27784594234186E-16,
-5.8));
#20242=CARTESIAN_POINT('Ctrl Pts',(-2.08688079408944,0.101093267950359,
-5.8));
#20243=CARTESIAN_POINT('Ctrl Pts',(-2.07606256936626,0.200116780800451,
-5.78306010664896));
#20244=CARTESIAN_POINT('Ctrl Pts',(-2.03456000012612,0.400564730585057,
-5.7138100508258));
#20245=CARTESIAN_POINT('Ctrl Pts',(-2.00198415673787,0.497484683785944,
-5.65792591947954));
#20246=CARTESIAN_POINT('Ctrl Pts',(-1.92762106375197,0.672219726341378,
-5.5102465790806));
#20247=CARTESIAN_POINT('Ctrl Pts',(-1.88521703073068,0.747655625946073,
-5.41535484251111));
#20248=CARTESIAN_POINT('Ctrl Pts',(-1.82963665913355,0.837307075018195,
-5.23892457904446));
#20249=CARTESIAN_POINT('Ctrl Pts',(-1.81154384378188,0.8637489894802,-5.16502186650822));
#20250=CARTESIAN_POINT('Ctrl Pts',(-1.79307858729398,0.890223641153724,
-5.04065959660886));
#20251=CARTESIAN_POINT('Ctrl Pts',(-1.78858372602066,0.896476659347318,
-4.99305285657899));
#20252=CARTESIAN_POINT('Ctrl Pts',(-1.78632454767185,0.899627884673538,
-4.92989708461551));
#20253=CARTESIAN_POINT('Ctrl Pts',(-1.78605710994918,0.9,-4.91494427305051));
#20254=CARTESIAN_POINT('Ctrl Pts',(-1.78605710994918,0.9,-4.9));
#20255=CARTESIAN_POINT('Ctrl Pts',(-1.78605710994918,0.9,-4.9));
#20256=CARTESIAN_POINT('Ctrl Pts',(-1.78605710994918,0.9,-4.87230304065669));
#20257=CARTESIAN_POINT('Ctrl Pts',(-1.7869769405052,0.89872266648372,-4.84463541023445));
#20258=CARTESIAN_POINT('Ctrl Pts',(-1.79231868802101,0.891241854858107,
-4.76381818537326));
#20259=CARTESIAN_POINT('Ctrl Pts',(-1.79916641606906,0.88163807864837,-4.71160904837684));
#20260=CARTESIAN_POINT('Ctrl Pts',(-1.82686643689218,0.841169124752791,
-4.56481378587192));
#20261=CARTESIAN_POINT('Ctrl Pts',(-1.85446030150783,0.799437867210866,
-4.47550957740264));
#20262=CARTESIAN_POINT('Ctrl Pts',(-1.91932437559004,0.684995961096763,
-4.30636138511347));
#20263=CARTESIAN_POINT('Ctrl Pts',(-1.95740679794227,0.608819659462652,
-4.22838203723553));
#20264=CARTESIAN_POINT('Ctrl Pts',(-2.02485323182035,0.430006700487909,
-4.1016362333799));
#20265=CARTESIAN_POINT('Ctrl Pts',(-2.05383693479979,0.327023915525715,
-4.05368786483531));
#20266=CARTESIAN_POINT('Ctrl Pts',(-2.08565111645498,0.116269187541378,
-4.00170605857396));
#20267=CARTESIAN_POINT('Ctrl Pts',(-2.09048597736785,0.013571707734776,
-3.99421211556224));
#20268=CARTESIAN_POINT('Ctrl Pts',(-2.07776710291235,-0.19148403344073,
-4.01460189690483));
#20269=CARTESIAN_POINT('Ctrl Pts',(-2.06053976427926,-0.289671925625125,
-4.04202503782963));
#20270=CARTESIAN_POINT('Ctrl Pts',(-2.00671918893296,-0.488728582767384,
-4.13487097478375));
#20271=CARTESIAN_POINT('Ctrl Pts',(-1.96758297172864,-0.584443608987603,
-4.20573850098139));
#20272=CARTESIAN_POINT('Ctrl Pts',(-1.88908829229803,-0.743279797016489,
-4.37887910454813));
#20273=CARTESIAN_POINT('Ctrl Pts',(-1.84955679967837,-0.806500365822468,
-4.48238860864025));
#20274=CARTESIAN_POINT('Ctrl Pts',(-1.80880106698392,-0.867867222875829,
-4.65409622882474));
#20275=CARTESIAN_POINT('Ctrl Pts',(-1.79841793711201,-0.882619607672314,
-4.71346892553171));
#20276=CARTESIAN_POINT('Ctrl Pts',(-1.78818429336492,-0.897056276598473,
-4.81607218145843));
#20277=CARTESIAN_POINT('Ctrl Pts',(-1.78605710994918,-0.9,-4.85793001834952));
#20278=CARTESIAN_POINT('Ctrl Pts',(-1.78605710994918,-0.9,-4.9));
#20279=CARTESIAN_POINT('Origin',(0.,0.,-5.));
#20280=CARTESIAN_POINT('',(3.74939945665464E-32,3.06161699786838E-16,0.));
#20281=CARTESIAN_POINT('Origin',(0.,0.,-5.));
#20282=CARTESIAN_POINT('Origin',(-5.,0.,-4.9));
#20283=CARTESIAN_POINT('',(-5.,0.9,-4.9));
#20284=CARTESIAN_POINT('Origin',(-2.1,1.212435565298,-27.8));
#20285=CARTESIAN_POINT('',(0.,2.424871130596,-32.2));
#20286=CARTESIAN_POINT('',(0.,2.424871130596,-27.8));
#20287=CARTESIAN_POINT('',(-2.1,1.212435565298,-32.2));
#20288=CARTESIAN_POINT('',(-2.1,1.212435565298,-32.2));
#20289=CARTESIAN_POINT('',(-2.1,1.212435565298,-27.8));
#20290=CARTESIAN_POINT('Origin',(-2.1,-1.212435565298,-27.8));
#20291=CARTESIAN_POINT('',(-2.1,-1.212435565298,-32.2));
#20292=CARTESIAN_POINT('',(-2.1,-1.212435565298,-32.2));
#20293=CARTESIAN_POINT('',(-2.1,-1.212435565298,-27.8));
#20294=CARTESIAN_POINT('Origin',(0.,-2.424871130596,-27.8));
#20295=CARTESIAN_POINT('',(0.,-2.424871130596,-32.2));
#20296=CARTESIAN_POINT('',(0.,-2.424871130596,-32.2));
#20297=CARTESIAN_POINT('',(0.,-2.424871130596,-27.8));
#20298=CARTESIAN_POINT('Origin',(2.1,-1.212435565298,-27.8));
#20299=CARTESIAN_POINT('',(2.1,-1.212435565298,-32.2));
#20300=CARTESIAN_POINT('',(2.1,-1.212435565298,-32.2));
#20301=CARTESIAN_POINT('',(2.1,-1.212435565298,-27.8));
#20302=CARTESIAN_POINT('Origin',(2.1,1.212435565298,-27.8));
#20303=CARTESIAN_POINT('',(2.1,1.212435565298,-32.2));
#20304=CARTESIAN_POINT('',(2.1,1.212435565298,-32.2));
#20305=CARTESIAN_POINT('',(2.1,1.212435565298,-27.8));
#20306=CARTESIAN_POINT('Origin',(0.,2.424871130596,-27.8));
#20307=CARTESIAN_POINT('',(0.,2.424871130596,-32.2));
#20308=CARTESIAN_POINT('Origin',(0.,0.,-32.2));
#20309=CARTESIAN_POINT('',(-1.37153434820004,-0.607366060714214,-32.2));
#20310=CARTESIAN_POINT('',(-1.37391623627015,-0.601217905938934,-32.2001711891269));
#20311=CARTESIAN_POINT('Ctrl Pts',(-1.37153434820004,-0.607366060714214,
-32.2));
#20312=CARTESIAN_POINT('Ctrl Pts',(-1.37242344863637,-0.605358322932482,
-32.2000570630423));
#20313=CARTESIAN_POINT('Ctrl Pts',(-1.37330814048737,-0.603348632866364,
-32.2001141260846));
#20314=CARTESIAN_POINT('Ctrl Pts',(-1.37418841522194,-0.601337009895288,
-32.2001711891269));
#20315=CARTESIAN_POINT('',(0.,-1.5,-32.2));
#20316=CARTESIAN_POINT('Origin',(0.,0.,-32.2));
#20317=CARTESIAN_POINT('',(-7.68260507571859E-6,-1.33950719362872,-32.1999496734209));
#20318=CARTESIAN_POINT('',(0.,-1.5,-32.2));
#20319=CARTESIAN_POINT('',(1.10953170738974,-0.35934403464,-32.1999624944555));
#20320=CARTESIAN_POINT('Ctrl Pts',(1.10946928894836,-0.359327399770989,
-32.2));
#20321=CARTESIAN_POINT('Ctrl Pts',(1.08903134641224,-0.463981924591757,
-32.2));
#20322=CARTESIAN_POINT('Ctrl Pts',(1.05178007571481,-0.581189099461517,
-32.2));
#20323=CARTESIAN_POINT('Ctrl Pts',(0.922701647259221,-0.812733731151359,
-32.2));
#20324=CARTESIAN_POINT('Ctrl Pts',(0.843132342414831,-0.913259848035649,
-32.2));
#20325=CARTESIAN_POINT('Ctrl Pts',(0.650405694031852,-1.09411325950692,
-32.2));
#20326=CARTESIAN_POINT('Ctrl Pts',(0.534709046647493,-1.17218209995489,
-32.2));
#20327=CARTESIAN_POINT('Ctrl Pts',(0.247987289255217,-1.30354237792863,
-32.2));
#20328=CARTESIAN_POINT('Ctrl Pts',(0.101385973706355,-1.32920597320179,
-32.2));
#20329=CARTESIAN_POINT('Ctrl Pts',(-1.53652101508341E-5,-1.33942086081202,
-32.2));
#20330=CARTESIAN_POINT('',(0.489601837133837,1.05872183713734,-32.2));
#20331=CARTESIAN_POINT('Ctrl Pts',(0.489601837133808,1.05872183713728,-32.2));
#20332=CARTESIAN_POINT('Ctrl Pts',(0.51857496980069,1.04522945410028,-32.2));
#20333=CARTESIAN_POINT('Ctrl Pts',(0.546708450841989,1.03069977102869,-32.2));
#20334=CARTESIAN_POINT('Ctrl Pts',(0.574079162507932,1.01517372385618,-32.2));
#20335=CARTESIAN_POINT('Ctrl Pts',(0.601788573860249,0.999455549150711,
-32.2));
#20336=CARTESIAN_POINT('Ctrl Pts',(0.628716837972728,0.982715812039489,
-32.2));
#20337=CARTESIAN_POINT('Ctrl Pts',(0.654924168246827,0.964947264141742,
-32.2));
#20338=CARTESIAN_POINT('Ctrl Pts',(0.671760176005753,0.953532465032388,
-32.2));
#20339=CARTESIAN_POINT('Ctrl Pts',(0.688298993318717,0.941691519760189,
-32.2));
#20340=CARTESIAN_POINT('Ctrl Pts',(0.704548179537464,0.929414759990573,
-32.2));
#20341=CARTESIAN_POINT('Ctrl Pts',(0.740116410445957,0.90254186799368,-32.2));
#20342=CARTESIAN_POINT('Ctrl Pts',(0.774270727515133,0.873591059770721,
-32.2));
#20343=CARTESIAN_POINT('Ctrl Pts',(0.806653680998004,0.842780534610089,
-32.2));
#20344=CARTESIAN_POINT('Ctrl Pts',(0.829132335967985,0.821393382110362,
-32.2));
#20345=CARTESIAN_POINT('Ctrl Pts',(0.850757926025641,0.799111125103228,
-32.2));
#20346=CARTESIAN_POINT('Ctrl Pts',(0.87142065334157,0.776018028800699,-32.2));
#20347=CARTESIAN_POINT('Ctrl Pts',(0.892050009827519,0.752962228435856,
-32.2));
#20348=CARTESIAN_POINT('Ctrl Pts',(0.911717446523677,0.729103354230809,
-32.2));
#20349=CARTESIAN_POINT('Ctrl Pts',(0.930361395902375,0.704476420442543,
-32.2));
#20350=CARTESIAN_POINT('Ctrl Pts',(0.951973732379004,0.675928521678787,
-32.2));
#20351=CARTESIAN_POINT('Ctrl Pts',(0.97221154496313,0.646348165623794,-32.2));
#20352=CARTESIAN_POINT('Ctrl Pts',(0.991051880052035,0.615842514725783,
-32.2));
#20353=CARTESIAN_POINT('Ctrl Pts',(1.00427160782397,0.594437566327873,-32.2));
#20354=CARTESIAN_POINT('Ctrl Pts',(1.01680423321371,0.572574415000461,-32.2));
#20355=CARTESIAN_POINT('Ctrl Pts',(1.02863277515403,0.550296487726837,-32.2));
#20356=CARTESIAN_POINT('Ctrl Pts',(1.05314560211509,0.504128922944566,-32.2));
#20357=CARTESIAN_POINT('Ctrl Pts',(1.07462078700313,0.456193592852453,-32.2));
#20358=CARTESIAN_POINT('Ctrl Pts',(1.09285040392536,0.407053468476931,-32.2));
#20359=CARTESIAN_POINT('Ctrl Pts',(1.11053719474954,0.359376597119088,-32.2));
#20360=CARTESIAN_POINT('Ctrl Pts',(1.12516803341667,0.310577100774157,-32.2));
#20361=CARTESIAN_POINT('Ctrl Pts',(1.13661646586548,0.261120445276902,-32.2));
#20362=CARTESIAN_POINT('Ctrl Pts',(1.14596056480605,0.220754405270782,-32.2));
#20363=CARTESIAN_POINT('Ctrl Pts',(1.15318470938534,0.179951383476785,-32.2));
#20364=CARTESIAN_POINT('Ctrl Pts',(1.15823093245761,0.138967806309482,-32.2));
#20365=CARTESIAN_POINT('Ctrl Pts',(1.16329511589048,0.0978383616658232,
-32.2));
#20366=CARTESIAN_POINT('Ctrl Pts',(1.16616787746435,0.0565354402705209,
-32.2));
#20367=CARTESIAN_POINT('Ctrl Pts',(1.16679746053248,0.015229310284014,-32.2));
#20368=CARTESIAN_POINT('Ctrl Pts',(1.16714856231426,-0.00780602305134579,
-32.2));
#20369=CARTESIAN_POINT('Ctrl Pts',(1.16680161359773,-0.030842710411849,
-32.2));
#20370=CARTESIAN_POINT('Ctrl Pts',(1.16574410749483,-0.0538519246251241,
-32.2));
#20371=CARTESIAN_POINT('Ctrl Pts',(1.1644894176962,-0.0811514610238715,
-32.2));
#20372=CARTESIAN_POINT('Ctrl Pts',(1.16223449940996,-0.108413071862421,
-32.2));
#20373=CARTESIAN_POINT('Ctrl Pts',(1.15900028857009,-0.135588564761368,
-32.2));
#20374=CARTESIAN_POINT('Ctrl Pts',(1.15502516959396,-0.168989546594902,
-32.2));
#20375=CARTESIAN_POINT('Ctrl Pts',(1.14957369981675,-0.20226703966678,-32.2));
#20376=CARTESIAN_POINT('Ctrl Pts',(1.14263928437902,-0.235446334559117,
-32.2));
#20377=CARTESIAN_POINT('Ctrl Pts',(1.13576030868238,-0.268360365344467,
-32.2));
#20378=CARTESIAN_POINT('Ctrl Pts',(1.12742174417963,-0.301178469756348,
-32.2));
#20379=CARTESIAN_POINT('Ctrl Pts',(1.11756964714795,-0.333907056427342,
-32.2));
#20380=CARTESIAN_POINT('Ctrl Pts',(1.1150161570307,-0.342389729948267,-32.2));
#20381=CARTESIAN_POINT('Ctrl Pts',(1.11236075568906,-0.350866262367389,
-32.2));
#20382=CARTESIAN_POINT('Ctrl Pts',(1.10960200800286,-0.359336469688434,
-32.2));
#20383=CARTESIAN_POINT('Ctrl Pts',(-1.37364723137695,-0.601091548606956,
-32.2));
#20384=CARTESIAN_POINT('Ctrl Pts',(-1.41239809287261,-0.485177618605703,
-32.2));
#20385=CARTESIAN_POINT('Ctrl Pts',(-1.43721913529673,-0.364224462906739,
-32.1999999999997));
#20386=CARTESIAN_POINT('Ctrl Pts',(-1.45443046115612,-0.12184967748929,
-32.1999999999997));
#20387=CARTESIAN_POINT('Ctrl Pts',(-1.44774454028095,-0.00120493111834647,
-32.1999999999997));
#20388=CARTESIAN_POINT('Ctrl Pts',(-1.39523776659632,0.289647590051206,
-32.1999999999997));
#20389=CARTESIAN_POINT('Ctrl Pts',(-1.33259337975644,0.457025994986103,
-32.2000000000004));
#20390=CARTESIAN_POINT('Ctrl Pts',(-1.14669279999604,0.757466021501395,
-32.2000000000004));
#20391=CARTESIAN_POINT('Ctrl Pts',(-1.02281858295675,0.889543113224934,
-32.2));
#20392=CARTESIAN_POINT('Ctrl Pts',(-0.739424758019696,1.09285013074389,
-32.2));
#20393=CARTESIAN_POINT('Ctrl Pts',(-0.585285031395165,1.16397131995923,
-32.1999999999995));
#20394=CARTESIAN_POINT('Ctrl Pts',(-0.259459731178378,1.23784226683936,
-32.1999999999995));
#20395=CARTESIAN_POINT('Ctrl Pts',(-0.0956654035339672,1.24352732441668,
-32.2000000000001));
#20396=CARTESIAN_POINT('Ctrl Pts',(0.258061421686738,1.18582051359148,-32.2000000000001));
#20397=CARTESIAN_POINT('Ctrl Pts',(0.39958824699244,1.11415800436119,-32.2));
#20398=CARTESIAN_POINT('Ctrl Pts',(0.489601837133914,1.05872183713747,-32.2));
#20399=CARTESIAN_POINT('Origin',(0.,0.,-32.2));
#20400=CARTESIAN_POINT('',(1.05931837406391E-5,-1.49970471981709,-32.1077344900145));
#20401=CARTESIAN_POINT('Ctrl Pts',(1.9414191012962E-5,-1.49999999987436,
-32.1079045323221));
#20402=CARTESIAN_POINT('Ctrl Pts',(-0.150756927286492,-1.50000195134149,
-32.1157211989316));
#20403=CARTESIAN_POINT('Ctrl Pts',(-0.300662543778459,-1.47727005913098,
-32.1239427369621));
#20404=CARTESIAN_POINT('Ctrl Pts',(-0.580589173772402,-1.39038854903977,
-32.1398124836169));
#20405=CARTESIAN_POINT('Ctrl Pts',(-0.709851208783395,-1.32905217388155,
-32.1472405420935));
#20406=CARTESIAN_POINT('Ctrl Pts',(-0.88710089333139,-1.21160584570517,
-32.1582276281382));
#20407=CARTESIAN_POINT('Ctrl Pts',(-0.942870535510222,-1.16873057217264,
-32.161844427991));
#20408=CARTESIAN_POINT('Ctrl Pts',(-1.05136504230531,-1.07248447363525,
-32.1695118574188));
#20409=CARTESIAN_POINT('Ctrl Pts',(-1.10351027642,-1.01875172871345,-32.1735838961206));
#20410=CARTESIAN_POINT('Ctrl Pts',(-1.24091513632039,-0.854180765807274,
-32.1852578166437));
#20411=CARTESIAN_POINT('Ctrl Pts',(-1.31499941955155,-0.735031403791276,
-32.1927319272353));
#20412=CARTESIAN_POINT('Ctrl Pts',(-1.37153434820004,-0.607366060714214,
-32.2));
#20413=CARTESIAN_POINT('',(0.,-1.5,-32.1078125));
#20414=CARTESIAN_POINT('Ctrl Pts',(-0.9683606883504,0.5860878712161,-30.56360688769));
#20415=CARTESIAN_POINT('Ctrl Pts',(-0.841941231244,0.7949637727945,-30.58077178948));
#20416=CARTESIAN_POINT('Ctrl Pts',(-0.4496074219719,1.12727586262,-30.61510159306));
#20417=CARTESIAN_POINT('Ctrl Pts',(0.3210196062211,1.170506932088,-30.66659629844));
#20418=CARTESIAN_POINT('Ctrl Pts',(0.9617584207716,0.7403170710639,-30.71809100381));
#20419=CARTESIAN_POINT('Ctrl Pts',(1.213652727685,0.01083402249656,-30.76958570919));
#20420=CARTESIAN_POINT('Ctrl Pts',(0.9748232760455,-0.7230402406274,-30.82108041456));
#20421=CARTESIAN_POINT('Ctrl Pts',(0.3418443908816,-1.164564134257,-30.87257511994));
#20422=CARTESIAN_POINT('Ctrl Pts',(-0.4293532065945,-1.135219537988,-30.92406982531));
#20423=CARTESIAN_POINT('Ctrl Pts',(-1.026949913989,-0.6468704059859,-30.97556453069));
#20424=CARTESIAN_POINT('Ctrl Pts',(-1.20931907835,0.1030283602118,-31.02705923606));
#20425=CARTESIAN_POINT('Ctrl Pts',(-0.9027231702267,0.8112695922203,-31.07855394144));
#20426=CARTESIAN_POINT('Ctrl Pts',(-0.2311283984392,1.191489461132,-31.13004864681));
#20427=CARTESIAN_POINT('Ctrl Pts',(0.5339187258583,1.089953332612,-31.18154335219));
#20428=CARTESIAN_POINT('Ctrl Pts',(1.083086014468,0.5477153988916,-31.23303805756));
#20429=CARTESIAN_POINT('Ctrl Pts',(1.194328167088,-0.2159807914049,-31.28453276294));
#20430=CARTESIAN_POINT('Ctrl Pts',(0.8226665446893,-0.8923492753407,-31.33602746831));
#20431=CARTESIAN_POINT('Ctrl Pts',(0.1183754231753,-1.207913379402,-31.38752217369));
#20432=CARTESIAN_POINT('Ctrl Pts',(-0.6337785389668,-1.035080787425,-31.43901687906));
#20433=CARTESIAN_POINT('Ctrl Pts',(-1.129676258131,-0.4437330557542,-31.49051158444));
#20434=CARTESIAN_POINT('Ctrl Pts',(-1.168810966393,0.3270296588359,-31.54200628981));
#20435=CARTESIAN_POINT('Ctrl Pts',(-0.7353592922662,0.9655641793129,-31.59350099519));
#20436=CARTESIAN_POINT('Ctrl Pts',(-0.004579138184,1.213691272131,-31.64499570056));
#20437=CARTESIAN_POINT('Ctrl Pts',(0.7280525020971,0.9710854892931,-31.69649040594));
#20438=CARTESIAN_POINT('Ctrl Pts',(1.16631002676,0.335839839429,-31.74798511131));
#20439=CARTESIAN_POINT('Ctrl Pts',(1.132992364504,-0.4351962200625,-31.79947981669));
#20440=CARTESIAN_POINT('Ctrl Pts',(0.641570930501,-1.030269050578,-31.85097452206));
#20441=CARTESIAN_POINT('Ctrl Pts',(-0.1092576130587,-1.208772097777,-31.90246922744));
#20442=CARTESIAN_POINT('Ctrl Pts',(-0.8159093239228,-0.8985319049552,-31.95396393281));
#20443=CARTESIAN_POINT('Ctrl Pts',(-1.192665944352,-0.2249850320436,-32.00545863819));
#20444=CARTESIAN_POINT('Ctrl Pts',(-1.087182459866,0.539521014043,-32.05695334356));
#20445=CARTESIAN_POINT('Ctrl Pts',(-0.5421489359955,1.085916477839,-32.10844804894));
#20446=CARTESIAN_POINT('Ctrl Pts',(0.2222093980149,1.193113862031,-32.15994275432));
#20447=CARTESIAN_POINT('Ctrl Pts',(0.6715924913568,0.9432899673364,-32.1942725579));
#20448=CARTESIAN_POINT('Ctrl Pts',(0.83615698899,0.762930472122,-32.21143745969));
#20449=CARTESIAN_POINT('Ctrl Pts',(-1.0833316035,0.6556725411871,-30.64119627189));
#20450=CARTESIAN_POINT('Ctrl Pts',(-0.9419026970726,0.8893477286577,-30.65836117369));
#20451=CARTESIAN_POINT('Ctrl Pts',(-0.5029881275127,1.261114358038,-30.69269097727));
#20452=CARTESIAN_POINT('Ctrl Pts',(0.3591334189276,1.309478138571,-30.74418568264));
#20453=CARTESIAN_POINT('Ctrl Pts',(1.075945466073,0.8282129678975,-30.79568038802));
#20454=CARTESIAN_POINT('Ctrl Pts',(1.35774652089,0.01212031746512,-30.84717509339));
#20455=CARTESIAN_POINT('Ctrl Pts',(1.090561477218,-0.8088849048676,-30.89866979877));
#20456=CARTESIAN_POINT('Ctrl Pts',(0.382430675446,-1.302829767999,-30.95016450414));
#20457=CARTESIAN_POINT('Ctrl Pts',(-0.4803291824663,-1.27000116507,-31.00165920952));
#20458=CARTESIAN_POINT('Ctrl Pts',(-1.148876973652,-0.7236716262895,-31.05315391489));
#20459=CARTESIAN_POINT('Ctrl Pts',(-1.352898348779,0.1152606461796,-31.10464862027));
#20460=CARTESIAN_POINT('Ctrl Pts',(-1.009901115652,0.907589495096,-31.15614332565));
#20461=CARTESIAN_POINT('Ctrl Pts',(-0.2585696647001,1.332951868048,-31.20763803102));
#20462=CARTESIAN_POINT('Ctrl Pts',(0.5973094905453,1.219360622301,-31.2591327364));
#20463=CARTESIAN_POINT('Ctrl Pts',(1.211677965553,0.6127442062457,-31.31062744177));
#20464=CARTESIAN_POINT('Ctrl Pts',(1.336127606089,-0.2416236221613,-31.36212214715));
#20465=CARTESIAN_POINT('Ctrl Pts',(0.9203395777271,-0.9982955555368,-31.41361685252));
#20466=CARTESIAN_POINT('Ctrl Pts',(0.132429825525,-1.351325754896,-31.4651115579));
#20467=CARTESIAN_POINT('Ctrl Pts',(-0.7090253963658,-1.157973204286,-31.51660626327));
#20468=CARTESIAN_POINT('Ctrl Pts',(-1.26379974619,-0.4964163132592,-31.56810096865));
#20469=CARTESIAN_POINT('Ctrl Pts',(-1.307580815334,0.3658570292669,-31.61959567402));
#20470=CARTESIAN_POINT('Ctrl Pts',(-0.8226665650754,1.080203072307,-31.6710903794));
#20471=CARTESIAN_POINT('Ctrl Pts',(-0.005122807205206,1.357789641617,-31.72258508477));
#20472=CARTESIAN_POINT('Ctrl Pts',(0.8144922589459,1.086379912885,-31.77407979015));
#20473=CARTESIAN_POINT('Ctrl Pts',(1.304782945723,0.3757132194075,-31.82557449552));
#20474=CARTESIAN_POINT('Ctrl Pts',(1.267509565142,-0.4868659215406,-31.8770692009));
#20475=CARTESIAN_POINT('Ctrl Pts',(0.7177429580321,-1.15259018259,-31.92856390627));
#20476=CARTESIAN_POINT('Ctrl Pts',(-0.1222294818174,-1.352286426643,-31.98005861165));
#20477=CARTESIAN_POINT('Ctrl Pts',(-0.9127800899286,-1.005212232489,-32.03155331702));
#20478=CARTESIAN_POINT('Ctrl Pts',(-1.334268032024,-0.2516969125858,-32.0830480224));
#20479=CARTESIAN_POINT('Ctrl Pts',(-1.216260771128,0.6035769236572,-32.13454272777));
#20480=CARTESIAN_POINT('Ctrl Pts',(-0.6065168518646,1.214844482388,-32.18603743315));
#20481=CARTESIAN_POINT('Ctrl Pts',(0.2485917348362,1.33476912979,-32.23753213852));
#20482=CARTESIAN_POINT('Ctrl Pts',(0.7513288997713,1.055284301783,-32.27186194211));
#20483=CARTESIAN_POINT('Ctrl Pts',(0.9354317069637,0.8535111985296,-32.2890268439));
#20484=CARTESIAN_POINT('Ctrl Pts',(-1.198302518649,0.7252572111581,-30.7187856561));
#20485=CARTESIAN_POINT('Ctrl Pts',(-1.041864162901,0.9837316845208,-30.73595055789));
#20486=CARTESIAN_POINT('Ctrl Pts',(-0.5563688330535,1.394952853457,-30.77028036148));
#20487=CARTESIAN_POINT('Ctrl Pts',(0.3972472316341,1.448449345054,-30.82177506685));
#20488=CARTESIAN_POINT('Ctrl Pts',(1.190132511375,0.9161088647312,-30.87326977223));
#20489=CARTESIAN_POINT('Ctrl Pts',(1.501840314096,0.01340661243369,-30.9247644776));
#20490=CARTESIAN_POINT('Ctrl Pts',(1.206299678391,-0.8947295691077,-30.97625918298));
#20491=CARTESIAN_POINT('Ctrl Pts',(0.4230169600104,-1.441095401742,-31.02775388835));
#20492=CARTESIAN_POINT('Ctrl Pts',(-0.5313051583381,-1.404782792152,-31.07924859373));
#20493=CARTESIAN_POINT('Ctrl Pts',(-1.270804033315,-0.800472846593,-31.1307432991));
#20494=CARTESIAN_POINT('Ctrl Pts',(-1.496477619208,0.1274929321474,-31.18223800448));
#20495=CARTESIAN_POINT('Ctrl Pts',(-1.117079061076,1.003909397972,-31.23373270985));
#20496=CARTESIAN_POINT('Ctrl Pts',(-0.2860109309609,1.474414274964,-31.28522741523));
#20497=CARTESIAN_POINT('Ctrl Pts',(0.6607002552323,1.34876791199,-31.3367221206));
#20498=CARTESIAN_POINT('Ctrl Pts',(1.340269916638,0.6777730135999,-31.38821682598));
#20499=CARTESIAN_POINT('Ctrl Pts',(1.47792704509,-0.2672664529177,-31.43971153135));
#20500=CARTESIAN_POINT('Ctrl Pts',(1.018012610765,-1.104241835733,-31.49120623673));
#20501=CARTESIAN_POINT('Ctrl Pts',(0.1464842278746,-1.494738130389,-31.5427009421));
#20502=CARTESIAN_POINT('Ctrl Pts',(-0.7842722537648,-1.280865621146,-31.59419564748));
#20503=CARTESIAN_POINT('Ctrl Pts',(-1.397923234248,-0.5490995707643,-31.64569035285));
#20504=CARTESIAN_POINT('Ctrl Pts',(-1.446350664275,0.4046843996979,-31.69718505823));
#20505=CARTESIAN_POINT('Ctrl Pts',(-0.9099738378846,1.1948419653,-31.7486797636));
#20506=CARTESIAN_POINT('Ctrl Pts',(-0.005666476226419,1.501888011103,-31.80017446898));
#20507=CARTESIAN_POINT('Ctrl Pts',(0.9009320157947,1.201674336477,-31.85166917435));
#20508=CARTESIAN_POINT('Ctrl Pts',(1.443255864685,0.415586599386,-31.90316387973));
#20509=CARTESIAN_POINT('Ctrl Pts',(1.40202676578,-0.5385356230187,-31.95465858511));
#20510=CARTESIAN_POINT('Ctrl Pts',(0.7939149855631,-1.274911314603,-32.00615329048));
#20511=CARTESIAN_POINT('Ctrl Pts',(-0.1352013505761,-1.495800755509,-32.05764799586));
#20512=CARTESIAN_POINT('Ctrl Pts',(-1.009650855934,-1.111892560022,-32.10914270123));
#20513=CARTESIAN_POINT('Ctrl Pts',(-1.475870119695,-0.2784087931281,-32.16063740661));
#20514=CARTESIAN_POINT('Ctrl Pts',(-1.345339082391,0.6676328332714,-32.21213211198));
#20515=CARTESIAN_POINT('Ctrl Pts',(-0.6708847677338,1.343772486938,-32.26362681736));
#20516=CARTESIAN_POINT('Ctrl Pts',(0.2749740716576,1.476424397549,-32.31512152273));
#20517=CARTESIAN_POINT('Ctrl Pts',(0.8310653081857,1.16727863623,-32.34945132631));
#20518=CARTESIAN_POINT('Ctrl Pts',(1.034706424937,0.9440919249371,-32.36661622811));
#20519=CARTESIAN_POINT('Ctrl Pts',(-1.313273433799,0.794841881129,-30.79637504031));
#20520=CARTESIAN_POINT('Ctrl Pts',(-1.14182562873,1.078115640384,-30.8135399421));
#20521=CARTESIAN_POINT('Ctrl Pts',(-0.6097495385943,1.528791348876,-30.84786974568));
#20522=CARTESIAN_POINT('Ctrl Pts',(0.4353610443407,1.587420551537,-30.89936445106));
#20523=CARTESIAN_POINT('Ctrl Pts',(1.304319556676,1.004004761565,-30.95085915644));
#20524=CARTESIAN_POINT('Ctrl Pts',(1.645934107302,0.01469290740225,-31.00235386181));
#20525=CARTESIAN_POINT('Ctrl Pts',(1.322037879563,-0.9805742333479,-31.05384856719));
#20526=CARTESIAN_POINT('Ctrl Pts',(0.4636032445749,-1.579361035484,-31.10534327256));
#20527=CARTESIAN_POINT('Ctrl Pts',(-0.5822811342099,-1.539564419234,-31.15683797794));
#20528=CARTESIAN_POINT('Ctrl Pts',(-1.392731092978,-0.8772740668966,-31.20833268331));
#20529=CARTESIAN_POINT('Ctrl Pts',(-1.640056889637,0.1397252181152,-31.25982738869));
#20530=CARTESIAN_POINT('Ctrl Pts',(-1.224257006501,1.100229300847,-31.31132209406));
#20531=CARTESIAN_POINT('Ctrl Pts',(-0.3134521972218,1.615876681881,-31.36281679944));
#20532=CARTESIAN_POINT('Ctrl Pts',(0.7240910199193,1.478175201679,-31.41431150481));
#20533=CARTESIAN_POINT('Ctrl Pts',(1.468861867722,0.742801820954,-31.46580621019));
#20534=CARTESIAN_POINT('Ctrl Pts',(1.619726484091,-0.2929092836741,-31.51730091556));
#20535=CARTESIAN_POINT('Ctrl Pts',(1.115685643803,-1.210188115929,-31.56879562094));
#20536=CARTESIAN_POINT('Ctrl Pts',(0.1605386302243,-1.638150505883,-31.62029032631));
#20537=CARTESIAN_POINT('Ctrl Pts',(-0.8595191111638,-1.403758038006,-31.67178503169));
#20538=CARTESIAN_POINT('Ctrl Pts',(-1.532046722306,-0.6017828282693,-31.72327973706));
#20539=CARTESIAN_POINT('Ctrl Pts',(-1.585120513216,0.4435117701289,-31.77477444244));
#20540=CARTESIAN_POINT('Ctrl Pts',(-0.9972811106938,1.309480858294,-31.82626914781));
#20541=CARTESIAN_POINT('Ctrl Pts',(-0.006210145247626,1.645986380589,-31.87776385319));
#20542=CARTESIAN_POINT('Ctrl Pts',(0.9873717726436,1.316968760069,-31.92925855856));
#20543=CARTESIAN_POINT('Ctrl Pts',(1.581728783648,0.4554599793645,-31.98075326394));
#20544=CARTESIAN_POINT('Ctrl Pts',(1.536543966417,-0.5902053244968,-32.03224796931));
#20545=CARTESIAN_POINT('Ctrl Pts',(0.8700870130942,-1.397232446615,-32.08374267469));
#20546=CARTESIAN_POINT('Ctrl Pts',(-0.1481732193349,-1.639315084374,-32.13523738006));
#20547=CARTESIAN_POINT('Ctrl Pts',(-1.10652162194,-1.218572887555,-32.18673208544));
#20548=CARTESIAN_POINT('Ctrl Pts',(-1.617472207367,-0.3051206736703,-32.23822679081));
#20549=CARTESIAN_POINT('Ctrl Pts',(-1.474417393653,0.7316887428856,-32.28972149619));
#20550=CARTESIAN_POINT('Ctrl Pts',(-0.7352526836029,1.472700491487,-32.34121620156));
#20551=CARTESIAN_POINT('Ctrl Pts',(0.3013564084789,1.618079665308,-32.39271090694));
#20552=CARTESIAN_POINT('Ctrl Pts',(0.9108017166002,1.279272970676,-32.42704071052));
#20553=CARTESIAN_POINT('Ctrl Pts',(1.133981142911,1.034672651345,-32.44420561231));
#20554=CARTESIAN_POINT('',(-0.685937500187104,0.944111968542343,-30.6155198486503));
#20555=CARTESIAN_POINT('Ctrl Pts',(-0.685549818356495,0.943589307941825,
-30.6154432565738));
#20556=CARTESIAN_POINT('Ctrl Pts',(-0.58064605296268,1.02007511987387,-30.6243229170041));
#20557=CARTESIAN_POINT('Ctrl Pts',(-0.444206516756635,1.09392715892444,
-30.6348232653003));
#20558=CARTESIAN_POINT('Ctrl Pts',(-0.123013026528223,1.16966346430087,
-30.6572180841587));
#20559=CARTESIAN_POINT('Ctrl Pts',(0.0323543525080591,1.1755099489028,-30.6674551876461));
#20560=CARTESIAN_POINT('Ctrl Pts',(0.272129692413745,1.13820198274907,-30.6841062976065));
#20561=CARTESIAN_POINT('Ctrl Pts',(0.35976297016591,1.11401115078793,-30.6904574701318));
#20562=CARTESIAN_POINT('Ctrl Pts',(0.515514067421646,1.04955883562299,-30.7020015367485));
#20563=CARTESIAN_POINT('Ctrl Pts',(0.583848005518145,1.01277911064057,-30.7071896615724));
#20564=CARTESIAN_POINT('Ctrl Pts',(0.724546181506395,0.918370978969335,
-30.7185554543531));
#20565=CARTESIAN_POINT('Ctrl Pts',(0.795191272615342,0.858032542126043,
-30.7247396075133));
#20566=CARTESIAN_POINT('Ctrl Pts',(0.962172388622911,0.677781105774433,
-30.7415978089187));
#20567=CARTESIAN_POINT('Ctrl Pts',(1.04182541894227,0.547667974612751,-30.7522459281879));
#20568=CARTESIAN_POINT('Ctrl Pts',(1.12323761388946,0.324738122282939,-30.7680872244194));
#20569=CARTESIAN_POINT('Ctrl Pts',(1.14355889053653,0.243126408867936,-30.7736158882269));
#20570=CARTESIAN_POINT('Ctrl Pts',(1.16583991182123,0.0841465040768233,
-30.7844711483562));
#20571=CARTESIAN_POINT('Ctrl Pts',(1.16913809492736,0.00689646112748725,
-30.7898296388345));
#20572=CARTESIAN_POINT('Ctrl Pts',(1.16222537935487,-0.113540683276614,
-30.7983737162774));
#20573=CARTESIAN_POINT('Ctrl Pts',(1.15723001531888,-0.157076089779638,
-30.8014697176085));
#20574=CARTESIAN_POINT('Ctrl Pts',(1.13490702072137,-0.284498729207274,
-30.8103909766174));
#20575=CARTESIAN_POINT('Ctrl Pts',(1.11060620210311,-0.36691443612988,-30.8160317748216));
#20576=CARTESIAN_POINT('Ctrl Pts',(1.04510048542586,-0.524311586158876,
-30.827298666073));
#20577=CARTESIAN_POINT('Ctrl Pts',(1.00394780872658,-0.599371546138324,
-30.8329348435321));
#20578=CARTESIAN_POINT('Ctrl Pts',(0.921020285080622,-0.718350217423981,
-30.8429575993004));
#20579=CARTESIAN_POINT('Ctrl Pts',(0.882990259693012,-0.76494679049744,
-30.8472534440817));
#20580=CARTESIAN_POINT('Ctrl Pts',(0.815751820700548,-0.835292827709003,
-30.8541625266585));
#20581=CARTESIAN_POINT('Ctrl Pts',(0.788600249269866,-0.861057780772529,
-30.8567974562499));
#20582=CARTESIAN_POINT('Ctrl Pts',(0.704840482900919,-0.932860902847456,
-30.8643865651111));
#20583=CARTESIAN_POINT('Ctrl Pts',(0.644987568932664,-0.974856777009102,
-30.8691842871257));
#20584=CARTESIAN_POINT('Ctrl Pts',(0.516425892376748,-1.04837375477001,
-30.8789144838574));
#20585=CARTESIAN_POINT('Ctrl Pts',(0.4474710934552,-1.07950036803969,-30.8838515782429));
#20586=CARTESIAN_POINT('Ctrl Pts',(0.322697231458926,-1.12218677030221,
-30.8928435994936));
#20587=CARTESIAN_POINT('Ctrl Pts',(0.267843862426517,-1.13669200069658,
-30.896846619438));
#20588=CARTESIAN_POINT('Ctrl Pts',(0.168539599695823,-1.15537506229575,
-30.9040510091863));
#20589=CARTESIAN_POINT('Ctrl Pts',(0.12437129358316,-1.16109940910304,-30.9072314578863));
#20590=CARTESIAN_POINT('Ctrl Pts',(0.04002917364263,-1.16701286980662,-30.9131523317177));
#20591=CARTESIAN_POINT('Ctrl Pts',(0.00014785501451689,-1.16766543747708,
-30.9158750267731));
#20592=CARTESIAN_POINT('Ctrl Pts',(-0.120399774363236,-1.16329491837156,
-30.9239498325746));
#20593=CARTESIAN_POINT('Ctrl Pts',(-0.200704815239112,-1.151826505131,-30.9291490667603));
#20594=CARTESIAN_POINT('Ctrl Pts',(-0.315214160338411,-1.12341563756021,
-30.9369298719994));
#20595=CARTESIAN_POINT('Ctrl Pts',(-0.350995565090333,-1.11273069881691,
-30.9394161098036));
#20596=CARTESIAN_POINT('Ctrl Pts',(-0.457319408159109,-1.07547579278067,
-30.9470914368855));
#20597=CARTESIAN_POINT('Ctrl Pts',(-0.526092532709015,-1.043814098234,-30.9525024051635));
#20598=CARTESIAN_POINT('Ctrl Pts',(-0.637601397105962,-0.978724537033635,
-30.9617031731051));
#20599=CARTESIAN_POINT('Ctrl Pts',(-0.682226149753855,-0.948353027567811,
-30.9655138607647));
#20600=CARTESIAN_POINT('Ctrl Pts',(-0.776257227460013,-0.873838007781977,
-30.9736876405209));
#20601=CARTESIAN_POINT('Ctrl Pts',(-0.824357288478918,-0.828279102352816,
-30.9779858533615));
#20602=CARTESIAN_POINT('Ctrl Pts',(-0.910617501933913,-0.731559492611122,
-30.9864321791417));
#20603=CARTESIAN_POINT('Ctrl Pts',(-0.949079289481939,-0.680674445423622,
-30.9905825954745));
#20604=CARTESIAN_POINT('Ctrl Pts',(-1.02513338266168,-0.56138353942896,
-31.000216709631));
#20605=CARTESIAN_POINT('Ctrl Pts',(-1.06060237636569,-0.49155930001184,
-31.0058072822228));
#20606=CARTESIAN_POINT('Ctrl Pts',(-1.10962744691463,-0.365287132932502,
-31.0154453787039));
#20607=CARTESIAN_POINT('Ctrl Pts',(-1.12649192979211,-0.310091614787038,
-31.0195135341267));
#20608=CARTESIAN_POINT('Ctrl Pts',(-1.15268125864006,-0.192731992657596,
-31.0276959783734));
#20609=CARTESIAN_POINT('Ctrl Pts',(-1.16115789218137,-0.13051886757346,
-31.0317727346732));
#20610=CARTESIAN_POINT('Ctrl Pts',(-1.16791178975008,-0.00868033034464753,
-31.0397150790911));
#20611=CARTESIAN_POINT('Ctrl Pts',(-1.1666680633032,0.0509752084799933,
-31.0435873391708));
#20612=CARTESIAN_POINT('Ctrl Pts',(-1.15467348304469,0.17617947896303,-31.0521400991318));
#20613=CARTESIAN_POINT('Ctrl Pts',(-1.14284908742083,0.241656664267984,
-31.0568344967498));
#20614=CARTESIAN_POINT('Ctrl Pts',(-1.10763145439615,0.372687281057628,
-31.0664668348878));
#20615=CARTESIAN_POINT('Ctrl Pts',(-1.08370537416884,0.438139495945055,
-31.0714053450789));
#20616=CARTESIAN_POINT('Ctrl Pts',(-1.02026614664799,0.572107606135475,
-31.0815641621441));
#20617=CARTESIAN_POINT('Ctrl Pts',(-0.979287244981931,0.639164520306697,
-31.0866104510614));
#20618=CARTESIAN_POINT('Ctrl Pts',(-0.910536559022417,0.729969026199407,
-31.0940487006932));
#20619=CARTESIAN_POINT('Ctrl Pts',(-0.887588763253689,0.757550902676565,
-31.0964059553973));
#20620=CARTESIAN_POINT('Ctrl Pts',(-0.79318341488161,0.861115385835129,
-31.105836469407));
#20621=CARTESIAN_POINT('Ctrl Pts',(-0.712708892211407,0.929007678350079,
-31.1133048282032));
#20622=CARTESIAN_POINT('Ctrl Pts',(-0.586676199099358,1.00947261785909,
-31.1238366894391));
#20623=CARTESIAN_POINT('Ctrl Pts',(-0.54711709638151,1.03161773821077,-31.1270017225964));
#20624=CARTESIAN_POINT('Ctrl Pts',(-0.447880028777928,1.07963910147511,
-31.1345515613862));
#20625=CARTESIAN_POINT('Ctrl Pts',(-0.387510472693664,1.10260994906124,
-31.1387701787857));
#20626=CARTESIAN_POINT('Ctrl Pts',(-0.284851937819151,1.13211115662808,
-31.1457492890684));
#20627=CARTESIAN_POINT('Ctrl Pts',(-0.243599465079629,1.14155657530597,
-31.1485177707169));
#20628=CARTESIAN_POINT('Ctrl Pts',(-0.128297940424894,1.16153184398187,
-31.1563826813405));
#20629=CARTESIAN_POINT('Ctrl Pts',(-0.05339768760864,1.16731338199176,-31.1616009318968));
#20630=CARTESIAN_POINT('Ctrl Pts',(0.0892765697898679,1.1649149779081,-31.1716159041541));
#20631=CARTESIAN_POINT('Ctrl Pts',(0.15714162457393,1.15795513700009,-31.1764096565917));
#20632=CARTESIAN_POINT('Ctrl Pts',(0.278664991070919,1.13454883807076,-31.1849605518862));
#20633=CARTESIAN_POINT('Ctrl Pts',(0.332653037305334,1.12002949667963,-31.1887346689173));
#20634=CARTESIAN_POINT('Ctrl Pts',(0.433816672891627,1.0844438029925,-31.1958147743426));
#20635=CARTESIAN_POINT('Ctrl Pts',(0.480820518649546,1.06424943532574,-31.1991383315904));
#20636=CARTESIAN_POINT('Ctrl Pts',(0.64177924230017,0.982275042229206,-31.2112090255195));
#20637=CARTESIAN_POINT('Ctrl Pts',(0.747625313053594,0.904251732343868,
-31.2203661560253));
#20638=CARTESIAN_POINT('Ctrl Pts',(0.880907974589085,0.767383596728147,
-31.2336520510528));
#20639=CARTESIAN_POINT('Ctrl Pts',(0.920355842015236,0.719964895099076,
-31.2378964628582));
#20640=CARTESIAN_POINT('Ctrl Pts',(0.994030870573145,0.615094816078788,
-31.2465511819434));
#20641=CARTESIAN_POINT('Ctrl Pts',(1.02719182235098,0.557521893428536,-31.2508737135115));
#20642=CARTESIAN_POINT('Ctrl Pts',(1.11651848045971,0.36662271234126,-31.2650086372261));
#20643=CARTESIAN_POINT('Ctrl Pts',(1.15347382627016,0.22401192173484,-31.2751414931434));
#20644=CARTESIAN_POINT('Ctrl Pts',(1.1744576386023,-0.0697605175983266,
-31.2954708383108));
#20645=CARTESIAN_POINT('Ctrl Pts',(1.15618399361287,-0.217343368572523,
-31.3051565938156));
#20646=CARTESIAN_POINT('Ctrl Pts',(1.06334090087441,-0.501175404200165,
-31.3254700203755));
#20647=CARTESIAN_POINT('Ctrl Pts',(0.990072860789148,-0.634244960097407,
-31.3357877022529));
#20648=CARTESIAN_POINT('Ctrl Pts',(0.779939960671839,-0.886826667173546,
-31.3582916167791));
#20649=CARTESIAN_POINT('Ctrl Pts',(0.651195811249931,-0.976393206170076,
-31.3686325822348));
#20650=CARTESIAN_POINT('Ctrl Pts',(0.40465076484607,-1.10348922038188,-31.3874884713758));
#20651=CARTESIAN_POINT('Ctrl Pts',(0.26067210257786,-1.14683252718141,-31.3975848541239));
#20652=CARTESIAN_POINT('Ctrl Pts',(0.0414129321920925,-1.1685833647203,
-31.4127775461669));
#20653=CARTESIAN_POINT('Ctrl Pts',(-0.0311611824591641,-1.16863904701939,
-31.4177144778021));
#20654=CARTESIAN_POINT('Ctrl Pts',(-0.250957175467129,-1.14849060721418,
-31.4326611289385));
#20655=CARTESIAN_POINT('Ctrl Pts',(-0.396566537627489,-1.10667316158768,
-31.44261757239));
#20656=CARTESIAN_POINT('Ctrl Pts',(-0.638350257118472,-0.98452433640704,
-31.461266651544));
#20657=CARTESIAN_POINT('Ctrl Pts',(-0.736541623239782,-0.913407391716465,
-31.4696968846861));
#20658=CARTESIAN_POINT('Ctrl Pts',(-0.923384755992755,-0.726303779689699,
-31.4875096033724));
#20659=CARTESIAN_POINT('Ctrl Pts',(-1.0055723746581,-0.607329676628576,
-31.4968989787272));
#20660=CARTESIAN_POINT('Ctrl Pts',(-1.0936762524601,-0.412696282653138,
-31.5116737635136));
#20661=CARTESIAN_POINT('Ctrl Pts',(-1.11727838553113,-0.344659613610039,
-31.5168039971177));
#20662=CARTESIAN_POINT('Ctrl Pts',(-1.14616299763878,-0.225186641674113,
-31.5253254635316));
#20663=CARTESIAN_POINT('Ctrl Pts',(-1.15476615560226,-0.174808565363235,
-31.5287817978504));
#20664=CARTESIAN_POINT('Ctrl Pts',(-1.16753840461434,-0.0518871225375712,
-31.5370652043289));
#20665=CARTESIAN_POINT('Ctrl Pts',(-1.16829471715105,0.0210179048571228,
-31.5418549401139));
#20666=CARTESIAN_POINT('Ctrl Pts',(-1.15703286837474,0.160510799516341,
-31.5511950587481));
#20667=CARTESIAN_POINT('Ctrl Pts',(-1.14592336273605,0.227225796083613,
-31.5557428617876));
#20668=CARTESIAN_POINT('Ctrl Pts',(-1.11662488052543,0.3416742850202,-31.5639576111054));
#20669=CARTESIAN_POINT('Ctrl Pts',(-1.10084925783999,0.390046111141884,
-31.567582314457));
#20670=CARTESIAN_POINT('Ctrl Pts',(-1.06334533384066,0.483414957899083,
-31.5747012168093));
#20671=CARTESIAN_POINT('Ctrl Pts',(-1.04188770919863,0.528059829950944,
-31.5781420352983));
#20672=CARTESIAN_POINT('Ctrl Pts',(-0.991356486728722,0.617571049953205,
-31.5851109376138));
#20673=CARTESIAN_POINT('Ctrl Pts',(-0.96211461432135,0.661875222634075,
-31.5886220053224));
#20674=CARTESIAN_POINT('Ctrl Pts',(-0.875015979693796,0.776286059444753,
-31.5981155690734));
#20675=CARTESIAN_POINT('Ctrl Pts',(-0.811616460796327,0.842239001467981,
-31.6040805899385));
#20676=CARTESIAN_POINT('Ctrl Pts',(-0.707260818464706,0.928555454565463,
-31.6133843286188));
#20677=CARTESIAN_POINT('Ctrl Pts',(-0.671285275966235,0.955051098604024,
-31.6165309479633));
#20678=CARTESIAN_POINT('Ctrl Pts',(-0.576842243397548,1.01658449168296,
-31.6245495281119));
#20679=CARTESIAN_POINT('Ctrl Pts',(-0.516407878498177,1.04883047882692,
-31.6294318125191));
#20680=CARTESIAN_POINT('Ctrl Pts',(-0.386933712951129,1.1031863842945,-31.6390086889994));
#20681=CARTESIAN_POINT('Ctrl Pts',(-0.318197534791427,1.12464209428096,
-31.6437060028805));
#20682=CARTESIAN_POINT('Ctrl Pts',(-0.176551057827588,1.15509542084064,
-31.6532098441827));
#20683=CARTESIAN_POINT('Ctrl Pts',(-0.103562879627239,1.16383625984169,
-31.6580222417704));
#20684=CARTESIAN_POINT('Ctrl Pts',(0.00757975185125543,1.16688101758023,
-31.6656505014464));
#20685=CARTESIAN_POINT('Ctrl Pts',(0.0456383690066451,1.16610227706485,
-31.6683241575286));
#20686=CARTESIAN_POINT('Ctrl Pts',(0.166807315161587,1.15774406385772,-31.6769512638621));
#20687=CARTESIAN_POINT('Ctrl Pts',(0.249701555193096,1.1431299277067,-31.6829994302105));
#20688=CARTESIAN_POINT('Ctrl Pts',(0.365039122436339,1.10896345331728,-31.6911740597271));
#20689=CARTESIAN_POINT('Ctrl Pts',(0.399178429731245,1.09703892879711,-31.6935755172703));
#20690=CARTESIAN_POINT('Ctrl Pts',(0.507266581111613,1.05351244564662,-31.701245116546));
#20691=CARTESIAN_POINT('Ctrl Pts',(0.578724955642715,1.01570900434554,-31.7064229068078));
#20692=CARTESIAN_POINT('Ctrl Pts',(0.679519651351591,0.94862017495968,-31.7145405625731));
#20693=CARTESIAN_POINT('Ctrl Pts',(0.712237917566348,0.92434310659105,-31.7173323014913));
#20694=CARTESIAN_POINT('Ctrl Pts',(0.782828297502978,0.866126524336308,
-31.7237497581707));
#20695=CARTESIAN_POINT('Ctrl Pts',(0.819965848295058,0.831275602275542,
-31.7273928733489));
#20696=CARTESIAN_POINT('Ctrl Pts',(0.889879014567416,0.75648662679121,-31.7346851589437));
#20697=CARTESIAN_POINT('Ctrl Pts',(0.922584047073668,0.716479193628441,
-31.738332751243));
#20698=CARTESIAN_POINT('Ctrl Pts',(0.988121125294871,0.623950581583141,
-31.7460816214656));
#20699=CARTESIAN_POINT('Ctrl Pts',(1.01962351039126,0.570598821904264,-31.7501180542607));
#20700=CARTESIAN_POINT('Ctrl Pts',(1.07676956878579,0.453589499983911,-31.7586015879158));
#20701=CARTESIAN_POINT('Ctrl Pts',(1.10141647309642,0.389406426700824,-31.7630519669856));
#20702=CARTESIAN_POINT('Ctrl Pts',(1.13884447385869,0.259660537621559,-31.7722465089549));
#20703=CARTESIAN_POINT('Ctrl Pts',(1.15194897150424,0.194139742766789,-31.7769860960563));
#20704=CARTESIAN_POINT('Ctrl Pts',(1.1672103135223,0.0594154514047917,-31.786637421575));
#20705=CARTESIAN_POINT('Ctrl Pts',(1.16894378165254,-0.00986571973121408,
-31.7915476746924));
#20706=CARTESIAN_POINT('Ctrl Pts',(1.1604583412024,-0.136354678584791,-31.8001907605822));
#20707=CARTESIAN_POINT('Ctrl Pts',(1.15213820383205,-0.193450951917024,
-31.8039493203448));
#20708=CARTESIAN_POINT('Ctrl Pts',(1.12539423050888,-0.313872074658607,
-31.8119794187064));
#20709=CARTESIAN_POINT('Ctrl Pts',(1.10563389783109,-0.377002239706556,
-31.816262647434));
#20710=CARTESIAN_POINT('Ctrl Pts',(1.06699224135733,-0.472075357193685,
-31.8232522134308));
#20711=CARTESIAN_POINT('Ctrl Pts',(1.05159611665665,-0.505451744236681,
-31.8258065160752));
#20712=CARTESIAN_POINT('Ctrl Pts',(0.997697504751317,-0.609396293443471,
-31.8340351723212));
#20713=CARTESIAN_POINT('Ctrl Pts',(0.953462279858224,-0.677039455355891,
-31.8398087470032));
#20714=CARTESIAN_POINT('Ctrl Pts',(0.875876982117829,-0.772264684904525,
-31.8483668447474));
#20715=CARTESIAN_POINT('Ctrl Pts',(0.847212776712624,-0.803722565967738,
-31.8512769224679));
#20716=CARTESIAN_POINT('Ctrl Pts',(0.787009152503631,-0.86261132692273,
-31.8568875280796));
#20717=CARTESIAN_POINT('Ctrl Pts',(0.755717262167963,-0.890004801972639,
-31.8595912763478));
#20718=CARTESIAN_POINT('Ctrl Pts',(0.678733697678142,-0.950425163636487,
-31.8659695744294));
#20719=CARTESIAN_POINT('Ctrl Pts',(0.63189677977743,-0.981973859333561,
-31.8696567319898));
#20720=CARTESIAN_POINT('Ctrl Pts',(0.519801354509735,-1.04643731668189,
-31.8784459259654));
#20721=CARTESIAN_POINT('Ctrl Pts',(0.453159318095688,-1.07701398350054,
-31.8835937097214));
#20722=CARTESIAN_POINT('Ctrl Pts',(0.30912384004286,-1.12765457696487,-31.8943670714784));
#20723=CARTESIAN_POINT('Ctrl Pts',(0.231242788441453,-1.14650870172707,
-31.8999922894932));
#20724=CARTESIAN_POINT('Ctrl Pts',(0.110773568709514,-1.16249701372248,
-31.9082282615955));
#20725=CARTESIAN_POINT('Ctrl Pts',(0.0692623325449389,-1.1656493189394,
-31.9109710701201));
#20726=CARTESIAN_POINT('Ctrl Pts',(-0.0454268327301759,-1.16809589961942,
-31.9184840634544));
#20727=CARTESIAN_POINT('Ctrl Pts',(-0.118656559476324,-1.16265865935421,
-31.9232749526452));
#20728=CARTESIAN_POINT('Ctrl Pts',(-0.247313507871422,-1.14109367538233,
-31.9321948832158));
#20729=CARTESIAN_POINT('Ctrl Pts',(-0.303190714654443,-1.12752207428608,
-31.9361993591496));
#20730=CARTESIAN_POINT('Ctrl Pts',(-0.452865660521723,-1.07951943878788,
-31.9472141775491));
#20731=CARTESIAN_POINT('Ctrl Pts',(-0.544157689964662,-1.03704794058161,
-31.9542499483904));
#20732=CARTESIAN_POINT('Ctrl Pts',(-0.669499700364756,-0.957123845705213,
-31.9642691289062));
#20733=CARTESIAN_POINT('Ctrl Pts',(-0.708700366708839,-0.928341028069589,
-31.9674498951241));
#20734=CARTESIAN_POINT('Ctrl Pts',(-0.798156607010517,-0.853557790951347,
-31.9751348354495));
#20735=CARTESIAN_POINT('Ctrl Pts',(-0.846532795135961,-0.805251056003578,
-31.9797251625568));
#20736=CARTESIAN_POINT('Ctrl Pts',(-0.950464210935684,-0.681991701886756,
-31.9908063714599));
#20737=CARTESIAN_POINT('Ctrl Pts',(-1.002191263051,-0.603682661018503,-31.997345447302));
#20738=CARTESIAN_POINT('Ctrl Pts',(-1.11304275244878,-0.382944202377441,
-32.0144690651066));
#20739=CARTESIAN_POINT('Ctrl Pts',(-1.15302090381803,-0.2355416839742,-32.0242610185895));
#20740=CARTESIAN_POINT('Ctrl Pts',(-1.17121369822542,0.0302875605874619,
-32.0424073410858));
#20741=CARTESIAN_POINT('Ctrl Pts',(-1.16270608476529,0.144486904507698,
-32.0502868606288));
#20742=CARTESIAN_POINT('Ctrl Pts',(-1.10479117593712,0.406453358131091,
-32.0687819686291));
#20743=CARTESIAN_POINT('Ctrl Pts',(-1.04222804244462,0.547067618273399,
-32.0788474634008));
#20744=CARTESIAN_POINT('Ctrl Pts',(-0.863884158737958,0.797961159360694,
-32.0997864489639));
#20745=CARTESIAN_POINT('Ctrl Pts',(-0.750781838165988,0.905665773067937,
-32.1103406369112));
#20746=CARTESIAN_POINT('Ctrl Pts',(-0.474269706082626,1.08072592818931,
-32.1327633981003));
#20747=CARTESIAN_POINT('Ctrl Pts',(-0.328649337640334,1.12621628952164,
-32.1428790802087));
#20748=CARTESIAN_POINT('Ctrl Pts',(-0.0880045267715734,1.16876081259411,
-32.159463210428));
#20749=CARTESIAN_POINT('Ctrl Pts',(0.0317130996195926,1.17202486743615,
-32.1675214898663));
#20750=CARTESIAN_POINT('Ctrl Pts',(0.207541202474937,1.14986260680352,-32.1797221634427));
#20751=CARTESIAN_POINT('Ctrl Pts',(0.265225746622224,1.13804061104461,-32.1838016068475));
#20752=CARTESIAN_POINT('Ctrl Pts',(0.379471890339568,1.1050092507888,-32.191937678746));
#20753=CARTESIAN_POINT('Ctrl Pts',(0.43549315896196,1.08391949249316,-32.1959752132237));
#20754=CARTESIAN_POINT('Ctrl Pts',(0.489601837133815,1.05872183713728,-32.1999999999999));
#20755=CARTESIAN_POINT('',(-0.881447090972499,1.21320766888878,-30.8075882712147));
#20756=CARTESIAN_POINT('',(-0.6859379234404,0.9441125563889,-30.61554752692));
#20757=CARTESIAN_POINT('Ctrl Pts',(-0.881406518429929,1.21312559025058,
-30.8078849673971));
#20758=CARTESIAN_POINT('Ctrl Pts',(-0.79008662599039,1.27933557882102,-30.8137160152781));
#20759=CARTESIAN_POINT('Ctrl Pts',(-0.691313381309575,1.33525609171038,
-30.8194533024385));
#20760=CARTESIAN_POINT('Ctrl Pts',(-0.489918252130208,1.42100767299626,
-30.8309935829052));
#20761=CARTESIAN_POINT('Ctrl Pts',(-0.388091655782742,1.45203456811973,
-30.8367977370922));
#20762=CARTESIAN_POINT('Ctrl Pts',(-0.172122595797077,1.49390562222026,
-30.8488414701131));
#20763=CARTESIAN_POINT('Ctrl Pts',(-0.0573076259882289,1.502956892091,-30.8550591698905));
#20764=CARTESIAN_POINT('Ctrl Pts',(0.141659514305707,1.49529218732152,-30.8654107218449));
#20765=CARTESIAN_POINT('Ctrl Pts',(0.225375475387054,1.48492949413823,-30.8696854414375));
#20766=CARTESIAN_POINT('Ctrl Pts',(0.461660801982068,1.43520771759958,-30.882150950471));
#20767=CARTESIAN_POINT('Ctrl Pts',(0.609566018273736,1.37841704093802,-30.8906597091753));
#20768=CARTESIAN_POINT('Ctrl Pts',(0.824725152900814,1.2554745072927,-30.9041453796565));
#20769=CARTESIAN_POINT('Ctrl Pts',(0.900182963410078,1.2028217148482,-30.909115708631));
#20770=CARTESIAN_POINT('Ctrl Pts',(1.08476327734415,1.04671912984802,-30.9218791144841));
#20771=CARTESIAN_POINT('Ctrl Pts',(1.18336234755058,0.933435969686118,-30.9293613811484));
#20772=CARTESIAN_POINT('Ctrl Pts',(1.3172285738265,0.722591374806512,-30.9426119478136));
#20773=CARTESIAN_POINT('Ctrl Pts',(1.36220261914603,0.633428070916348,-30.9479777546079));
#20774=CARTESIAN_POINT('Ctrl Pts',(1.4428429516675,0.425550449776397,-30.960018791922));
#20775=CARTESIAN_POINT('Ctrl Pts',(1.4735988539753,0.304792351095012,-30.9666968186304));
#20776=CARTESIAN_POINT('Ctrl Pts',(1.50058334541614,0.0867624271108834,
-30.9782427494017));
#20777=CARTESIAN_POINT('Ctrl Pts',(1.50289470475243,-0.0090133054095964,
-30.9831649796411));
#20778=CARTESIAN_POINT('Ctrl Pts',(1.48179490039278,-0.298466953504106,
-30.9984396551502));
#20779=CARTESIAN_POINT('Ctrl Pts',(1.42987621490152,-0.489656997555912,
-31.0088880132697));
#20780=CARTESIAN_POINT('Ctrl Pts',(1.2386012241916,-0.879835871463111,-31.0321233695193));
#20781=CARTESIAN_POINT('Ctrl Pts',(1.10314579046395,-1.02748310901842,-31.0424184303893));
#20782=CARTESIAN_POINT('Ctrl Pts',(0.841355375644668,-1.25518308736778,
-31.0607060142992));
#20783=CARTESIAN_POINT('Ctrl Pts',(0.671706708060022,-1.35419411522653,
-31.0708950113284));
#20784=CARTESIAN_POINT('Ctrl Pts',(0.399238767357063,-1.44907881193649,
-31.0863851114838));
#20785=CARTESIAN_POINT('Ctrl Pts',(0.306591001400567,-1.47143123103278,
-31.0915269749786));
#20786=CARTESIAN_POINT('Ctrl Pts',(0.113353143272575,-1.49850340174426,
-31.1018748998098));
#20787=CARTESIAN_POINT('Ctrl Pts',(0.0135762553281146,-1.50239730172588,
-31.1070662013325));
#20788=CARTESIAN_POINT('Ctrl Pts',(-0.25279976086019,-1.48689363127454,
-31.1210066620724));
#20789=CARTESIAN_POINT('Ctrl Pts',(-0.440327599977758,-1.4485730974684,
-31.1308870078316));
#20790=CARTESIAN_POINT('Ctrl Pts',(-0.824338933496522,-1.27143949898088,
-31.1539432665113));
#20791=CARTESIAN_POINT('Ctrl Pts',(-0.97390169357174,-1.15076855336848,
-31.1636864658054));
#20792=CARTESIAN_POINT('Ctrl Pts',(-1.14942639738023,-0.96710241579273,
-31.1768629096307));
#20793=CARTESIAN_POINT('Ctrl Pts',(-1.20864987162695,-0.892267291039145,
-31.1818226921469));
#20794=CARTESIAN_POINT('Ctrl Pts',(-1.31153191079653,-0.733178090589835,
-31.1919988181629));
#20795=CARTESIAN_POINT('Ctrl Pts',(-1.35510592769048,-0.649243111987365,
-31.1972110998056));
#20796=CARTESIAN_POINT('Ctrl Pts',(-1.4430303095048,-0.431803877659614,
-31.2099919419473));
#20797=CARTESIAN_POINT('Ctrl Pts',(-1.47664096128969,-0.295262535485362,
-31.2172154468669));
#20798=CARTESIAN_POINT('Ctrl Pts',(-1.50411912757575,-0.0322778863762428,
-31.230824171605));
#20799=CARTESIAN_POINT('Ctrl Pts',(-1.50169331600658,0.0937759591765203,
-31.2373099128508));
#20800=CARTESIAN_POINT('Ctrl Pts',(-1.45877594130903,0.385873451166313,
-31.2533154840002));
#20801=CARTESIAN_POINT('Ctrl Pts',(-1.40192168754619,0.576773620324711,
-31.2641906913579));
#20802=CARTESIAN_POINT('Ctrl Pts',(-1.24228484519573,0.844679607623427,
-31.2802472652015));
#20803=CARTESIAN_POINT('Ctrl Pts',(-1.18883912584601,0.918303367222,-31.284861711137));
#20804=CARTESIAN_POINT('Ctrl Pts',(-1.06362541041061,1.06141058899406,-31.2948277191295));
#20805=CARTESIAN_POINT('Ctrl Pts',(-0.990653681906926,1.12962368854039,
-31.3002226847462));
#20806=CARTESIAN_POINT('Ctrl Pts',(-0.834479275518156,1.24938156325568,
-31.3109555592689));
#20807=CARTESIAN_POINT('Ctrl Pts',(-0.751318553615352,1.30131156952722,
-31.3162982013493));
#20808=CARTESIAN_POINT('Ctrl Pts',(-0.552552652402147,1.39983681676189,
-31.3281230810791));
#20809=CARTESIAN_POINT('Ctrl Pts',(-0.435630188981496,1.44041399534726,
-31.3343404047184));
#20810=CARTESIAN_POINT('Ctrl Pts',(-0.132937870119536,1.50496257801301,
-31.3504040525313));
#20811=CARTESIAN_POINT('Ctrl Pts',(0.0559719993075142,1.50928152959898,
-31.3605875743258));
#20812=CARTESIAN_POINT('Ctrl Pts',(0.416632678179987,1.45186566078964,-31.3802907470301));
#20813=CARTESIAN_POINT('Ctrl Pts',(0.586857963378165,1.39229352268651,-31.3893980346239));
#20814=CARTESIAN_POINT('Ctrl Pts',(0.910640740006506,1.20620019271066,-31.4090381303016));
#20815=CARTESIAN_POINT('Ctrl Pts',(1.05917804790911,1.07788949844651,-31.41946583828));
#20816=CARTESIAN_POINT('Ctrl Pts',(1.32423117837389,0.742889010787418,-31.4423282514141));
#20817=CARTESIAN_POINT('Ctrl Pts',(1.40073910986579,0.558632045022755,-31.452494098352));
#20818=CARTESIAN_POINT('Ctrl Pts',(1.49626125117303,0.215384419002758,-31.4713146187414));
#20819=CARTESIAN_POINT('Ctrl Pts',(1.51221196691776,0.014491680411974,-31.4818312421332));
#20820=CARTESIAN_POINT('Ctrl Pts',(1.47740899534278,-0.276788453865656,
-31.4975402963852));
#20821=CARTESIAN_POINT('Ctrl Pts',(1.45682220235215,-0.369786974767944,
-31.5026323980835));
#20822=CARTESIAN_POINT('Ctrl Pts',(1.36806601562231,-0.642230151416177,
-31.517791599168));
#20823=CARTESIAN_POINT('Ctrl Pts',(1.27387636212263,-0.812521573844567,
-31.5277066552976));
#20824=CARTESIAN_POINT('Ctrl Pts',(1.02814167442595,-1.10901835949839,-31.548154594587));
#20825=CARTESIAN_POINT('Ctrl Pts',(0.878131014092237,-1.23143645550272,
-31.5586713008323));
#20826=CARTESIAN_POINT('Ctrl Pts',(0.542797830598519,-1.40952383585759,
-31.578579337433));
#20827=CARTESIAN_POINT('Ctrl Pts',(0.363013394480282,-1.46628866348356,
-31.5880421456073));
#20828=CARTESIAN_POINT('Ctrl Pts',(0.0743620682596745,-1.50154155002754,
-31.6036596732713));
#20829=CARTESIAN_POINT('Ctrl Pts',(-0.0311382941941019,-1.50311766402509,
-31.6094853829751));
#20830=CARTESIAN_POINT('Ctrl Pts',(-0.246326110710298,-1.48346206537663,
-31.6211736713795));
#20831=CARTESIAN_POINT('Ctrl Pts',(-0.355213869364278,-1.46090073589857,
-31.6269166443787));
#20832=CARTESIAN_POINT('Ctrl Pts',(-0.53321731237527,-1.40330380008982,
-31.6365687084528));
#20833=CARTESIAN_POINT('Ctrl Pts',(-0.604429361722516,-1.37413765579584,
-31.6405141016791));
#20834=CARTESIAN_POINT('Ctrl Pts',(-0.79410328740295,-1.27901266898536,
-31.6516104404927));
#20835=CARTESIAN_POINT('Ctrl Pts',(-0.905494966010469,-1.20273423832872,
-31.6589593501426));
#20836=CARTESIAN_POINT('Ctrl Pts',(-1.166901453977,-0.966788599054434,-31.678226063038));
#20837=CARTESIAN_POINT('Ctrl Pts',(-1.2772148206795,-0.803691622859537,
-31.6880116044744));
#20838=CARTESIAN_POINT('Ctrl Pts',(-1.3849448199296,-0.579839538881978,
-31.7008813038447));
#20839=CARTESIAN_POINT('Ctrl Pts',(-1.41329287853837,-0.506704748463012,
-31.7050201908034));
#20840=CARTESIAN_POINT('Ctrl Pts',(-1.47287881374097,-0.308138417722713,
-31.7162293998432));
#20841=CARTESIAN_POINT('Ctrl Pts',(-1.49412227426975,-0.179965409458075,
-31.7233765017813));
#20842=CARTESIAN_POINT('Ctrl Pts',(-1.50233949805111,0.0512896747237151,
-31.7357797099441));
#20843=CARTESIAN_POINT('Ctrl Pts',(-1.49536294654877,0.153084621763814,
-31.7410012173628));
#20844=CARTESIAN_POINT('Ctrl Pts',(-1.46151200506474,0.349489472780055,
-31.7512417022782));
#20845=CARTESIAN_POINT('Ctrl Pts',(-1.43574274826947,0.443079292656519,
-31.7562649972009));
#20846=CARTESIAN_POINT('Ctrl Pts',(-1.35324376147598,0.65860320719556,-31.7686134586091));
#20847=CARTESIAN_POINT('Ctrl Pts',(-1.28894921214917,0.77707047456878,-31.7759524714491));
#20848=CARTESIAN_POINT('Ctrl Pts',(-1.09859692931211,1.03858451421536,-31.7933795730877));
#20849=CARTESIAN_POINT('Ctrl Pts',(-0.960074498189745,1.16789073189457,
-31.8027834654643));
#20850=CARTESIAN_POINT('Ctrl Pts',(-0.656121551014658,1.35824435926684,
-31.8217597197663));
#20851=CARTESIAN_POINT('Ctrl Pts',(-0.498064699137248,1.42381470626568,
-31.8309331232312));
#20852=CARTESIAN_POINT('Ctrl Pts',(-0.14094115511042,1.50641662107625,-31.8505768131683));
#20853=CARTESIAN_POINT('Ctrl Pts',(0.0557338468603843,1.51165229967551,
-31.8605541249687));
#20854=CARTESIAN_POINT('Ctrl Pts',(0.444388507881338,1.4448535910386,-31.8814228607825));
#20855=CARTESIAN_POINT('Ctrl Pts',(0.632485824724102,1.37356746613444,-31.8919926370937));
#20856=CARTESIAN_POINT('Ctrl Pts',(0.98895705395808,1.15025371807177,-31.9144543658979));
#20857=CARTESIAN_POINT('Ctrl Pts',(1.1221288035876,1.00707400476522,-31.924529693045));
#20858=CARTESIAN_POINT('Ctrl Pts',(1.27392369897089,0.796101204632409,-31.9382013838022));
#20859=CARTESIAN_POINT('Ctrl Pts',(1.32421243107241,0.709581560557193,-31.9434492774636));
#20860=CARTESIAN_POINT('Ctrl Pts',(1.4466469402899,0.441345485206039,-31.959132347925));
#20861=CARTESIAN_POINT('Ctrl Pts',(1.49142361622571,0.252182015772013,-31.9695969023453));
#20862=CARTESIAN_POINT('Ctrl Pts',(1.5050330411194,-0.131895182047114,-31.9897595738826));
#20863=CARTESIAN_POINT('Ctrl Pts',(1.47628922826956,-0.322084931689001,
-31.9994735551462));
#20864=CARTESIAN_POINT('Ctrl Pts',(1.38141864067906,-0.5919315821454,-32.0148547383256));
#20865=CARTESIAN_POINT('Ctrl Pts',(1.34040367527535,-0.679847013725666,
-32.0201949304321));
#20866=CARTESIAN_POINT('Ctrl Pts',(1.23541296291457,-0.857179707721256,
-32.031322308911));
#20867=CARTESIAN_POINT('Ctrl Pts',(1.16939049170082,-0.944710215970665,
-32.0369916517565));
#20868=CARTESIAN_POINT('Ctrl Pts',(0.995624032465529,-1.13005097410711,
-32.0501197742209));
#20869=CARTESIAN_POINT('Ctrl Pts',(0.863278653887601,-1.24099037191773,
-32.0588622674964));
#20870=CARTESIAN_POINT('Ctrl Pts',(0.591571910837053,-1.38260099293634,
-32.0756184397751));
#20871=CARTESIAN_POINT('Ctrl Pts',(0.484976021203013,-1.42366132742166,
-32.081906458484));
#20872=CARTESIAN_POINT('Ctrl Pts',(0.252444912482356,-1.48352548355856,
-32.0946122106501));
#20873=CARTESIAN_POINT('Ctrl Pts',(0.126228242511555,-1.49940828336764,
-32.1010172840953));
#20874=CARTESIAN_POINT('Ctrl Pts',(1.77217646831623E-6,-1.49940943975982,
-32.1075644477068));
#20875=CARTESIAN_POINT('Ctrl Pts',(-1.354384777031,0.7225666776598,-30.25156091023));
#20876=CARTESIAN_POINT('Ctrl Pts',(-1.177323984063,1.054450848381,-30.27106091023));
#20877=CARTESIAN_POINT('Ctrl Pts',(-0.569111203504,1.580105774587,-30.31006091023));
#20878=CARTESIAN_POINT('Ctrl Pts',(0.6379428881994,1.553898857047,-30.36856091023));
#20879=CARTESIAN_POINT('Ctrl Pts',(1.515280082606,0.7246860501608,-30.42706091023));
#20880=CARTESIAN_POINT('Ctrl Pts',(1.610006155319,-0.4787341075376,-30.48556091023));
#20881=CARTESIAN_POINT('Ctrl Pts',(0.8731225586908,-1.434908334168,-30.54406091023));
#20882=CARTESIAN_POINT('Ctrl Pts',(-0.3147391875509,-1.649921262663,-30.60256091023));
#20883=CARTESIAN_POINT('Ctrl Pts',(-1.340034041364,-1.012724728735,-30.66106091023));
#20884=CARTESIAN_POINT('Ctrl Pts',(-1.673178974659,0.1475613323174,-30.71956091023));
#20885=CARTESIAN_POINT('Ctrl Pts',(-1.142099513493,1.231629392261,-30.77806091023));
#20886=CARTESIAN_POINT('Ctrl Pts',(-0.0211068401903,1.679540644058,-30.83656091023));
#20887=CARTESIAN_POINT('Ctrl Pts',(1.110787857823,1.259941506756,-30.89506091023));
#20888=CARTESIAN_POINT('Ctrl Pts',(1.668942351274,0.1895618522656,-30.95356091023));
#20889=CARTESIAN_POINT('Ctrl Pts',(1.365060658244,-0.9787296188165,-31.01206091023));
#20890=CARTESIAN_POINT('Ctrl Pts',(0.3561026739166,-1.641491137051,-31.07056091023));
#20891=CARTESIAN_POINT('Ctrl Pts',(-0.8367882010172,-1.456395473099,-31.12906091023));
#20892=CARTESIAN_POINT('Ctrl Pts',(-1.597464201167,-0.519047582986,-31.18756091023));
#20893=CARTESIAN_POINT('Ctrl Pts',(-1.533023655909,0.686396924418,-31.24606091023));
#20894=CARTESIAN_POINT('Ctrl Pts',(-0.6767511671866,1.53730612602,-31.30456091023));
#20895=CARTESIAN_POINT('Ctrl Pts',(0.52907443495,1.594171417921,-31.36306091023));
#20896=CARTESIAN_POINT('Ctrl Pts',(1.461624385972,0.8276209410372,-31.42156091023));
#20897=CARTESIAN_POINT('Ctrl Pts',(1.639221290546,-0.3664093696299,-31.48006091023));
#20898=CARTESIAN_POINT('Ctrl Pts',(0.9701334287918,-1.371183213173,-31.53856091023));
#20899=CARTESIAN_POINT('Ctrl Pts',(-0.2000443226221,-1.667718359793,-31.59706091023));
#20900=CARTESIAN_POINT('Ctrl Pts',(-1.266895850185,-1.102849551308,-31.65556091023));
#20901=CARTESIAN_POINT('Ctrl Pts',(-1.679374972687,0.03165926908636,-31.71406091023));
#20902=CARTESIAN_POINT('Ctrl Pts',(-1.224428737161,1.149815288114,-31.77256091023));
#20903=CARTESIAN_POINT('Ctrl Pts',(-0.1370469690625,1.674073791154,-31.83106091023));
#20904=CARTESIAN_POINT('Ctrl Pts',(1.021129492522,1.333641902982,-31.88956091023));
#20905=CARTESIAN_POINT('Ctrl Pts',(1.651847110893,0.3043759554816,-31.94806091023));
#20906=CARTESIAN_POINT('Ctrl Pts',(1.42946546972,-0.8821571614021,-32.00656091023));
#20907=CARTESIAN_POINT('Ctrl Pts',(0.4683422360403,-1.612847596885,-32.06506091023));
#20908=CARTESIAN_POINT('Ctrl Pts',(-0.3326844530463,-1.545082331076,-32.10406091023));
#20909=CARTESIAN_POINT('Ctrl Pts',(-0.6710062646147,-1.380656119664,-32.12356091023));
#20910=CARTESIAN_POINT('Ctrl Pts',(-1.235814757055,0.6593093619714,-30.32915029444));
#20911=CARTESIAN_POINT('Ctrl Pts',(-1.07425480411,0.9621386338044,-30.34865029444));
#20912=CARTESIAN_POINT('Ctrl Pts',(-0.5192881931508,1.441774942437,-30.38765029444));
#20913=CARTESIAN_POINT('Ctrl Pts',(0.5820939874436,1.417862317323,-30.44615029444));
#20914=CARTESIAN_POINT('Ctrl Pts',(1.38262443503,0.6612431933735,-30.50465029444));
#20915=CARTESIAN_POINT('Ctrl Pts',(1.469057685405,-0.4368231870542,-30.56315029444));
#20916=CARTESIAN_POINT('Ctrl Pts',(0.7966847834135,-1.309288855323,-30.62165029444));
#20917=CARTESIAN_POINT('Ctrl Pts',(-0.2871852513371,-1.50547841275,-30.68015029444));
#20918=CARTESIAN_POINT('Ctrl Pts',(-1.22272036083,-0.9240654397699,-30.73865029444));
#20919=CARTESIAN_POINT('Ctrl Pts',(-1.5267000214,0.1346430313904,-30.79715029444));
#20920=CARTESIAN_POINT('Ctrl Pts',(-1.042114070341,1.123806029122,-30.85565029444));
#20921=CARTESIAN_POINT('Ctrl Pts',(-0.01925903555941,1.532504756551,-30.91415029444));
#20922=CARTESIAN_POINT('Ctrl Pts',(1.013543602922,1.149639551094,-30.97265029444));
#20923=CARTESIAN_POINT('Ctrl Pts',(1.522834294475,0.1729666032706,-31.03115029444));
#20924=CARTESIAN_POINT('Ctrl Pts',(1.245556015057,-0.8930464419066,-31.08965029444));
#20925=CARTESIAN_POINT('Ctrl Pts',(0.3249275589301,-1.497786305004,-31.14815029444));
#20926=CARTESIAN_POINT('Ctrl Pts',(-0.7635313279386,-1.328894896257,-31.20665029444));
#20927=CARTESIAN_POINT('Ctrl Pts',(-1.457613720376,-0.4736074072494,-31.26515029444));
#20928=CARTESIAN_POINT('Ctrl Pts',(-1.398814641906,0.6263061005841,-31.32365029444));
#20929=CARTESIAN_POINT('Ctrl Pts',(-0.6175047840515,1.402722201892,-31.38215029444));
#20930=CARTESIAN_POINT('Ctrl Pts',(0.4827564554623,1.454609204823,-31.44065029444));
#20931=CARTESIAN_POINT('Ctrl Pts',(1.333666042389,0.7551666184726,-31.49915029444));
#20932=CARTESIAN_POINT('Ctrl Pts',(1.495715172889,-0.3343319518877,-31.55765029444));
#20933=CARTESIAN_POINT('Ctrl Pts',(0.8852028079061,-1.251142569086,-31.61615029444));
#20934=CARTESIAN_POINT('Ctrl Pts',(-0.1825313826277,-1.521717457694,-31.67465029444));
#20935=CARTESIAN_POINT('Ctrl Pts',(-1.15598507445,-1.006300257822,-31.73315029444));
#20936=CARTESIAN_POINT('Ctrl Pts',(-1.53235358893,0.02888764891485,-31.79165029444));
#20937=CARTESIAN_POINT('Ctrl Pts',(-1.117235757524,1.049154365167,-31.85015029444));
#20938=CARTESIAN_POINT('Ctrl Pts',(-0.1250491512082,1.527516500918,-31.90865029444));
#20939=CARTESIAN_POINT('Ctrl Pts',(0.9317344059998,1.216887824112,-31.96715029444));
#20940=CARTESIAN_POINT('Ctrl Pts',(1.507235662021,0.2777292715157,-32.02565029444));
#20941=CARTESIAN_POINT('Ctrl Pts',(1.304322488069,-0.804928449131,-32.08415029444));
#20942=CARTESIAN_POINT('Ctrl Pts',(0.4273410750521,-1.471650372119,-32.14265029444));
#20943=CARTESIAN_POINT('Ctrl Pts',(-0.303559493203,-1.409817636753,-32.18165029444));
#20944=CARTESIAN_POINT('Ctrl Pts',(-0.6122628206918,-1.259786167148,-32.20115029444));
#20945=CARTESIAN_POINT('Ctrl Pts',(-1.117244737079,0.5960520462829,-30.40673967864));
#20946=CARTESIAN_POINT('Ctrl Pts',(-0.9711856241576,0.8698264192279,-30.42623967864));
#20947=CARTESIAN_POINT('Ctrl Pts',(-0.4694651827977,1.303444110288,-30.46523967864));
#20948=CARTESIAN_POINT('Ctrl Pts',(0.5262450866879,1.2818257776,-30.52373967864));
#20949=CARTESIAN_POINT('Ctrl Pts',(1.249968787454,0.5978003365862,-30.58223967864));
#20950=CARTESIAN_POINT('Ctrl Pts',(1.32810921549,-0.3949122665708,-30.64073967864));
#20951=CARTESIAN_POINT('Ctrl Pts',(0.7202470081362,-1.183669376478,-30.69923967864));
#20952=CARTESIAN_POINT('Ctrl Pts',(-0.2596313151233,-1.361035562837,-30.75773967864));
#20953=CARTESIAN_POINT('Ctrl Pts',(-1.105406680295,-0.8354061508049,-30.81623967864));
#20954=CARTESIAN_POINT('Ctrl Pts',(-1.380221068141,0.1217247304635,-30.87473967864));
#20955=CARTESIAN_POINT('Ctrl Pts',(-0.9421286271891,1.015982665983,-30.93323967864));
#20956=CARTESIAN_POINT('Ctrl Pts',(-0.01741123092852,1.385468869044,-30.99173967864));
#20957=CARTESIAN_POINT('Ctrl Pts',(0.9162993480212,1.039337595432,-31.05023967864));
#20958=CARTESIAN_POINT('Ctrl Pts',(1.376726237677,0.1563713542756,-31.10873967864));
#20959=CARTESIAN_POINT('Ctrl Pts',(1.12605137187,-0.8073632649967,-31.16723967864));
#20960=CARTESIAN_POINT('Ctrl Pts',(0.2937524439436,-1.354081472956,-31.22573967864));
#20961=CARTESIAN_POINT('Ctrl Pts',(-0.6902744548601,-1.201394319414,-31.28423967864));
#20962=CARTESIAN_POINT('Ctrl Pts',(-1.317763239585,-0.4281672315128,-31.34273967864));
#20963=CARTESIAN_POINT('Ctrl Pts',(-1.264605627904,0.5662152767502,-31.40123967864));
#20964=CARTESIAN_POINT('Ctrl Pts',(-0.5582584009165,1.268138277765,-31.45973967864));
#20965=CARTESIAN_POINT('Ctrl Pts',(0.4364384759746,1.315046991725,-31.51823967864));
#20966=CARTESIAN_POINT('Ctrl Pts',(1.205707698806,0.682712295908,-31.57673967864));
#20967=CARTESIAN_POINT('Ctrl Pts',(1.352209055232,-0.3022545341455,-31.63523967864));
#20968=CARTESIAN_POINT('Ctrl Pts',(0.8002721870203,-1.131101924998,-31.69373967864));
#20969=CARTESIAN_POINT('Ctrl Pts',(-0.1650184426333,-1.375716555595,-31.75223967864));
#20970=CARTESIAN_POINT('Ctrl Pts',(-1.045074298715,-0.9097509643373,-31.81073967864));
#20971=CARTESIAN_POINT('Ctrl Pts',(-1.385332205172,0.02611602874334,-31.86923967864));
#20972=CARTESIAN_POINT('Ctrl Pts',(-1.010042777888,0.9484934422207,-31.92773967864));
#20973=CARTESIAN_POINT('Ctrl Pts',(-0.1130513333539,1.380959210682,-31.98623967864));
#20974=CARTESIAN_POINT('Ctrl Pts',(0.8423393194779,1.100133745242,-32.04473967864));
#20975=CARTESIAN_POINT('Ctrl Pts',(1.362624213149,0.2510825875499,-32.10323967864));
#20976=CARTESIAN_POINT('Ctrl Pts',(1.179179506419,-0.72769973686,-32.16173967864));
#20977=CARTESIAN_POINT('Ctrl Pts',(0.3863399140639,-1.330453147354,-32.22023967864));
#20978=CARTESIAN_POINT('Ctrl Pts',(-0.2744345333596,-1.27455294243,-32.25923967864));
#20979=CARTESIAN_POINT('Ctrl Pts',(-0.5535193767689,-1.138916214631,-32.27873967864));
#20980=CARTESIAN_POINT('Ctrl Pts',(-0.9986747171026,0.5327947305945,-30.48432906285));
#20981=CARTESIAN_POINT('Ctrl Pts',(-0.868116444205,0.7775142046513,-30.50382906285));
#20982=CARTESIAN_POINT('Ctrl Pts',(-0.4196421724445,1.165113278138,-30.54282906285));
#20983=CARTESIAN_POINT('Ctrl Pts',(0.4703961859321,1.145789237877,-30.60132906285));
#20984=CARTESIAN_POINT('Ctrl Pts',(1.117313139878,0.5343574797989,-30.65982906285));
#20985=CARTESIAN_POINT('Ctrl Pts',(1.187160745576,-0.3530013460875,-30.71832906285));
#20986=CARTESIAN_POINT('Ctrl Pts',(0.6438092328589,-1.058049897633,-30.77682906285));
#20987=CARTESIAN_POINT('Ctrl Pts',(-0.2320773789096,-1.216592712924,-30.83532906285));
#20988=CARTESIAN_POINT('Ctrl Pts',(-0.9880929997609,-0.74674686184,-30.89382906285));
#20989=CARTESIAN_POINT('Ctrl Pts',(-1.233742114882,0.1088064295365,-30.95232906285));
#20990=CARTESIAN_POINT('Ctrl Pts',(-0.8421431840371,0.9081593028442,-31.01082906285));
#20991=CARTESIAN_POINT('Ctrl Pts',(-0.01556342629764,1.238432981537,-31.06932906285));
#20992=CARTESIAN_POINT('Ctrl Pts',(0.8190550931203,0.9290356397707,-31.12782906285));
#20993=CARTESIAN_POINT('Ctrl Pts',(1.230618180878,0.1397761052806,-31.18632906285));
#20994=CARTESIAN_POINT('Ctrl Pts',(1.006546728684,-0.7216800880868,-31.24482906285));
#20995=CARTESIAN_POINT('Ctrl Pts',(0.2625773289571,-1.210376640909,-31.30332906285));
#20996=CARTESIAN_POINT('Ctrl Pts',(-0.6170175817815,-1.073893742571,-31.36182906285));
#20997=CARTESIAN_POINT('Ctrl Pts',(-1.177912758794,-0.3827270557762,-31.42032906285));
#20998=CARTESIAN_POINT('Ctrl Pts',(-1.130396613902,0.5061244529163,-31.47882906285));
#20999=CARTESIAN_POINT('Ctrl Pts',(-0.4990120177814,1.133554353637,-31.53732906285));
#21000=CARTESIAN_POINT('Ctrl Pts',(0.390120496487,1.175484778628,-31.59582906285));
#21001=CARTESIAN_POINT('Ctrl Pts',(1.077749355224,0.6102579733435,-31.65432906285));
#21002=CARTESIAN_POINT('Ctrl Pts',(1.208702937575,-0.2701771164033,-31.71282906285));
#21003=CARTESIAN_POINT('Ctrl Pts',(0.7153415661346,-1.011061280911,-31.77132906285));
#21004=CARTESIAN_POINT('Ctrl Pts',(-0.147505502639,-1.229715653496,-31.82982906285));
#21005=CARTESIAN_POINT('Ctrl Pts',(-0.9341635229797,-0.8132016708522,-31.88832906285));
#21006=CARTESIAN_POINT('Ctrl Pts',(-1.238310821415,0.02334440857183,-31.94682906285));
#21007=CARTESIAN_POINT('Ctrl Pts',(-0.9028497982508,0.8478325192742,-32.00532906285));
#21008=CARTESIAN_POINT('Ctrl Pts',(-0.1010535154996,1.234401920446,-32.06382906285));
#21009=CARTESIAN_POINT('Ctrl Pts',(0.752944232956,0.9833796663719,-32.12232906285));
#21010=CARTESIAN_POINT('Ctrl Pts',(1.218012764277,0.224435903584,-32.18082906285));
#21011=CARTESIAN_POINT('Ctrl Pts',(1.054036524768,-0.6504710245889,-32.23932906285));
#21012=CARTESIAN_POINT('Ctrl Pts',(0.3453387530757,-1.189255922589,-32.29782906285));
#21013=CARTESIAN_POINT('Ctrl Pts',(-0.2453095735162,-1.139288248107,-32.33682906285));
#21014=CARTESIAN_POINT('Ctrl Pts',(-0.494775932846,-1.018046262115,-32.35632906285));
#21015=CARTESIAN_POINT('Ctrl Pts',(1.58448099658799E-15,-1.4996457514538,
-32.1074280088343));
#21016=CARTESIAN_POINT('Ctrl Pts',(-4.02777456180757E-14,-1.47307126155369,
-32.1227816138083));
#21017=CARTESIAN_POINT('Ctrl Pts',(-4.08797690373025E-12,-1.44649677165354,
-32.1381352187823));
#21018=CARTESIAN_POINT('Ctrl Pts',(-4.08797690373025E-12,-1.39314602998405,
-32.1689589981181));
#21019=CARTESIAN_POINT('Ctrl Pts',(-6.03115543055E-16,-1.36636977821469,
-32.1844291724799));
#21020=CARTESIAN_POINT('Ctrl Pts',(-6.03115543055E-16,-1.33959352644542,
-32.1998993468418));
#21021=CARTESIAN_POINT('',(-0.881417612943866,1.21316727086597,-30.3080680843044));
#21022=CARTESIAN_POINT('Ctrl Pts',(-0.881271937662713,1.21292436187718,
-30.8080241838854));
#21023=CARTESIAN_POINT('Ctrl Pts',(-1.00850257770077,1.12100015634677,-30.7997573214021));
#21024=CARTESIAN_POINT('Ctrl Pts',(-1.11962151110689,1.01045334070276,-30.791142048369));
#21025=CARTESIAN_POINT('Ctrl Pts',(-1.29782368007299,0.764709539444589,
-30.7748536411824));
#21026=CARTESIAN_POINT('Ctrl Pts',(-1.36620783948847,0.633308215427597,
-30.7672924655404));
#21027=CARTESIAN_POINT('Ctrl Pts',(-1.44791553044954,0.400408010499091,
-30.7544822326199));
#21028=CARTESIAN_POINT('Ctrl Pts',(-1.47183072254183,0.302461831188457,
-30.7492472683227));
#21029=CARTESIAN_POINT('Ctrl Pts',(-1.49870865055451,0.109629087763779,
-30.738824650982));
#21030=CARTESIAN_POINT('Ctrl Pts',(-1.50269192751912,0.0158391051916832,
-30.7336538650198));
#21031=CARTESIAN_POINT('Ctrl Pts',(-1.48844953100768,-0.251855598929125,
-30.7190433780395));
#21032=CARTESIAN_POINT('Ctrl Pts',(-1.44806891166574,-0.423480947216793,
-30.7100681728756));
#21033=CARTESIAN_POINT('Ctrl Pts',(-1.34175315864756,-0.675773645942979,
-30.6958599534907));
#21034=CARTESIAN_POINT('Ctrl Pts',(-1.29359321344248,-0.764564369839684,
-30.690618628421));
#21035=CARTESIAN_POINT('Ctrl Pts',(-1.18513459159227,-0.923705254367759,
-30.6803156958803));
#21036=CARTESIAN_POINT('Ctrl Pts',(-1.12669270096378,-0.994231687201124,
-30.6752783061748));
#21037=CARTESIAN_POINT('Ctrl Pts',(-0.938545859850394,-1.18244444707684,
-30.6607782140534));
#21038=CARTESIAN_POINT('Ctrl Pts',(-0.793522725874811,-1.2832066969144,
-30.6517845335157));
#21039=CARTESIAN_POINT('Ctrl Pts',(-0.545053607980234,-1.39997528592721,
-30.6375367089199));
#21040=CARTESIAN_POINT('Ctrl Pts',(-0.449356628346627,-1.43389985036606,
-30.6322690691834));
#21041=CARTESIAN_POINT('Ctrl Pts',(-0.256824866392193,-1.48080608022622,
-30.6216685621478));
#21042=CARTESIAN_POINT('Ctrl Pts',(-0.161142963600495,-1.4942981699223,
-30.6163461134762));
#21043=CARTESIAN_POINT('Ctrl Pts',(0.0965437044720375,-1.50505707981076,
-30.6023150548004));
#21044=CARTESIAN_POINT('Ctrl Pts',(0.258322541556046,-1.48506645149598,
-30.593976335957));
#21045=CARTESIAN_POINT('Ctrl Pts',(0.513375728501787,-1.41211330395416,
-30.5802170579591));
#21046=CARTESIAN_POINT('Ctrl Pts',(0.611090204635858,-1.37300329719874,
-30.5747725770304));
#21047=CARTESIAN_POINT('Ctrl Pts',(0.795293760309478,-1.27574114267746,
-30.5636573804259));
#21048=CARTESIAN_POINT('Ctrl Pts',(0.880864790932003,-1.21831318979652,
-30.5579831919676));
#21049=CARTESIAN_POINT('Ctrl Pts',(1.05086496760408,-1.07627017131234,-30.5459381412953));
#21050=CARTESIAN_POINT('Ctrl Pts',(1.13229476874188,-0.989462653585845,
-30.5397306838153));
#21051=CARTESIAN_POINT('Ctrl Pts',(1.31267063557654,-0.746322614434621,
-30.52399325693));
#21052=CARTESIAN_POINT('Ctrl Pts',(1.39617883260761,-0.577543248151898,
-30.5144741851185));
#21053=CARTESIAN_POINT('Ctrl Pts',(1.47191857527949,-0.304326950315721,
-30.4990435204291));
#21054=CARTESIAN_POINT('Ctrl Pts',(1.48855505534371,-0.207802407227979,
-30.4936519971964));
#21055=CARTESIAN_POINT('Ctrl Pts',(1.50286798890886,-0.00518476754475829,
-30.4827983456252));
#21056=CARTESIAN_POINT('Ctrl Pts',(1.49922046596233,0.0999638418623623,
-30.4773509267098));
#21057=CARTESIAN_POINT('Ctrl Pts',(1.46369104273209,0.358095280148811,-30.4638339471291));
#21058=CARTESIAN_POINT('Ctrl Pts',(1.41636832436588,0.528094531696217,-30.4548661060413));
#21059=CARTESIAN_POINT('Ctrl Pts',(1.28560465947371,0.777895524399192,-30.4394761899898));
#21060=CARTESIAN_POINT('Ctrl Pts',(1.23584650838838,0.854597008610237,-30.4344616337474));
#21061=CARTESIAN_POINT('Ctrl Pts',(1.11320543282276,1.00976823521111,-30.4239068184296));
#21062=CARTESIAN_POINT('Ctrl Pts',(1.03870092469521,1.08581595462586,-30.4184021257723));
#21063=CARTESIAN_POINT('Ctrl Pts',(0.833653311054535,1.25586254468988,-30.4045866429208));
#21064=CARTESIAN_POINT('Ctrl Pts',(0.69364232957928,1.33917766672989,-30.3962483611893));
#21065=CARTESIAN_POINT('Ctrl Pts',(0.452710415206934,1.4332053036504,-30.3821661482874));
#21066=CARTESIAN_POINT('Ctrl Pts',(0.358915569212309,1.45945723586656,-30.3767980732763));
#21067=CARTESIAN_POINT('Ctrl Pts',(0.160658085760966,1.4941602769485,-30.3660297074887));
#21068=CARTESIAN_POINT('Ctrl Pts',(0.057009913787783,1.50135840423208,-30.3606431606162));
#21069=CARTESIAN_POINT('Ctrl Pts',(-0.19053515909408,1.49356059421536,-30.3477934729808));
#21070=CARTESIAN_POINT('Ctrl Pts',(-0.334268697842853,1.46862044317557,
-30.3403361053898));
#21071=CARTESIAN_POINT('Ctrl Pts',(-0.618615280175414,1.37522068205069,
-30.3242597935662));
#21072=CARTESIAN_POINT('Ctrl Pts',(-0.756125381298191,1.30435623160632,
-30.3157610121053));
#21073=CARTESIAN_POINT('Ctrl Pts',(-0.8812312603029,1.21295391713908,-30.3076008391023));
#21074=CARTESIAN_POINT('',(-0.685937814923959,0.944112407119636,-30.5000774675642));
#21075=CARTESIAN_POINT('',(-0.8816778784387,1.213525491562,-30.3078125));
#21076=CARTESIAN_POINT('Ctrl Pts',(-0.685548708199919,0.943590117361044,
-30.4999580574627));
#21077=CARTESIAN_POINT('Ctrl Pts',(-0.620658503056946,0.990901745737687,
-30.5054493275448));
#21078=CARTESIAN_POINT('Ctrl Pts',(-0.550959823264162,1.03163702953013,
-30.5109566740961));
#21079=CARTESIAN_POINT('Ctrl Pts',(-0.403872488361834,1.09795612075019,
-30.5220381978001));
#21080=CARTESIAN_POINT('Ctrl Pts',(-0.327257154251574,1.12290648436756,
-30.5275399734823));
#21081=CARTESIAN_POINT('Ctrl Pts',(-0.100873402982573,1.17156187918893,
-30.5432675541518));
#21082=CARTESIAN_POINT('Ctrl Pts',(0.053399591797408,1.17465261587528,-30.553424700155));
#21083=CARTESIAN_POINT('Ctrl Pts',(0.391521872713888,1.11617340314988,-30.5768753375799));
#21084=CARTESIAN_POINT('Ctrl Pts',(0.53180965214093,1.04428570792321,-30.5876876224664));
#21085=CARTESIAN_POINT('Ctrl Pts',(0.72553131493444,0.920594607136468,-30.6032043458073));
#21086=CARTESIAN_POINT('Ctrl Pts',(0.816159816510971,0.841517554690681,
-30.611101164653));
#21087=CARTESIAN_POINT('Ctrl Pts',(0.960946221710973,0.670376878708893,
-30.6263353830646));
#21088=CARTESIAN_POINT('Ctrl Pts',(1.01723879274502,0.581765626143624,-30.6337115693417));
#21089=CARTESIAN_POINT('Ctrl Pts',(1.10425141536702,0.390087082012562,-30.64834528083));
#21090=CARTESIAN_POINT('Ctrl Pts',(1.13460050240139,0.288910726357807,-30.6553271203898));
#21091=CARTESIAN_POINT('Ctrl Pts',(1.16338805497993,0.111296031839137,-30.6672934493909));
#21092=CARTESIAN_POINT('Ctrl Pts',(1.16840076223968,0.0358059784192352,
-30.6722986874147));
#21093=CARTESIAN_POINT('Ctrl Pts',(1.1640118352481,-0.106156990343197,-30.6819567814185));
#21094=CARTESIAN_POINT('Ctrl Pts',(1.15618689001219,-0.172475808382573,
-30.686599600179));
#21095=CARTESIAN_POINT('Ctrl Pts',(1.1324952743554,-0.285021426899435,-30.6947702271497));
#21096=CARTESIAN_POINT('Ctrl Pts',(1.11969541457319,-0.331193090783143,
-30.6981669611072));
#21097=CARTESIAN_POINT('Ctrl Pts',(1.06524415949267,-0.489387920864526,
-30.7097201100341));
#21098=CARTESIAN_POINT('Ctrl Pts',(1.00906889671204,-0.596548724884538,
-30.7175157393668));
#21099=CARTESIAN_POINT('Ctrl Pts',(0.907478030436901,-0.734901646249509,
-30.7288918619303));
#21100=CARTESIAN_POINT('Ctrl Pts',(0.873819215807472,-0.774897823605277,
-30.7323768988926));
#21101=CARTESIAN_POINT('Ctrl Pts',(0.804048748951575,-0.847167206515101,
-30.7392409545507));
#21102=CARTESIAN_POINT('Ctrl Pts',(0.768469068537212,-0.879620246660906,
-30.7426065220351));
#21103=CARTESIAN_POINT('Ctrl Pts',(0.695440347491846,-0.938054764308324,
-30.7492738276346));
#21104=CARTESIAN_POINT('Ctrl Pts',(0.658559073910089,-0.964127226949575,
-30.7525210802118));
#21105=CARTESIAN_POINT('Ctrl Pts',(0.582208819688217,-1.01174476378742,
-30.7588592772385));
#21106=CARTESIAN_POINT('Ctrl Pts',(0.542749389348318,-1.03331199398362,
-30.7619381584573));
#21107=CARTESIAN_POINT('Ctrl Pts',(0.416276876357301,-1.09342586330311,
-30.7713609849539));
#21108=CARTESIAN_POINT('Ctrl Pts',(0.325380070116385,-1.12400298222979,
-30.7775132584775));
#21109=CARTESIAN_POINT('Ctrl Pts',(0.190071498834436,-1.15190522952279,
-30.7866412473092));
#21110=CARTESIAN_POINT('Ctrl Pts',(0.147470992919353,-1.15827142163799,
-30.7895119494768));
#21111=CARTESIAN_POINT('Ctrl Pts',(0.0195633985643735,-1.17004221305817,
-30.7982779098936));
#21112=CARTESIAN_POINT('Ctrl Pts',(-0.0653833390363976,-1.16807622863429,
-30.8044159856939));
#21113=CARTESIAN_POINT('Ctrl Pts',(-0.191666563688748,-1.15140566703514,
-30.8135099611217));
#21114=CARTESIAN_POINT('Ctrl Pts',(-0.233832913002153,-1.14346534826818,
-30.816515879701));
#21115=CARTESIAN_POINT('Ctrl Pts',(-0.366314577040543,-1.11102808203377,
-30.8258099429263));
#21116=CARTESIAN_POINT('Ctrl Pts',(-0.4546293910922,-1.07804391131431,-30.8318420499684));
#21117=CARTESIAN_POINT('Ctrl Pts',(-0.576506740473783,-1.01517446868446,
-30.8408040974894));
#21118=CARTESIAN_POINT('Ctrl Pts',(-0.614124897463469,-0.993041057591312,
-30.8436721997507));
#21119=CARTESIAN_POINT('Ctrl Pts',(-0.681414838461067,-0.948091679732547,
-30.8491193011929));
#21120=CARTESIAN_POINT('Ctrl Pts',(-0.711441123643893,-0.925834257978619,
-30.8516833011831));
#21121=CARTESIAN_POINT('Ctrl Pts',(-0.79022740139402,-0.861034604049957,
-30.8588671848167));
#21122=CARTESIAN_POINT('Ctrl Pts',(-0.836508566353444,-0.815801487855969,
-30.8635724603074));
#21123=CARTESIAN_POINT('Ctrl Pts',(-0.905208129760981,-0.736646372968856,
-30.8710613864576));
#21124=CARTESIAN_POINT('Ctrl Pts',(-0.930070295231557,-0.704839956840183,
-30.8738968769317));
#21125=CARTESIAN_POINT('Ctrl Pts',(-0.982286842236417,-0.630564553449005,
-30.8800889328438));
#21126=CARTESIAN_POINT('Ctrl Pts',(-1.00869765789631,-0.587422341858284,
-30.883418330516));
#21127=CARTESIAN_POINT('Ctrl Pts',(-1.06170501340571,-0.48702278699212,
-30.8908180465144));
#21128=CARTESIAN_POINT('Ctrl Pts',(-1.08671765906662,-0.428906450045411,
-30.8948688018013));
#21129=CARTESIAN_POINT('Ctrl Pts',(-1.12002448009141,-0.329971499936298,
-30.9017422583765));
#21130=CARTESIAN_POINT('Ctrl Pts',(-1.1311068495569,-0.29009808489723,-30.9045072036108));
#21131=CARTESIAN_POINT('Ctrl Pts',(-1.15123618562205,-0.198246548887531,
-30.9109945668488));
#21132=CARTESIAN_POINT('Ctrl Pts',(-1.15886629216208,-0.146014505077338,
-30.9147706560545));
#21133=CARTESIAN_POINT('Ctrl Pts',(-1.16642753965937,-0.0483358449972948,
-30.921828495974));
#21134=CARTESIAN_POINT('Ctrl Pts',(-1.16728315965028,-0.00293675892899701,
-30.9251063416237));
#21135=CARTESIAN_POINT('Ctrl Pts',(-1.16423412848984,0.0764793241860627,
-30.9307261307089));
#21136=CARTESIAN_POINT('Ctrl Pts',(-1.16145205542447,0.110545851708783,
-30.9330939648108));
#21137=CARTESIAN_POINT('Ctrl Pts',(-1.1507630119261,0.196040296314932,-30.9389159856546));
#21138=CARTESIAN_POINT('Ctrl Pts',(-1.14093638520118,0.247240011612176,
-30.9423091552743));
#21139=CARTESIAN_POINT('Ctrl Pts',(-1.11415509775947,0.349773164106084,
-30.9491663254526));
#21140=CARTESIAN_POINT('Ctrl Pts',(-1.09694525695557,0.401049399726515,
-30.9526299660782));
#21141=CARTESIAN_POINT('Ctrl Pts',(-1.06191971430983,0.485244558921056,
-30.9586301629196));
#21142=CARTESIAN_POINT('Ctrl Pts',(-1.04592843859889,0.518966246414727,
-30.9611252077559));
#21143=CARTESIAN_POINT('Ctrl Pts',(-1.00667850457887,0.592004102249595,
-30.9668413737592));
#21144=CARTESIAN_POINT('Ctrl Pts',(-0.982690543030822,0.630789580669632,
-30.9700809744543));
#21145=CARTESIAN_POINT('Ctrl Pts',(-0.92577731115898,0.711764805256299,
-30.9771871833879));
#21146=CARTESIAN_POINT('Ctrl Pts',(-0.892021085752503,0.753375714006476,
-30.9810643272464));
#21147=CARTESIAN_POINT('Ctrl Pts',(-0.831157513826872,0.81885589047688,
-30.9874031052895));
#21148=CARTESIAN_POINT('Ctrl Pts',(-0.805487538846159,0.844079160218681,
-30.9899110954614));
#21149=CARTESIAN_POINT('Ctrl Pts',(-0.741884245488248,0.901166354308377,
-30.995701440776));
#21150=CARTESIAN_POINT('Ctrl Pts',(-0.702972232118756,0.931952904362451,
-30.9989337662652));
#21151=CARTESIAN_POINT('Ctrl Pts',(-0.618514271893681,0.990541324608438,
-31.0055765993046));
#21152=CARTESIAN_POINT('Ctrl Pts',(-0.572684700748231,1.01794232834898,
-31.0089834107297));
#21153=CARTESIAN_POINT('Ctrl Pts',(-0.49255597576707,1.05855280552911,-31.0148746919682));
#21154=CARTESIAN_POINT('Ctrl Pts',(-0.459157642464918,1.07351338031607,
-31.0173157459797));
#21155=CARTESIAN_POINT('Ctrl Pts',(-0.362257512762512,1.11129644287772,
-31.0244646695162));
#21156=CARTESIAN_POINT('Ctrl Pts',(-0.297410848298703,1.13011301102836,
-31.0292997106953));
#21157=CARTESIAN_POINT('Ctrl Pts',(-0.187124706409844,1.15211935516333,
-31.0373816939126));
#21158=CARTESIAN_POINT('Ctrl Pts',(-0.142289990560102,1.15841330716532,
-31.0406284239081));
#21159=CARTESIAN_POINT('Ctrl Pts',(-0.063176738898904,1.16497102653747,
-31.046208231521));
#21160=CARTESIAN_POINT('Ctrl Pts',(-0.0289746663040221,1.16633112542234,
-31.0485702431819));
#21161=CARTESIAN_POINT('Ctrl Pts',(0.0593084551231717,1.16604144539294,
-31.0545031810733));
#21162=CARTESIAN_POINT('Ctrl Pts',(0.113395661910786,1.16218189970294,-31.0579956853853));
#21163=CARTESIAN_POINT('Ctrl Pts',(0.224842541394679,1.14641006745828,-31.0652428658355));
#21164=CARTESIAN_POINT('Ctrl Pts',(0.282100957497795,1.1338736788578,-31.0689971062012));
#21165=CARTESIAN_POINT('Ctrl Pts',(0.374052171032848,1.10606227821236,-31.0754427222994));
#21166=CARTESIAN_POINT('Ctrl Pts',(0.409453520323982,1.09337035163398,-31.0780348427351));
#21167=CARTESIAN_POINT('Ctrl Pts',(0.517476805264023,1.04857455727421,-31.0862385359748));
#21168=CARTESIAN_POINT('Ctrl Pts',(0.587682831432323,1.01055892366634,-31.0920033516305));
#21169=CARTESIAN_POINT('Ctrl Pts',(0.690824163490302,0.940622392373098,
-31.1008475785035));
#21170=CARTESIAN_POINT('Ctrl Pts',(0.72681028023883,0.913113517205756,-31.1040148988039));
#21171=CARTESIAN_POINT('Ctrl Pts',(0.817984776836416,0.834813237889736,
-31.1121663288315));
#21172=CARTESIAN_POINT('Ctrl Pts',(0.870253412544716,0.780594317299417,
-31.1169396107474));
#21173=CARTESIAN_POINT('Ctrl Pts',(0.937220513377292,0.695987892557664,
-31.1239148245526));
#21174=CARTESIAN_POINT('Ctrl Pts',(0.956547942992973,0.669287829234583,
-31.1260589017073));
#21175=CARTESIAN_POINT('Ctrl Pts',(0.996400989999189,0.60878603062681,-31.1308845701165));
#21176=CARTESIAN_POINT('Ctrl Pts',(1.01635907202192,0.574675644168678,-31.1335875623297));
#21177=CARTESIAN_POINT('Ctrl Pts',(1.07408883199262,0.46327759563795,-31.1423270895464));
#21178=CARTESIAN_POINT('Ctrl Pts',(1.1051196110236,0.382453701872699,-31.1485422957239));
#21179=CARTESIAN_POINT('Ctrl Pts',(1.13988537104464,0.251184830520502,-31.1581469742182));
#21180=CARTESIAN_POINT('Ctrl Pts',(1.14962127517682,0.202259736242942,-31.1616242141299));
#21181=CARTESIAN_POINT('Ctrl Pts',(1.16481115260415,0.0892323089346831,
-31.1693363582519));
#21182=CARTESIAN_POINT('Ctrl Pts',(1.16819757460234,0.0248471507560758,
-31.173462210906));
#21183=CARTESIAN_POINT('Ctrl Pts',(1.16505492615128,-0.0755507344237222,
-31.1799619715207));
#21184=CARTESIAN_POINT('Ctrl Pts',(1.16221017433194,-0.111704713006625,
-31.182319041523));
#21185=CARTESIAN_POINT('Ctrl Pts',(1.15158005006472,-0.194696702061016,
-31.1879013545843));
#21186=CARTESIAN_POINT('Ctrl Pts',(1.14259382155944,-0.241266739154483,
-31.1911518502856));
#21187=CARTESIAN_POINT('Ctrl Pts',(1.10912772555809,-0.371437981360074,
-31.2005258451499));
#21188=CARTESIAN_POINT('Ctrl Pts',(1.07796884465094,-0.453349820889493,
-31.2067744058992));
#21189=CARTESIAN_POINT('Ctrl Pts',(1.01993868550944,-0.566914805651578,
-31.2157311300408));
#21190=CARTESIAN_POINT('Ctrl Pts',(0.999685483652604,-0.602026275118691,
-31.2185454180568));
#21191=CARTESIAN_POINT('Ctrl Pts',(0.943447679441216,-0.688917601007358,
-31.2255910197575));
#21192=CARTESIAN_POINT('Ctrl Pts',(0.904986255469571,-0.739088189196026,
-31.2296842482066));
#21193=CARTESIAN_POINT('Ctrl Pts',(0.83239505206359,-0.819144896900878,
-31.2367052600699));
#21194=CARTESIAN_POINT('Ctrl Pts',(0.800287439985633,-0.850591997282813,
-31.2396426579672));
#21195=CARTESIAN_POINT('Ctrl Pts',(0.677247083649768,-0.957343264563837,
-31.2506083772752));
#21196=CARTESIAN_POINT('Ctrl Pts',(0.576361367480104,-1.02061902569622,
-31.2589908100937));
#21197=CARTESIAN_POINT('Ctrl Pts',(0.421633955074437,-1.08851278412317,
-31.2708526489429));
#21198=CARTESIAN_POINT('Ctrl Pts',(0.373333306378296,-1.1060982468434,-31.274429506583));
#21199=CARTESIAN_POINT('Ctrl Pts',(0.268024200900743,-1.13685382344944,
-31.2819219010863));
#21200=CARTESIAN_POINT('Ctrl Pts',(0.210733858165044,-1.14907162017185,
-31.2857759753666));
#21201=CARTESIAN_POINT('Ctrl Pts',(0.0850061683590383,-1.16595350028459,
-31.2940714011991));
#21202=CARTESIAN_POINT('Ctrl Pts',(0.0171193143066746,-1.16881571421432,
-31.2985589381589));
#21203=CARTESIAN_POINT('Ctrl Pts',(-0.170348216791286,-1.16010129180361,
-31.3113707279674));
#21204=CARTESIAN_POINT('Ctrl Pts',(-0.289034321660633,-1.13599694319867,
-31.3198463246205));
#21205=CARTESIAN_POINT('Ctrl Pts',(-0.468120182557069,-1.07066515186562,
-31.3330824400782));
#21206=CARTESIAN_POINT('Ctrl Pts',(-0.532693517969684,-1.04033994702365,
-31.3379530166625));
#21207=CARTESIAN_POINT('Ctrl Pts',(-0.625391610677575,-0.985851723054238,
-31.3450977313131));
#21208=CARTESIAN_POINT('Ctrl Pts',(-0.655959765253003,-0.965871197408253,
-31.3474902215926));
#21209=CARTESIAN_POINT('Ctrl Pts',(-0.777879976153246,-0.877380172770267,
-31.357486367411));
#21210=CARTESIAN_POINT('Ctrl Pts',(-0.859912618212914,-0.796237594718653,
-31.3653439434294));
#21211=CARTESIAN_POINT('Ctrl Pts',(-0.975254435297355,-0.643948339349487,
-31.3785854260959));
#21212=CARTESIAN_POINT('Ctrl Pts',(-1.01577210878922,-0.578125335361136,
-31.3839392354365));
#21213=CARTESIAN_POINT('Ctrl Pts',(-1.10899380208953,-0.387246913439551,
-31.3985453285889));
#21214=CARTESIAN_POINT('Ctrl Pts',(-1.14344335550353,-0.264663157205293,
-31.4068122887934));
#21215=CARTESIAN_POINT('Ctrl Pts',(-1.17590076084456,0.00819027975376396,
-31.4254655864227));
#21216=CARTESIAN_POINT('Ctrl Pts',(-1.16463926395832,0.161289680328769,
-31.4359077152906));
#21217=CARTESIAN_POINT('Ctrl Pts',(-1.08535270579174,0.45572979035119,-31.4568415946505));
#21218=CARTESIAN_POINT('Ctrl Pts',(-1.01670874950091,0.592794756408663,
-31.466956769279));
#21219=CARTESIAN_POINT('Ctrl Pts',(-0.827849909053765,0.83538314803652,
-31.487852646732));
#21220=CARTESIAN_POINT('Ctrl Pts',(-0.709617583089645,0.93843676949597,
-31.4983682348508));
#21221=CARTESIAN_POINT('Ctrl Pts',(-0.511147348714834,1.05180989497623,
-31.5140645531066));
#21222=CARTESIAN_POINT('Ctrl Pts',(-0.443272565048419,1.08210604098259,
-31.5191611936776));
#21223=CARTESIAN_POINT('Ctrl Pts',(-0.230901793688486,1.15296249320239,
-31.5344190291072));
#21224=CARTESIAN_POINT('Ctrl Pts',(-0.0801266960605881,1.17280484436255,
-31.5444358079042));
#21225=CARTESIAN_POINT('Ctrl Pts',(0.221971670579917,1.15577877094791,-31.5650280299048));
#21226=CARTESIAN_POINT('Ctrl Pts',(0.369673902437772,1.11746614756773,-31.575591324995));
#21227=CARTESIAN_POINT('Ctrl Pts',(0.622160525775805,0.994452459531914,
-31.5946539956718));
#21228=CARTESIAN_POINT('Ctrl Pts',(0.727539007713757,0.920189142633611,
-31.6030889670126));
#21229=CARTESIAN_POINT('Ctrl Pts',(0.916982964614389,0.73477608994851,-31.6210410579286));
#21230=CARTESIAN_POINT('Ctrl Pts',(0.996272708142201,0.623142279337944,
-31.6307046019878));
#21231=CARTESIAN_POINT('Ctrl Pts',(1.08433698239759,0.435193202490311,-31.6449148687832));
#21232=CARTESIAN_POINT('Ctrl Pts',(1.10822642430814,0.369663308560383,-31.6495634464446));
#21233=CARTESIAN_POINT('Ctrl Pts',(1.15766448812734,0.185711327184666,-31.6622430262217));
#21234=CARTESIAN_POINT('Ctrl Pts',(1.17132519379187,0.0639675994095021,
-31.6702435733044));
#21235=CARTESIAN_POINT('Ctrl Pts',(1.16300828851598,-0.110853971756192,
-31.6824209503072));
#21236=CARTESIAN_POINT('Ctrl Pts',(1.15655334679051,-0.164270613099354,
-31.6862649953204));
#21237=CARTESIAN_POINT('Ctrl Pts',(1.13596513152833,-0.271414406573397,
-31.6939847321905));
#21238=CARTESIAN_POINT('Ctrl Pts',(1.1215795497405,-0.325113706990364,-31.6978144376222));
#21239=CARTESIAN_POINT('Ctrl Pts',(1.08263550331581,-0.438176204048292,
-31.7058935031972));
#21240=CARTESIAN_POINT('Ctrl Pts',(1.05682806402532,-0.497140478928953,
-31.7101306170283));
#21241=CARTESIAN_POINT('Ctrl Pts',(0.98300300796349,-0.63449965815748,-31.7204223140629));
#21242=CARTESIAN_POINT('Ctrl Pts',(0.930173045980556,-0.710361834246211,
-31.7264812348101));
#21243=CARTESIAN_POINT('Ctrl Pts',(0.838930525074047,-0.812502698043108,
-31.7359377792509));
#21244=CARTESIAN_POINT('Ctrl Pts',(0.807039546152215,-0.844135571885244,
-31.7391179237103));
#21245=CARTESIAN_POINT('Ctrl Pts',(0.726353665209184,-0.91520566837048,
-31.746804006435));
#21246=CARTESIAN_POINT('Ctrl Pts',(0.676066014753284,-0.952672061924379,
-31.7512732634903));
#21247=CARTESIAN_POINT('Ctrl Pts',(0.586597396153142,-1.00892317739801,
-31.7585101855706));
#21248=CARTESIAN_POINT('Ctrl Pts',(0.548805759549127,-1.02989821143397,
-31.7614003698864));
#21249=CARTESIAN_POINT('Ctrl Pts',(0.431409242179501,-1.08697182239586,
-31.7700425151364));
#21250=CARTESIAN_POINT('Ctrl Pts',(0.348579506835605,-1.11657141359353,
-31.7756961700068));
#21251=CARTESIAN_POINT('Ctrl Pts',(0.217677855472974,-1.14733111137362,
-31.7846649392895));
#21252=CARTESIAN_POINT('Ctrl Pts',(0.171191373914171,-1.15531031302035,
-31.7878568696945));
#21253=CARTESIAN_POINT('Ctrl Pts',(0.0895549583645699,-1.16408050808528,
-31.7935895247711));
#21254=CARTESIAN_POINT('Ctrl Pts',(0.054609741640134,-1.16617767881962,
-31.796086555492));
#21255=CARTESIAN_POINT('Ctrl Pts',(-0.0467913736064708,-1.16763349643548,
-31.8033629679176));
#21256=CARTESIAN_POINT('Ctrl Pts',(-0.113337928350958,-1.16281548208516,
-31.8081612838819));
#21257=CARTESIAN_POINT('Ctrl Pts',(-0.235278263563502,-1.14362810067056,
-31.8166300151622));
#21258=CARTESIAN_POINT('Ctrl Pts',(-0.290908321981227,-1.13073008081567,
-31.8204024646212));
#21259=CARTESIAN_POINT('Ctrl Pts',(-0.444812112979426,-1.08322628172866,
-31.830945564078));
#21260=CARTESIAN_POINT('Ctrl Pts',(-0.540311217364741,-1.03946587487301,
-31.837621805171));
#21261=CARTESIAN_POINT('Ctrl Pts',(-0.673100283251339,-0.954845681333125,
-31.8484417282243));
#21262=CARTESIAN_POINT('Ctrl Pts',(-0.715792773943846,-0.923107745328805,
-31.8522365879894));
#21263=CARTESIAN_POINT('Ctrl Pts',(-0.803852241302621,-0.847752091635972,
-31.8605787399954));
#21264=CARTESIAN_POINT('Ctrl Pts',(-0.848313210756834,-0.802950806528635,
-31.8651310439244));
#21265=CARTESIAN_POINT('Ctrl Pts',(-0.916115433980169,-0.722848737228883,
-31.8723664669261));
#21266=CARTESIAN_POINT('Ctrl Pts',(-0.941571571027832,-0.689329219815559,
-31.8751785748015));
#21267=CARTESIAN_POINT('Ctrl Pts',(-0.99975857647731,-0.603675302149774,
-31.8819956493985));
#21268=CARTESIAN_POINT('Ctrl Pts',(-1.03040277506431,-0.550095551789753,
-31.88595080696));
#21269=CARTESIAN_POINT('Ctrl Pts',(-1.07866822297917,-0.447757935699058,
-31.8933197268893));
#21270=CARTESIAN_POINT('Ctrl Pts',(-1.09758968721411,-0.399614243566427,
-31.8967191126898));
#21271=CARTESIAN_POINT('Ctrl Pts',(-1.12524986139922,-0.312005362231876,
-31.9029894599813));
#21272=CARTESIAN_POINT('Ctrl Pts',(-1.13524081419106,-0.273143485089577,
-31.9058100800701));
#21273=CARTESIAN_POINT('Ctrl Pts',(-1.15655793595677,-0.167633623548991,
-31.9134992139986));
#21274=CARTESIAN_POINT('Ctrl Pts',(-1.16408685545047,-0.100190605984288,
-31.9184390059287));
#21275=CARTESIAN_POINT('Ctrl Pts',(-1.16671949918186,0.000995598857348756,
-31.9255822026249));
#21276=CARTESIAN_POINT('Ctrl Pts',(-1.16616740721873,0.0346408626275563,
-31.927906725977));
#21277=CARTESIAN_POINT('Ctrl Pts',(-1.16225049598424,0.101363110558704,
-31.9324145875288));
#21278=CARTESIAN_POINT('Ctrl Pts',(-1.15891999235791,0.134442845400991,
-31.9346064296027));
#21279=CARTESIAN_POINT('Ctrl Pts',(-1.14378268241922,0.240159071561426,
-31.9415747696343));
#21280=CARTESIAN_POINT('Ctrl Pts',(-1.12659062347451,0.312042548769722,
-31.9462565676558));
#21281=CARTESIAN_POINT('Ctrl Pts',(-1.09092949322726,0.415884557053626,
-31.9534961242054));
#21282=CARTESIAN_POINT('Ctrl Pts',(-1.07752966429866,0.449614269739891,
-31.9559292779484));
#21283=CARTESIAN_POINT('Ctrl Pts',(-1.0374731109826,0.537627087276782,-31.9626076401286));
#21284=CARTESIAN_POINT('Ctrl Pts',(-1.00807686224237,0.590494188094113,
-31.9669474270401));
#21285=CARTESIAN_POINT('Ctrl Pts',(-0.939126696925382,0.694708303515753,
-31.9759472815253));
#21286=CARTESIAN_POINT('Ctrl Pts',(-0.898980851929762,0.745692992216044,
-31.9806067047616));
#21287=CARTESIAN_POINT('Ctrl Pts',(-0.830179916132025,0.819829954206266,
-31.987550978645));
#21288=CARTESIAN_POINT('Ctrl Pts',(-0.804137417975539,0.845434094234728,
-31.9899822639371));
#21289=CARTESIAN_POINT('Ctrl Pts',(-0.737655511072942,0.905038542932737,
-31.9958345678478));
#21290=CARTESIAN_POINT('Ctrl Pts',(-0.695981335925813,0.937675454780674,
-31.9992128271908));
#21291=CARTESIAN_POINT('Ctrl Pts',(-0.612847639332127,0.994093419831662,
-32.0057054755517));
#21292=CARTESIAN_POINT('Ctrl Pts',(-0.571771963705075,1.01842145541926,
-32.0088137038318));
#21293=CARTESIAN_POINT('Ctrl Pts',(-0.495496118829579,1.05726047115192,
-32.0146036163438));
#21294=CARTESIAN_POINT('Ctrl Pts',(-0.460858658671628,1.07272788565039,
-32.0172423593459));
#21295=CARTESIAN_POINT('Ctrl Pts',(-0.375133633164121,1.10604743893886,
-32.0237480290935));
#21296=CARTESIAN_POINT('Ctrl Pts',(-0.323309374888746,1.12209275398005,
-32.0276600588066));
#21297=CARTESIAN_POINT('Ctrl Pts',(-0.221635181656419,1.14609414865391,
-32.035151397609));
#21298=CARTESIAN_POINT('Ctrl Pts',(-0.171876293416826,1.15454058196787,
-32.0387355372415));
#21299=CARTESIAN_POINT('Ctrl Pts',(-0.0877502387182354,1.16340157106644,
-32.0445526251554));
#21300=CARTESIAN_POINT('Ctrl Pts',(-0.0535558392802562,1.16552299988754,
-32.0468426510691));
#21301=CARTESIAN_POINT('Ctrl Pts',(0.0270083813386109,1.16703043450772,
-32.0521342104412));
#21302=CARTESIAN_POINT('Ctrl Pts',(0.0734045328626228,1.16518204041798,
-32.0551059263961));
#21303=CARTESIAN_POINT('Ctrl Pts',(0.171858372962463,1.15533764184338,-32.0614809553558));
#21304=CARTESIAN_POINT('Ctrl Pts',(0.223908914150883,1.14653962663329,-32.064894866051));
#21305=CARTESIAN_POINT('Ctrl Pts',(0.316431900889636,1.12404973179581,-32.0713318545482));
#21306=CARTESIAN_POINT('Ctrl Pts',(0.357074873436082,1.11169392879419,-32.0742859596744));
#21307=CARTESIAN_POINT('Ctrl Pts',(0.456782879970018,1.07529717055788,-32.0817878254199));
#21308=CARTESIAN_POINT('Ctrl Pts',(0.514847053636697,1.04850353644109,-32.0863907615577));
#21309=CARTESIAN_POINT('Ctrl Pts',(0.609764637786685,0.995107450904462,
-32.0941404178487));
#21310=CARTESIAN_POINT('Ctrl Pts',(0.64789339688654,0.970707018317168,-32.0973219442031));
#21311=CARTESIAN_POINT('Ctrl Pts',(0.715151547512504,0.922068492094722,
-32.1029949487002));
#21312=CARTESIAN_POINT('Ctrl Pts',(0.744736439003466,0.898452960557686,
-32.1055032684934));
#21313=CARTESIAN_POINT('Ctrl Pts',(0.818267481323139,0.83372917772617,-32.1118913711226));
#21314=CARTESIAN_POINT('Ctrl Pts',(0.860368514566787,0.790533037148104,
-32.1157159401581));
#21315=CARTESIAN_POINT('Ctrl Pts',(0.923449901262993,0.71458664340485,-32.1221795037161));
#21316=CARTESIAN_POINT('Ctrl Pts',(0.94642154334661,0.68384088381028,-32.1247457808902));
#21317=CARTESIAN_POINT('Ctrl Pts',(1.00557045651288,0.59563248486742,-32.1320332235485));
#21318=CARTESIAN_POINT('Ctrl Pts',(1.03824014728665,0.536068984602925,-32.1368509098396));
#21319=CARTESIAN_POINT('Ctrl Pts',(1.09664652215412,0.403931737157978,-32.1471559960423));
#21320=CARTESIAN_POINT('Ctrl Pts',(1.12088236127104,0.330622819452228,-32.152646886106));
#21321=CARTESIAN_POINT('Ctrl Pts',(1.14658333970841,0.217189487467516,-32.1605896802752));
#21322=CARTESIAN_POINT('Ctrl Pts',(1.15339342276266,0.178237339655661,-32.1632099946067));
#21323=CARTESIAN_POINT('Ctrl Pts',(1.16657974788419,0.0711945325339807,
-32.1702374938604));
#21324=CARTESIAN_POINT('Ctrl Pts',(1.16901560357053,0.00250273317850058,
-32.1745827432116));
#21325=CARTESIAN_POINT('Ctrl Pts',(1.16242719852251,-0.113341789505422,
-32.1823079664126));
#21326=CARTESIAN_POINT('Ctrl Pts',(1.15674237783295,-0.160460199536454,
-32.1855532645071));
#21327=CARTESIAN_POINT('Ctrl Pts',(1.13876044634579,-0.258614577418294,
-32.1925001731439));
#21328=CARTESIAN_POINT('Ctrl Pts',(1.12582551001773,-0.309528934911987,
-32.1962128878324));
#21329=CARTESIAN_POINT('Ctrl Pts',(1.10959412583112,-0.35936066950901,-32.1999249889109));
#21330=CARTESIAN_POINT('Ctrl Pts',(-1.015482192511,0.5750263216907,-30.425575843));
#21331=CARTESIAN_POINT('Ctrl Pts',(-0.8824095367636,0.8100293243789,-30.44399167037));
#21332=CARTESIAN_POINT('Ctrl Pts',(-0.4470880869402,1.18276829068,-30.48082332512));
#21333=CARTESIAN_POINT('Ctrl Pts',(0.4133389835427,1.195144688561,-30.53607080725));
#21334=CARTESIAN_POINT('Ctrl Pts',(1.082287319525,0.6540128508907,-30.59131828937));
#21335=CARTESIAN_POINT('Ctrl Pts',(1.250228977982,-0.189832146326,-30.6465657715));
#21336=CARTESIAN_POINT('Ctrl Pts',(0.8393735447346,-0.945811051386,-30.70181325362));
#21337=CARTESIAN_POINT('Ctrl Pts',(0.03993616735796,-1.263926564634,-30.75706073575));
#21338=CARTESIAN_POINT('Ctrl Pts',(-0.7779901316111,-0.9969138795045,-30.81230821787));
#21339=CARTESIAN_POINT('Ctrl Pts',(-1.235749089843,-0.2683839185767,-30.8675557));
#21340=CARTESIAN_POINT('Ctrl Pts',(-1.121423396098,0.5843931352325,-30.92280318212));
#21341=CARTESIAN_POINT('Ctrl Pts',(-0.4879395772335,1.166627935668,-30.97805066425));
#21342=CARTESIAN_POINT('Ctrl Pts',(0.3714337559552,1.208777371376,-31.03329814637));
#21343=CARTESIAN_POINT('Ctrl Pts',(1.058853438626,0.691328550783,-31.0885456285));
#21344=CARTESIAN_POINT('Ctrl Pts',(1.256081499646,-0.1461678338278,-31.14379311062));
#21345=CARTESIAN_POINT('Ctrl Pts',(0.8718120611923,-0.9159964516181,-31.19904059275));
#21346=CARTESIAN_POINT('Ctrl Pts',(0.08394099831018,-1.261768472513,-31.25428807487));
#21347=CARTESIAN_POINT('Ctrl Pts',(-0.7427901868119,-1.023410234361,-31.309535557));
#21348=CARTESIAN_POINT('Ctrl Pts',(-1.225649866438,-0.3112686529751,-31.36478303912));
#21349=CARTESIAN_POINT('Ctrl Pts',(-1.141100239542,0.5449734055297,-31.42003052125));
#21350=CARTESIAN_POINT('Ctrl Pts',(-0.5282831903702,1.148922382135,-31.47527800337));
#21351=CARTESIAN_POINT('Ctrl Pts',(0.3291002778155,1.220982709444,-31.5305254855));
#21352=CARTESIAN_POINT('Ctrl Pts',(1.034128194939,0.7277943700298,-31.58577296762));
#21353=CARTESIAN_POINT('Ctrl Pts',(1.260410936535,-0.1023232250025,-31.64102044975));
#21354=CARTESIAN_POINT('Ctrl Pts',(0.9031918799483,-0.8850707304042,-31.69626793187));
#21355=CARTESIAN_POINT('Ctrl Pts',(0.1278440645328,-1.258078549202,-31.751515414));
#21356=CARTESIAN_POINT('Ctrl Pts',(-0.7066886712758,-1.048664412443,-31.80676289612));
#21357=CARTESIAN_POINT('Ctrl Pts',(-1.214062705292,-0.3537753607434,-31.86201037825));
#21358=CARTESIAN_POINT('Ctrl Pts',(-1.159392542789,0.5048914975012,-31.91725786037));
#21359=CARTESIAN_POINT('Ctrl Pts',(-0.5679833167426,1.129824629341,-31.9725053425));
#21360=CARTESIAN_POINT('Ctrl Pts',(0.2863590197545,1.23169686325,-32.02775282462));
#21361=CARTESIAN_POINT('Ctrl Pts',(1.008178628936,0.7634106326662,-32.08300030675));
#21362=CARTESIAN_POINT('Ctrl Pts',(1.263094839915,-0.05848087125908,-32.13824778887));
#21363=CARTESIAN_POINT('Ctrl Pts',(1.043636050887,-0.5878927540068,-32.17507944362));
#21364=CARTESIAN_POINT('Ctrl Pts',(0.8614506246688,-0.7872497540188,-32.193495271));
#21365=CARTESIAN_POINT('Ctrl Pts',(-1.015482192511,0.5750263216907,-30.49106798064));
#21366=CARTESIAN_POINT('Ctrl Pts',(-0.8824095367636,0.8100293243789,-30.50948380802));
#21367=CARTESIAN_POINT('Ctrl Pts',(-0.4470880869402,1.18276829068,-30.54631546277));
#21368=CARTESIAN_POINT('Ctrl Pts',(0.4133389835427,1.195144688561,-30.60156294489));
#21369=CARTESIAN_POINT('Ctrl Pts',(1.082287319525,0.6540128508907,-30.65681042702));
#21370=CARTESIAN_POINT('Ctrl Pts',(1.250228977982,-0.189832146326,-30.71205790914));
#21371=CARTESIAN_POINT('Ctrl Pts',(0.8393735447346,-0.945811051386,-30.76730539127));
#21372=CARTESIAN_POINT('Ctrl Pts',(0.03993616735796,-1.263926564634,-30.82255287339));
#21373=CARTESIAN_POINT('Ctrl Pts',(-0.7779901316111,-0.9969138795045,-30.87780035552));
#21374=CARTESIAN_POINT('Ctrl Pts',(-1.235749089843,-0.2683839185767,-30.93304783764));
#21375=CARTESIAN_POINT('Ctrl Pts',(-1.121423396098,0.5843931352325,-30.98829531976));
#21376=CARTESIAN_POINT('Ctrl Pts',(-0.4879395772335,1.166627935668,-31.04354280189));
#21377=CARTESIAN_POINT('Ctrl Pts',(0.3714337559552,1.208777371376,-31.09879028401));
#21378=CARTESIAN_POINT('Ctrl Pts',(1.058853438626,0.691328550783,-31.15403776614));
#21379=CARTESIAN_POINT('Ctrl Pts',(1.256081499646,-0.1461678338278,-31.20928524826));
#21380=CARTESIAN_POINT('Ctrl Pts',(0.8718120611923,-0.9159964516181,-31.26453273039));
#21381=CARTESIAN_POINT('Ctrl Pts',(0.08394099831018,-1.261768472513,-31.31978021251));
#21382=CARTESIAN_POINT('Ctrl Pts',(-0.7427901868119,-1.023410234361,-31.37502769464));
#21383=CARTESIAN_POINT('Ctrl Pts',(-1.225649866438,-0.3112686529751,-31.43027517676));
#21384=CARTESIAN_POINT('Ctrl Pts',(-1.141100239542,0.5449734055297,-31.48552265889));
#21385=CARTESIAN_POINT('Ctrl Pts',(-0.5282831903702,1.148922382135,-31.54077014101));
#21386=CARTESIAN_POINT('Ctrl Pts',(0.3291002778155,1.220982709444,-31.59601762314));
#21387=CARTESIAN_POINT('Ctrl Pts',(1.034128194939,0.7277943700298,-31.65126510526));
#21388=CARTESIAN_POINT('Ctrl Pts',(1.260410936535,-0.1023232250025,-31.70651258739));
#21389=CARTESIAN_POINT('Ctrl Pts',(0.9031918799483,-0.8850707304042,-31.76176006951));
#21390=CARTESIAN_POINT('Ctrl Pts',(0.1278440645328,-1.258078549202,-31.81700755164));
#21391=CARTESIAN_POINT('Ctrl Pts',(-0.7066886712758,-1.048664412443,-31.87225503376));
#21392=CARTESIAN_POINT('Ctrl Pts',(-1.214062705292,-0.3537753607434,-31.92750251589));
#21393=CARTESIAN_POINT('Ctrl Pts',(-1.159392542789,0.5048914975012,-31.98274999801));
#21394=CARTESIAN_POINT('Ctrl Pts',(-0.5679833167426,1.129824629341,-32.03799748014));
#21395=CARTESIAN_POINT('Ctrl Pts',(0.2863590197545,1.23169686325,-32.09324496226));
#21396=CARTESIAN_POINT('Ctrl Pts',(1.008178628936,0.7634106326662,-32.14849244439));
#21397=CARTESIAN_POINT('Ctrl Pts',(1.263094839915,-0.05848087125908,-32.20373992651));
#21398=CARTESIAN_POINT('Ctrl Pts',(1.043636050887,-0.5878927540068,-32.24057158126));
#21399=CARTESIAN_POINT('Ctrl Pts',(0.8614506246688,-0.7872497540188,-32.25898740864));
#21400=CARTESIAN_POINT('Ctrl Pts',(-1.015482192511,0.5750263216907,-30.55656011828));
#21401=CARTESIAN_POINT('Ctrl Pts',(-0.8824095367636,0.8100293243789,-30.57497594566));
#21402=CARTESIAN_POINT('Ctrl Pts',(-0.4470880869402,1.18276829068,-30.61180760041));
#21403=CARTESIAN_POINT('Ctrl Pts',(0.4133389835427,1.195144688561,-30.66705508253));
#21404=CARTESIAN_POINT('Ctrl Pts',(1.082287319525,0.6540128508907,-30.72230256466));
#21405=CARTESIAN_POINT('Ctrl Pts',(1.250228977982,-0.189832146326,-30.77755004678));
#21406=CARTESIAN_POINT('Ctrl Pts',(0.8393735447346,-0.945811051386,-30.83279752891));
#21407=CARTESIAN_POINT('Ctrl Pts',(0.03993616735796,-1.263926564634,-30.88804501103));
#21408=CARTESIAN_POINT('Ctrl Pts',(-0.7779901316111,-0.9969138795045,-30.94329249316));
#21409=CARTESIAN_POINT('Ctrl Pts',(-1.235749089843,-0.2683839185767,-30.99853997528));
#21410=CARTESIAN_POINT('Ctrl Pts',(-1.121423396098,0.5843931352325,-31.05378745741));
#21411=CARTESIAN_POINT('Ctrl Pts',(-0.4879395772335,1.166627935668,-31.10903493953));
#21412=CARTESIAN_POINT('Ctrl Pts',(0.3714337559552,1.208777371376,-31.16428242166));
#21413=CARTESIAN_POINT('Ctrl Pts',(1.058853438626,0.691328550783,-31.21952990378));
#21414=CARTESIAN_POINT('Ctrl Pts',(1.256081499646,-0.1461678338278,-31.27477738591));
#21415=CARTESIAN_POINT('Ctrl Pts',(0.8718120611923,-0.9159964516181,-31.33002486803));
#21416=CARTESIAN_POINT('Ctrl Pts',(0.08394099831018,-1.261768472513,-31.38527235016));
#21417=CARTESIAN_POINT('Ctrl Pts',(-0.7427901868119,-1.023410234361,-31.44051983228));
#21418=CARTESIAN_POINT('Ctrl Pts',(-1.225649866438,-0.3112686529751,-31.4957673144));
#21419=CARTESIAN_POINT('Ctrl Pts',(-1.141100239542,0.5449734055297,-31.55101479653));
#21420=CARTESIAN_POINT('Ctrl Pts',(-0.5282831903702,1.148922382135,-31.60626227865));
#21421=CARTESIAN_POINT('Ctrl Pts',(0.3291002778155,1.220982709444,-31.66150976078));
#21422=CARTESIAN_POINT('Ctrl Pts',(1.034128194939,0.7277943700298,-31.7167572429));
#21423=CARTESIAN_POINT('Ctrl Pts',(1.260410936535,-0.1023232250025,-31.77200472503));
#21424=CARTESIAN_POINT('Ctrl Pts',(0.9031918799483,-0.8850707304042,-31.82725220715));
#21425=CARTESIAN_POINT('Ctrl Pts',(0.1278440645328,-1.258078549202,-31.88249968928));
#21426=CARTESIAN_POINT('Ctrl Pts',(-0.7066886712758,-1.048664412443,-31.9377471714));
#21427=CARTESIAN_POINT('Ctrl Pts',(-1.214062705292,-0.3537753607434,-31.99299465353));
#21428=CARTESIAN_POINT('Ctrl Pts',(-1.159392542789,0.5048914975012,-32.04824213565));
#21429=CARTESIAN_POINT('Ctrl Pts',(-0.5679833167426,1.129824629341,-32.10348961778));
#21430=CARTESIAN_POINT('Ctrl Pts',(0.2863590197545,1.23169686325,-32.1587370999));
#21431=CARTESIAN_POINT('Ctrl Pts',(1.008178628936,0.7634106326662,-32.21398458203));
#21432=CARTESIAN_POINT('Ctrl Pts',(1.263094839915,-0.05848087125908,-32.26923206415));
#21433=CARTESIAN_POINT('Ctrl Pts',(1.043636050887,-0.5878927540068,-32.3060637189));
#21434=CARTESIAN_POINT('Ctrl Pts',(0.8614506246688,-0.7872497540188,-32.32447954628));
#21435=CARTESIAN_POINT('Ctrl Pts',(-1.015482192511,0.5750263216907,-30.62205225592));
#21436=CARTESIAN_POINT('Ctrl Pts',(-0.8824095367636,0.8100293243789,-30.6404680833));
#21437=CARTESIAN_POINT('Ctrl Pts',(-0.4470880869402,1.18276829068,-30.67729973805));
#21438=CARTESIAN_POINT('Ctrl Pts',(0.4133389835427,1.195144688561,-30.73254722017));
#21439=CARTESIAN_POINT('Ctrl Pts',(1.082287319525,0.6540128508907,-30.7877947023));
#21440=CARTESIAN_POINT('Ctrl Pts',(1.250228977982,-0.189832146326,-30.84304218442));
#21441=CARTESIAN_POINT('Ctrl Pts',(0.8393735447346,-0.945811051386,-30.89828966655));
#21442=CARTESIAN_POINT('Ctrl Pts',(0.03993616735796,-1.263926564634,-30.95353714867));
#21443=CARTESIAN_POINT('Ctrl Pts',(-0.7779901316111,-0.9969138795045,-31.0087846308));
#21444=CARTESIAN_POINT('Ctrl Pts',(-1.235749089843,-0.2683839185767,-31.06403211292));
#21445=CARTESIAN_POINT('Ctrl Pts',(-1.121423396098,0.5843931352325,-31.11927959505));
#21446=CARTESIAN_POINT('Ctrl Pts',(-0.4879395772335,1.166627935668,-31.17452707717));
#21447=CARTESIAN_POINT('Ctrl Pts',(0.3714337559552,1.208777371376,-31.2297745593));
#21448=CARTESIAN_POINT('Ctrl Pts',(1.058853438626,0.691328550783,-31.28502204142));
#21449=CARTESIAN_POINT('Ctrl Pts',(1.256081499646,-0.1461678338278,-31.34026952355));
#21450=CARTESIAN_POINT('Ctrl Pts',(0.8718120611923,-0.9159964516181,-31.39551700567));
#21451=CARTESIAN_POINT('Ctrl Pts',(0.08394099831018,-1.261768472513,-31.4507644878));
#21452=CARTESIAN_POINT('Ctrl Pts',(-0.7427901868119,-1.023410234361,-31.50601196992));
#21453=CARTESIAN_POINT('Ctrl Pts',(-1.225649866438,-0.3112686529751,-31.56125945205));
#21454=CARTESIAN_POINT('Ctrl Pts',(-1.141100239542,0.5449734055297,-31.61650693417));
#21455=CARTESIAN_POINT('Ctrl Pts',(-0.5282831903702,1.148922382135,-31.6717544163));
#21456=CARTESIAN_POINT('Ctrl Pts',(0.3291002778155,1.220982709444,-31.72700189842));
#21457=CARTESIAN_POINT('Ctrl Pts',(1.034128194939,0.7277943700298,-31.78224938055));
#21458=CARTESIAN_POINT('Ctrl Pts',(1.260410936535,-0.1023232250025,-31.83749686267));
#21459=CARTESIAN_POINT('Ctrl Pts',(0.9031918799483,-0.8850707304042,-31.8927443448));
#21460=CARTESIAN_POINT('Ctrl Pts',(0.1278440645328,-1.258078549202,-31.94799182692));
#21461=CARTESIAN_POINT('Ctrl Pts',(-0.7066886712758,-1.048664412443,-32.00323930904));
#21462=CARTESIAN_POINT('Ctrl Pts',(-1.214062705292,-0.3537753607434,-32.05848679117));
#21463=CARTESIAN_POINT('Ctrl Pts',(-1.159392542789,0.5048914975012,-32.11373427329));
#21464=CARTESIAN_POINT('Ctrl Pts',(-0.5679833167426,1.129824629341,-32.16898175542));
#21465=CARTESIAN_POINT('Ctrl Pts',(0.2863590197545,1.23169686325,-32.22422923754));
#21466=CARTESIAN_POINT('Ctrl Pts',(1.008178628936,0.7634106326662,-32.27947671967));
#21467=CARTESIAN_POINT('Ctrl Pts',(1.263094839915,-0.05848087125908,-32.33472420179));
#21468=CARTESIAN_POINT('Ctrl Pts',(1.043636050887,-0.5878927540068,-32.37155585654));
#21469=CARTESIAN_POINT('Ctrl Pts',(0.8614506246688,-0.7872497540188,-32.38997168392));
#21470=CARTESIAN_POINT('',(-0.6859379234404,0.9441125563889,-30.50007747308));
#21471=CARTESIAN_POINT('Ctrl Pts',(1.155855903054,0.1607995190315,-28.62357429354));
#21472=CARTESIAN_POINT('Ctrl Pts',(1.195258896894,-0.1224362972325,-28.64307429354));
#21473=CARTESIAN_POINT('Ctrl Pts',(1.056077145856,-0.7175033572827,-28.68207429354));
#21474=CARTESIAN_POINT('Ctrl Pts',(0.3019967923042,-1.240748778247,-28.74057429354));
#21475=CARTESIAN_POINT('Ctrl Pts',(-0.6081163618214,-1.122792874227,-28.79907429354));
#21476=CARTESIAN_POINT('Ctrl Pts',(-1.204114952344,-0.4249855149138,-28.85757429354));
#21477=CARTESIAN_POINT('Ctrl Pts',(-1.178171694542,0.49235784776,-28.91607429354));
#21478=CARTESIAN_POINT('Ctrl Pts',(-0.5436824759227,1.155383851922,-28.97457429354));
#21479=CARTESIAN_POINT('Ctrl Pts',(0.3716274479098,1.221636807823,-29.03307429354));
#21480=CARTESIAN_POINT('Ctrl Pts',(1.094985744155,0.6568937894785,-29.09157429354));
#21481=CARTESIAN_POINT('Ctrl Pts',(1.252765868871,-0.2471455563325,-29.15007429354));
#21482=CARTESIAN_POINT('Ctrl Pts',(0.7634718132616,-1.023530188774,-29.20857429354));
#21483=CARTESIAN_POINT('Ctrl Pts',(-0.1201679976972,-1.271244628134,-29.26707429354));
#21484=CARTESIAN_POINT('Ctrl Pts',(-0.9417390602074,-0.8623403017182,-29.32557429354));
#21485=CARTESIAN_POINT('Ctrl Pts',(-1.276886402343,-0.008023019429936,-29.38407429354));
#21486=CARTESIAN_POINT('Ctrl Pts',(-0.9525009070881,0.850438284238,-29.44257429354));
#21487=CARTESIAN_POINT('Ctrl Pts',(-0.1361330203811,1.269634220587,-29.50107429354));
#21488=CARTESIAN_POINT('Ctrl Pts',(0.7505498113574,1.033043190765,-29.55957429354));
#21489=CARTESIAN_POINT('Ctrl Pts',(1.249561315594,0.262868354685,-29.61807429354));
#21490=CARTESIAN_POINT('Ctrl Pts',(1.103153839379,-0.6430823119665,-29.67657429354));
#21491=CARTESIAN_POINT('Ctrl Pts',(0.3869492533009,-1.216870382867,-29.73507429354));
#21492=CARTESIAN_POINT('Ctrl Pts',(-0.5291209893422,-1.162124878025,-29.79357429354));
#21493=CARTESIAN_POINT('Ctrl Pts',(-1.171891533923,-0.5071227513611,-29.85207429354));
#21494=CARTESIAN_POINT('Ctrl Pts',(-1.209360820682,0.4098166204233,-29.91057429354));
#21495=CARTESIAN_POINT('Ctrl Pts',(-0.6221753352776,1.115078965991,-29.96907429354));
#21496=CARTESIAN_POINT('Ctrl Pts',(0.2863739154552,1.244384671677,-30.02757429354));
#21497=CARTESIAN_POINT('Ctrl Pts',(1.047006449646,0.7309452405402,-30.08607429354));
#21498=CARTESIAN_POINT('Ctrl Pts',(1.266842465797,-0.1600395162514,-30.14457429354));
#21499=CARTESIAN_POINT('Ctrl Pts',(0.8323352153661,-0.9683609251365,-30.20307429354));
#21500=CARTESIAN_POINT('Ctrl Pts',(-0.03209325983472,-1.276509118266,-30.26157429354));
#21501=CARTESIAN_POINT('Ctrl Pts',(-0.8799211891228,-0.9253151078751,-30.32007429354));
#21502=CARTESIAN_POINT('Ctrl Pts',(-1.273344351706,-0.09619644100725,-30.37857429354));
#21503=CARTESIAN_POINT('Ctrl Pts',(-1.008732028848,0.7826683203553,-30.43707429354));
#21504=CARTESIAN_POINT('Ctrl Pts',(-0.485799150132,1.098923865977,-30.47607429354));
#21505=CARTESIAN_POINT('Ctrl Pts',(-0.2042496867001,1.148974072566,-30.49557429354));
#21506=CARTESIAN_POINT('Ctrl Pts',(1.155855903054,0.1607995190315,-28.68906643118));
#21507=CARTESIAN_POINT('Ctrl Pts',(1.195258896894,-0.1224362972325,-28.70856643118));
#21508=CARTESIAN_POINT('Ctrl Pts',(1.056077145856,-0.7175033572827,-28.74756643118));
#21509=CARTESIAN_POINT('Ctrl Pts',(0.3019967923042,-1.240748778247,-28.80606643118));
#21510=CARTESIAN_POINT('Ctrl Pts',(-0.6081163618214,-1.122792874227,-28.86456643118));
#21511=CARTESIAN_POINT('Ctrl Pts',(-1.204114952344,-0.4249855149138,-28.92306643118));
#21512=CARTESIAN_POINT('Ctrl Pts',(-1.178171694542,0.49235784776,-28.98156643118));
#21513=CARTESIAN_POINT('Ctrl Pts',(-0.5436824759227,1.155383851922,-29.04006643118));
#21514=CARTESIAN_POINT('Ctrl Pts',(0.3716274479098,1.221636807823,-29.09856643118));
#21515=CARTESIAN_POINT('Ctrl Pts',(1.094985744155,0.6568937894785,-29.15706643118));
#21516=CARTESIAN_POINT('Ctrl Pts',(1.252765868871,-0.2471455563325,-29.21556643118));
#21517=CARTESIAN_POINT('Ctrl Pts',(0.7634718132616,-1.023530188774,-29.27406643118));
#21518=CARTESIAN_POINT('Ctrl Pts',(-0.1201679976972,-1.271244628134,-29.33256643118));
#21519=CARTESIAN_POINT('Ctrl Pts',(-0.9417390602074,-0.8623403017182,-29.39106643118));
#21520=CARTESIAN_POINT('Ctrl Pts',(-1.276886402343,-0.008023019429936,-29.44956643118));
#21521=CARTESIAN_POINT('Ctrl Pts',(-0.9525009070881,0.850438284238,-29.50806643118));
#21522=CARTESIAN_POINT('Ctrl Pts',(-0.1361330203811,1.269634220587,-29.56656643118));
#21523=CARTESIAN_POINT('Ctrl Pts',(0.7505498113574,1.033043190765,-29.62506643118));
#21524=CARTESIAN_POINT('Ctrl Pts',(1.249561315594,0.262868354685,-29.68356643118));
#21525=CARTESIAN_POINT('Ctrl Pts',(1.103153839379,-0.6430823119665,-29.74206643118));
#21526=CARTESIAN_POINT('Ctrl Pts',(0.3869492533009,-1.216870382867,-29.80056643118));
#21527=CARTESIAN_POINT('Ctrl Pts',(-0.5291209893422,-1.162124878025,-29.85906643118));
#21528=CARTESIAN_POINT('Ctrl Pts',(-1.171891533923,-0.5071227513611,-29.91756643118));
#21529=CARTESIAN_POINT('Ctrl Pts',(-1.209360820682,0.4098166204233,-29.97606643118));
#21530=CARTESIAN_POINT('Ctrl Pts',(-0.6221753352776,1.115078965991,-30.03456643118));
#21531=CARTESIAN_POINT('Ctrl Pts',(0.2863739154552,1.244384671677,-30.09306643118));
#21532=CARTESIAN_POINT('Ctrl Pts',(1.047006449646,0.7309452405402,-30.15156643118));
#21533=CARTESIAN_POINT('Ctrl Pts',(1.266842465797,-0.1600395162514,-30.21006643118));
#21534=CARTESIAN_POINT('Ctrl Pts',(0.8323352153661,-0.9683609251365,-30.26856643118));
#21535=CARTESIAN_POINT('Ctrl Pts',(-0.03209325983472,-1.276509118266,-30.32706643118));
#21536=CARTESIAN_POINT('Ctrl Pts',(-0.8799211891228,-0.9253151078751,-30.38556643118));
#21537=CARTESIAN_POINT('Ctrl Pts',(-1.273344351706,-0.09619644100725,-30.44406643118));
#21538=CARTESIAN_POINT('Ctrl Pts',(-1.008732028848,0.7826683203553,-30.50256643118));
#21539=CARTESIAN_POINT('Ctrl Pts',(-0.485799150132,1.098923865977,-30.54156643118));
#21540=CARTESIAN_POINT('Ctrl Pts',(-0.2042496867001,1.148974072566,-30.56106643118));
#21541=CARTESIAN_POINT('Ctrl Pts',(1.155855903054,0.1607995190315,-28.75455856882));
#21542=CARTESIAN_POINT('Ctrl Pts',(1.195258896894,-0.1224362972325,-28.77405856882));
#21543=CARTESIAN_POINT('Ctrl Pts',(1.056077145856,-0.7175033572827,-28.81305856882));
#21544=CARTESIAN_POINT('Ctrl Pts',(0.3019967923042,-1.240748778247,-28.87155856882));
#21545=CARTESIAN_POINT('Ctrl Pts',(-0.6081163618214,-1.122792874227,-28.93005856882));
#21546=CARTESIAN_POINT('Ctrl Pts',(-1.204114952344,-0.4249855149138,-28.98855856882));
#21547=CARTESIAN_POINT('Ctrl Pts',(-1.178171694542,0.49235784776,-29.04705856882));
#21548=CARTESIAN_POINT('Ctrl Pts',(-0.5436824759227,1.155383851922,-29.10555856882));
#21549=CARTESIAN_POINT('Ctrl Pts',(0.3716274479098,1.221636807823,-29.16405856882));
#21550=CARTESIAN_POINT('Ctrl Pts',(1.094985744155,0.6568937894785,-29.22255856882));
#21551=CARTESIAN_POINT('Ctrl Pts',(1.252765868871,-0.2471455563325,-29.28105856882));
#21552=CARTESIAN_POINT('Ctrl Pts',(0.7634718132616,-1.023530188774,-29.33955856882));
#21553=CARTESIAN_POINT('Ctrl Pts',(-0.1201679976972,-1.271244628134,-29.39805856882));
#21554=CARTESIAN_POINT('Ctrl Pts',(-0.9417390602074,-0.8623403017182,-29.45655856882));
#21555=CARTESIAN_POINT('Ctrl Pts',(-1.276886402343,-0.008023019429936,-29.51505856882));
#21556=CARTESIAN_POINT('Ctrl Pts',(-0.9525009070881,0.850438284238,-29.57355856882));
#21557=CARTESIAN_POINT('Ctrl Pts',(-0.1361330203811,1.269634220587,-29.63205856882));
#21558=CARTESIAN_POINT('Ctrl Pts',(0.7505498113574,1.033043190765,-29.69055856882));
#21559=CARTESIAN_POINT('Ctrl Pts',(1.249561315594,0.262868354685,-29.74905856882));
#21560=CARTESIAN_POINT('Ctrl Pts',(1.103153839379,-0.6430823119665,-29.80755856882));
#21561=CARTESIAN_POINT('Ctrl Pts',(0.3869492533009,-1.216870382867,-29.86605856882));
#21562=CARTESIAN_POINT('Ctrl Pts',(-0.5291209893422,-1.162124878025,-29.92455856882));
#21563=CARTESIAN_POINT('Ctrl Pts',(-1.171891533923,-0.5071227513611,-29.98305856882));
#21564=CARTESIAN_POINT('Ctrl Pts',(-1.209360820682,0.4098166204233,-30.04155856882));
#21565=CARTESIAN_POINT('Ctrl Pts',(-0.6221753352776,1.115078965991,-30.10005856882));
#21566=CARTESIAN_POINT('Ctrl Pts',(0.2863739154552,1.244384671677,-30.15855856882));
#21567=CARTESIAN_POINT('Ctrl Pts',(1.047006449646,0.7309452405402,-30.21705856882));
#21568=CARTESIAN_POINT('Ctrl Pts',(1.266842465797,-0.1600395162514,-30.27555856882));
#21569=CARTESIAN_POINT('Ctrl Pts',(0.8323352153661,-0.9683609251365,-30.33405856882));
#21570=CARTESIAN_POINT('Ctrl Pts',(-0.03209325983472,-1.276509118266,-30.39255856882));
#21571=CARTESIAN_POINT('Ctrl Pts',(-0.8799211891228,-0.9253151078751,-30.45105856882));
#21572=CARTESIAN_POINT('Ctrl Pts',(-1.273344351706,-0.09619644100725,-30.50955856882));
#21573=CARTESIAN_POINT('Ctrl Pts',(-1.008732028848,0.7826683203553,-30.56805856882));
#21574=CARTESIAN_POINT('Ctrl Pts',(-0.485799150132,1.098923865977,-30.60705856882));
#21575=CARTESIAN_POINT('Ctrl Pts',(-0.2042496867001,1.148974072566,-30.62655856882));
#21576=CARTESIAN_POINT('Ctrl Pts',(1.155855903054,0.1607995190315,-28.82005070646));
#21577=CARTESIAN_POINT('Ctrl Pts',(1.195258896894,-0.1224362972325,-28.83955070646));
#21578=CARTESIAN_POINT('Ctrl Pts',(1.056077145856,-0.7175033572827,-28.87855070646));
#21579=CARTESIAN_POINT('Ctrl Pts',(0.3019967923042,-1.240748778247,-28.93705070646));
#21580=CARTESIAN_POINT('Ctrl Pts',(-0.6081163618214,-1.122792874227,-28.99555070646));
#21581=CARTESIAN_POINT('Ctrl Pts',(-1.204114952344,-0.4249855149138,-29.05405070646));
#21582=CARTESIAN_POINT('Ctrl Pts',(-1.178171694542,0.49235784776,-29.11255070646));
#21583=CARTESIAN_POINT('Ctrl Pts',(-0.5436824759227,1.155383851922,-29.17105070646));
#21584=CARTESIAN_POINT('Ctrl Pts',(0.3716274479098,1.221636807823,-29.22955070646));
#21585=CARTESIAN_POINT('Ctrl Pts',(1.094985744155,0.6568937894785,-29.28805070646));
#21586=CARTESIAN_POINT('Ctrl Pts',(1.252765868871,-0.2471455563325,-29.34655070646));
#21587=CARTESIAN_POINT('Ctrl Pts',(0.7634718132616,-1.023530188774,-29.40505070646));
#21588=CARTESIAN_POINT('Ctrl Pts',(-0.1201679976972,-1.271244628134,-29.46355070646));
#21589=CARTESIAN_POINT('Ctrl Pts',(-0.9417390602074,-0.8623403017182,-29.52205070646));
#21590=CARTESIAN_POINT('Ctrl Pts',(-1.276886402343,-0.008023019429936,-29.58055070646));
#21591=CARTESIAN_POINT('Ctrl Pts',(-0.9525009070881,0.850438284238,-29.63905070646));
#21592=CARTESIAN_POINT('Ctrl Pts',(-0.1361330203811,1.269634220587,-29.69755070646));
#21593=CARTESIAN_POINT('Ctrl Pts',(0.7505498113574,1.033043190765,-29.75605070646));
#21594=CARTESIAN_POINT('Ctrl Pts',(1.249561315594,0.262868354685,-29.81455070646));
#21595=CARTESIAN_POINT('Ctrl Pts',(1.103153839379,-0.6430823119665,-29.87305070646));
#21596=CARTESIAN_POINT('Ctrl Pts',(0.3869492533009,-1.216870382867,-29.93155070646));
#21597=CARTESIAN_POINT('Ctrl Pts',(-0.5291209893422,-1.162124878025,-29.99005070646));
#21598=CARTESIAN_POINT('Ctrl Pts',(-1.171891533923,-0.5071227513611,-30.04855070646));
#21599=CARTESIAN_POINT('Ctrl Pts',(-1.209360820682,0.4098166204233,-30.10705070646));
#21600=CARTESIAN_POINT('Ctrl Pts',(-0.6221753352776,1.115078965991,-30.16555070646));
#21601=CARTESIAN_POINT('Ctrl Pts',(0.2863739154552,1.244384671677,-30.22405070646));
#21602=CARTESIAN_POINT('Ctrl Pts',(1.047006449646,0.7309452405402,-30.28255070646));
#21603=CARTESIAN_POINT('Ctrl Pts',(1.266842465797,-0.1600395162514,-30.34105070646));
#21604=CARTESIAN_POINT('Ctrl Pts',(0.8323352153661,-0.9683609251365,-30.39955070646));
#21605=CARTESIAN_POINT('Ctrl Pts',(-0.03209325983472,-1.276509118266,-30.45805070646));
#21606=CARTESIAN_POINT('Ctrl Pts',(-0.8799211891228,-0.9253151078751,-30.51655070646));
#21607=CARTESIAN_POINT('Ctrl Pts',(-1.273344351706,-0.09619644100725,-30.57505070646));
#21608=CARTESIAN_POINT('Ctrl Pts',(-1.008732028848,0.7826683203553,-30.63355070646));
#21609=CARTESIAN_POINT('Ctrl Pts',(-0.485799150132,1.098923865977,-30.67255070646));
#21610=CARTESIAN_POINT('Ctrl Pts',(-0.2042496867001,1.148974072566,-30.69205070646));
#21611=CARTESIAN_POINT('',(1.10987074412979,-0.360618865453563,-28.7000774755696));
#21612=CARTESIAN_POINT('',(1.10987074420186,-0.360618865445946,-28.8155475173803));
#21613=CARTESIAN_POINT('',(1.109870874299,-0.360618907335,-28.70007747308));
#21614=CARTESIAN_POINT('Ctrl Pts',(1.10908833794556,-0.360366944018243,
-28.8155263221856));
#21615=CARTESIAN_POINT('Ctrl Pts',(1.08313436609586,-0.440796138886377,
-28.821289639903));
#21616=CARTESIAN_POINT('Ctrl Pts',(1.04860768641626,-0.518475529758915,
-28.8270583193288));
#21617=CARTESIAN_POINT('Ctrl Pts',(0.962822718320563,-0.665102822246014,
-28.8386648185783));
#21618=CARTESIAN_POINT('Ctrl Pts',(0.911877589687252,-0.732889579139993,
-28.8444246367459));
#21619=CARTESIAN_POINT('Ctrl Pts',(0.749526335843727,-0.906069987879671,
-28.8606247655878));
#21620=CARTESIAN_POINT('Ctrl Pts',(0.622881803069167,-0.997235485886477,
-28.8710522198585));
#21621=CARTESIAN_POINT('Ctrl Pts',(0.343528450555899,-1.12590745534022,
-28.8920310449809));
#21622=CARTESIAN_POINT('Ctrl Pts',(0.194312135562372,-1.16089704614948,
-28.902302863744));
#21623=CARTESIAN_POINT('Ctrl Pts',(-0.111156106659192,-1.17034442347986,
-28.9231468506276));
#21624=CARTESIAN_POINT('Ctrl Pts',(-0.26351142328336,-1.14592402246402,
-28.9334627805694));
#21625=CARTESIAN_POINT('Ctrl Pts',(-0.549326063249744,-1.04113475309189,
-28.9542375650596));
#21626=CARTESIAN_POINT('Ctrl Pts',(-0.677727411883004,-0.962092897939803,
-28.9643397811051));
#21627=CARTESIAN_POINT('Ctrl Pts',(-0.900820166818602,-0.754917089196826,
-28.9850966850868));
#21628=CARTESIAN_POINT('Ctrl Pts',(-0.991430863061421,-0.632184918383142,
-28.9953023673024));
#21629=CARTESIAN_POINT('Ctrl Pts',(-1.13130517516952,-0.337598251088518,
-29.0175666426254));
#21630=CARTESIAN_POINT('Ctrl Pts',(-1.15872514586492,-0.185091355530231,
-29.0279248529793));
#21631=CARTESIAN_POINT('Ctrl Pts',(-1.17156099735629,0.0915106406107147,
-29.0467982047518));
#21632=CARTESIAN_POINT('Ctrl Pts',(-1.15094021376635,0.240868634693148,
-29.0568916601283));
#21633=CARTESIAN_POINT('Ctrl Pts',(-1.04462445846178,0.551227615411852,
-29.079295860188));
#21634=CARTESIAN_POINT('Ctrl Pts',(-0.955273189774736,0.680414508389834,
-29.0897825979082));
#21635=CARTESIAN_POINT('Ctrl Pts',(-0.774838363480179,0.883314838060978,
-29.1082867322753));
#21636=CARTESIAN_POINT('Ctrl Pts',(-0.657401586964177,0.974985736585898,
-29.1182677916964));
#21637=CARTESIAN_POINT('Ctrl Pts',(-0.368344830676665,1.12174076584231,
-29.1404107238409));
#21638=CARTESIAN_POINT('Ctrl Pts',(-0.212531118107411,1.1535440042497,-29.1510273049902));
#21639=CARTESIAN_POINT('Ctrl Pts',(0.0594720124148806,1.17343886176816,
-29.1696126930078));
#21640=CARTESIAN_POINT('Ctrl Pts',(0.206305151023307,1.15779145978757,-29.1795125735436));
#21641=CARTESIAN_POINT('Ctrl Pts',(0.493566643319564,1.06879852693626,-29.2000550606956));
#21642=CARTESIAN_POINT('Ctrl Pts',(0.632274348520006,0.991765068167543,
-29.2106622296585));
#21643=CARTESIAN_POINT('Ctrl Pts',(0.843248468532097,0.814363861741664,
-29.2294473277748));
#21644=CARTESIAN_POINT('Ctrl Pts',(0.946872694845534,0.704265996517519,
-29.2395560462993));
#21645=CARTESIAN_POINT('Ctrl Pts',(1.10143556399852,0.414582166282669,-29.2619812077135));
#21646=CARTESIAN_POINT('Ctrl Pts',(1.14628465443798,0.262803931594675,-29.272558053066));
#21647=CARTESIAN_POINT('Ctrl Pts',(1.17306196823584,-0.0177920846726822,
-29.2917705495727));
#21648=CARTESIAN_POINT('Ctrl Pts',(1.16777374859159,-0.169443851360727,
-29.301923080837));
#21649=CARTESIAN_POINT('Ctrl Pts',(1.07311149596804,-0.482141027412294,
-29.324229282871));
#21650=CARTESIAN_POINT('Ctrl Pts',(0.998645675280905,-0.620862503467565,
-29.3347495650282));
#21651=CARTESIAN_POINT('Ctrl Pts',(0.802434704990753,-0.861103744062571,
-29.3558983763231));
#21652=CARTESIAN_POINT('Ctrl Pts',(0.686156399960789,-0.956092045564658,
-29.3659604824618));
#21653=CARTESIAN_POINT('Ctrl Pts',(0.418179775124533,-1.09915266243817,
-29.3866904752757));
#21654=CARTESIAN_POINT('Ctrl Pts',(0.268798826463745,-1.14470235742467,
-29.3971268139701));
#21655=CARTESIAN_POINT('Ctrl Pts',(-0.0370622684688421,-1.17652270127989,
-29.4181021416964));
#21656=CARTESIAN_POINT('Ctrl Pts',(-0.189446380573865,-1.16172356518029,
-29.4283633413594));
#21657=CARTESIAN_POINT('Ctrl Pts',(-0.48191823722687,-1.07231208588559,
-29.4492232952251));
#21658=CARTESIAN_POINT('Ctrl Pts',(-0.618455614369153,-1.00003027230851,
-29.4595514605357));
#21659=CARTESIAN_POINT('Ctrl Pts',(-0.854289106561804,-0.809574565893422,
-29.4802380394371));
#21660=CARTESIAN_POINT('Ctrl Pts',(-0.950818687642285,-0.693822895932136,
-29.4903371103176));
#21661=CARTESIAN_POINT('Ctrl Pts',(-1.09602778432127,-0.424466988073746,
-29.5112005351714));
#21662=CARTESIAN_POINT('Ctrl Pts',(-1.14228730776674,-0.278868611711132,
-29.5214196096766));
#21663=CARTESIAN_POINT('Ctrl Pts',(-1.17969101994448,0.0449548978083805,
-29.5436737563468));
#21664=CARTESIAN_POINT('Ctrl Pts',(-1.15666344894799,0.197955069125265,
-29.5540179844193));
#21665=CARTESIAN_POINT('Ctrl Pts',(-1.07946856224424,0.464460329139435,
-29.5729300210825));
#21666=CARTESIAN_POINT('Ctrl Pts',(-1.01165109460015,0.599360219704604,
-29.5830368577589));
#21667=CARTESIAN_POINT('Ctrl Pts',(-0.811053751559631,0.858554997261858,
-29.6054191523544));
#21668=CARTESIAN_POINT('Ctrl Pts',(-0.685118451514117,0.951996193221799,
-29.6158902244773));
#21669=CARTESIAN_POINT('Ctrl Pts',(-0.448246304615079,1.08615128492057,
-29.6344423045363));
#21670=CARTESIAN_POINT('Ctrl Pts',(-0.307294849336651,1.1350476484419,-29.6444366233427));
#21671=CARTESIAN_POINT('Ctrl Pts',(0.0292016419244714,1.18278509811256,
-29.667650805626));
#21672=CARTESIAN_POINT('Ctrl Pts',(0.189862921386255,1.15554169754149,-29.6784973022942));
#21673=CARTESIAN_POINT('Ctrl Pts',(0.435078569175385,1.09139610098499,-29.6957700105568));
#21674=CARTESIAN_POINT('Ctrl Pts',(0.568753885931893,1.02925174324196,-29.7056531858431));
#21675=CARTESIAN_POINT('Ctrl Pts',(0.8031219609487,0.858973369535551,-29.7254418679969));
#21676=CARTESIAN_POINT('Ctrl Pts',(0.903532701937408,0.751044251113621,
-29.7353250432866));
#21677=CARTESIAN_POINT('Ctrl Pts',(1.04031459198797,0.53765239083601,-29.7525977515492));
#21678=CARTESIAN_POINT('Ctrl Pts',(1.11587167131851,0.393273107848723,-29.7634442482175));
#21679=CARTESIAN_POINT('Ctrl Pts',(1.17445379308505,0.0584942439088353,
-29.7866584305008));
#21680=CARTESIAN_POINT('Ctrl Pts',(1.17150698299789,-0.090668363406152,
-29.7966527493071));
#21681=CARTESIAN_POINT('Ctrl Pts',(1.11711542772956,-0.357403365460144,
-29.8152048293661));
#21682=CARTESIAN_POINT('Ctrl Pts',(1.06716371732723,-0.506049870726462,
-29.8256759014888));
#21683=CARTESIAN_POINT('Ctrl Pts',(0.882642823167696,-0.776924872095253,
-29.8480581960844));
#21684=CARTESIAN_POINT('Ctrl Pts',(0.77530215321567,-0.883109475340823,
-29.858165032761));
#21685=CARTESIAN_POINT('Ctrl Pts',(0.545695120922613,-1.03888082979983,
-29.8770770694243));
#21686=CARTESIAN_POINT('Ctrl Pts',(0.407299221774572,-1.10806100432971,
-29.8874212974969));
#21687=CARTESIAN_POINT('Ctrl Pts',(0.0877663802010376,-1.17255492774913,
-29.9096754441671));
#21688=CARTESIAN_POINT('Ctrl Pts',(-0.0650008832968393,-1.17355187918509,
-29.9198945186722));
#21689=CARTESIAN_POINT('Ctrl Pts',(-0.366045653279394,-1.1186853746269,
-29.9407579435258));
#21690=CARTESIAN_POINT('Ctrl Pts',(-0.505961314281852,-1.06264952067055,
-29.9508570144062));
#21691=CARTESIAN_POINT('Ctrl Pts',(-0.75997201186392,-0.897212591118086,
-29.9715435933075));
#21692=CARTESIAN_POINT('Ctrl Pts',(-0.870908471580324,-0.78969413764874,
-29.9818717586181));
#21693=CARTESIAN_POINT('Ctrl Pts',(-1.04632261567737,-0.539166539140349,
-30.0027317124838));
#21694=CARTESIAN_POINT('Ctrl Pts',(-1.10748671081373,-0.39881382089982,
-30.0129929121468));
#21695=CARTESIAN_POINT('Ctrl Pts',(-1.17174004169197,-0.0980896064647566,
-30.0339682398731));
#21696=CARTESIAN_POINT('Ctrl Pts',(-1.17458095923193,0.0580557480089826,
-30.0444045785676));
#21697=CARTESIAN_POINT('Ctrl Pts',(-1.12133155849895,0.357124825114059,
-30.0651345713814));
#21698=CARTESIAN_POINT('Ctrl Pts',(-1.06692428771505,0.497065064247616,
-30.0751966775202));
#21699=CARTESIAN_POINT('Ctrl Pts',(-0.899073814666865,0.757911412204312,
-30.0963454888149));
#21700=CARTESIAN_POINT('Ctrl Pts',(-0.790153055006947,0.871599909795869,
-30.106865770972));
#21701=CARTESIAN_POINT('Ctrl Pts',(-0.522012612882802,1.05825780349354,
-30.1291719730058));
#21702=CARTESIAN_POINT('Ctrl Pts',(-0.379417361706689,1.11015017237935,
-30.1393245042701));
#21703=CARTESIAN_POINT('Ctrl Pts',(-0.104280046962064,1.17139237118361,
-30.1585370007769));
#21704=CARTESIAN_POINT('Ctrl Pts',(0.0539287632978188,1.17564040536612,
-30.1691138461296));
#21705=CARTESIAN_POINT('Ctrl Pts',(0.377197010975913,1.11815960801923,-30.1915390075439));
#21706=CARTESIAN_POINT('Ctrl Pts',(0.513927950087521,1.05362922373646,-30.2016477260683));
#21707=CARTESIAN_POINT('Ctrl Pts',(0.747841111914739,0.907800899737522,
-30.2204328241846));
#21708=CARTESIAN_POINT('Ctrl Pts',(0.863967323007234,0.799686680741337,
-30.2310399931474));
#21709=CARTESIAN_POINT('Ctrl Pts',(1.03737331464879,0.553985095242687,-30.2515824802992));
#21710=CARTESIAN_POINT('Ctrl Pts',(1.09762881343296,0.419173795090948,-30.2614823608351));
#21711=CARTESIAN_POINT('Ctrl Pts',(1.16276126940395,0.154335596280972,-30.2800677488528));
#21712=CARTESIAN_POINT('Ctrl Pts',(1.18066367741776,-0.00367979153002535,
-30.2906843300022));
#21713=CARTESIAN_POINT('Ctrl Pts',(1.13041480057629,-0.323938901225899,
-30.3128272621468));
#21714=CARTESIAN_POINT('Ctrl Pts',(1.0795205548877,-0.463955778317749,-30.322808321568));
#21715=CARTESIAN_POINT('Ctrl Pts',(0.942308301897849,-0.69825914566429,
-30.3413124559352));
#21716=CARTESIAN_POINT('Ctrl Pts',(0.847055326004481,-0.823158197369145,
-30.3517991936555));
#21717=CARTESIAN_POINT('Ctrl Pts',(0.584739770160091,-1.02017668863557,
-30.3742033937154));
#21718=CARTESIAN_POINT('Ctrl Pts',(0.449064049193805,-1.0859423776572,-30.3842968490918));
#21719=CARTESIAN_POINT('Ctrl Pts',(0.18203342209547,-1.15920947493991,-30.4031702008643));
#21720=CARTESIAN_POINT('Ctrl Pts',(0.0285175083645084,-1.18025875562043,
-30.4135284112181));
#21721=CARTESIAN_POINT('Ctrl Pts',(-0.294874600697855,-1.13826266613818,
-30.4357926865411));
#21722=CARTESIAN_POINT('Ctrl Pts',(-0.439600076520489,-1.09001309956844,
-30.4459983687568));
#21723=CARTESIAN_POINT('Ctrl Pts',(-0.705575432041411,-0.941860126973679,
-30.4667552727384));
#21724=CARTESIAN_POINT('Ctrl Pts',(-0.820426902272153,-0.844168464163867,
-30.476857488784));
#21725=CARTESIAN_POINT('Ctrl Pts',(-1.00840900073706,-0.604724253435626,
-30.4976322732741));
#21726=CARTESIAN_POINT('Ctrl Pts',(-1.07871456427402,-0.467372055691353,
-30.5079482032156));
#21727=CARTESIAN_POINT('Ctrl Pts',(-1.16412445259043,-0.173935093258025,
-30.5287921900991));
#21728=CARTESIAN_POINT('Ctrl Pts',(-1.17695775141982,-0.0212095663596859,
-30.5390640088622));
#21729=CARTESIAN_POINT('Ctrl Pts',(-1.14090836976859,0.284233085157646,
-30.5600428339846));
#21730=CARTESIAN_POINT('Ctrl Pts',(-1.0933401417,0.432850881490686,-30.5704702882553));
#21731=CARTESIAN_POINT('Ctrl Pts',(-0.978811929812615,0.64075935756687,
-30.586669448521));
#21732=CARTESIAN_POINT('Ctrl Pts',(-0.930095050179522,0.710147925105241,
-30.5924283383721));
#21733=CARTESIAN_POINT('Ctrl Pts',(-0.817158328342888,0.837048290513652,
-30.6040347961641));
#21734=CARTESIAN_POINT('Ctrl Pts',(-0.753940956291978,0.893899707069815,
-30.6098044000168));
#21735=CARTESIAN_POINT('Ctrl Pts',(-0.685457562470264,0.943445394325056,
-30.6155686401302));
#21736=CARTESIAN_POINT('Ctrl Pts',(1.10908828377812,-0.360367111878588,
-28.7000562803704));
#21737=CARTESIAN_POINT('Ctrl Pts',(1.08313431805632,-0.440796246967518,
-28.705819594086));
#21738=CARTESIAN_POINT('Ctrl Pts',(1.04860765672726,-0.518475580504724,
-28.7115882695023));
#21739=CARTESIAN_POINT('Ctrl Pts',(0.96282271832024,-0.665102822246447,
-28.7231947647351));
#21740=CARTESIAN_POINT('Ctrl Pts',(0.91187758968706,-0.7328895791402,-28.7289545829027));
#21741=CARTESIAN_POINT('Ctrl Pts',(0.749526335843715,-0.90606998787968,
-28.7451547117448));
#21742=CARTESIAN_POINT('Ctrl Pts',(0.622881803069154,-0.997235485886485,
-28.7555821660155));
#21743=CARTESIAN_POINT('Ctrl Pts',(0.343528450555896,-1.12590745534022,
-28.7765609911379));
#21744=CARTESIAN_POINT('Ctrl Pts',(0.194312135562378,-1.16089704614948,
-28.7868328099008));
#21745=CARTESIAN_POINT('Ctrl Pts',(-0.111156106659175,-1.17034442347986,
-28.8076767967842));
#21746=CARTESIAN_POINT('Ctrl Pts',(-0.263511423283337,-1.14592402246402,
-28.8179927267257));
#21747=CARTESIAN_POINT('Ctrl Pts',(-0.549326063249702,-1.04113475309191,
-28.8387675112157));
#21748=CARTESIAN_POINT('Ctrl Pts',(-0.677727411882962,-0.962092897939833,
-28.8488697272613));
#21749=CARTESIAN_POINT('Ctrl Pts',(-0.900820166818571,-0.754917089196863,
-28.8696266312429));
#21750=CARTESIAN_POINT('Ctrl Pts',(-0.991430863061393,-0.632184918383185,
-28.8798323134585));
#21751=CARTESIAN_POINT('Ctrl Pts',(-1.13130517516951,-0.337598251088571,
-28.9020965887813));
#21752=CARTESIAN_POINT('Ctrl Pts',(-1.15872514586491,-0.185091355530289,
-28.9124547991351));
#21753=CARTESIAN_POINT('Ctrl Pts',(-1.17156099735629,0.091510640610664,
-28.9313281509076));
#21754=CARTESIAN_POINT('Ctrl Pts',(-1.15094021376636,0.240868634693107,
-28.9414216062841));
#21755=CARTESIAN_POINT('Ctrl Pts',(-1.0446244584618,0.551227615411831,-28.9638258063441));
#21756=CARTESIAN_POINT('Ctrl Pts',(-0.955273189774745,0.680414508389824,
-28.9743125440646));
#21757=CARTESIAN_POINT('Ctrl Pts',(-0.774838363480177,0.883314838060981,
-28.992816678432));
#21758=CARTESIAN_POINT('Ctrl Pts',(-0.657401586964166,0.974985736585907,
-29.0027977378534));
#21759=CARTESIAN_POINT('Ctrl Pts',(-0.36834483067665,1.12174076584231,-29.0249406699982));
#21760=CARTESIAN_POINT('Ctrl Pts',(-0.21253111810739,1.1535440042497,-29.0355572511477));
#21761=CARTESIAN_POINT('Ctrl Pts',(0.0594720124149227,1.17343886176816,
-29.0541426391653));
#21762=CARTESIAN_POINT('Ctrl Pts',(0.206305151023344,1.15779145978756,-29.0640425197011));
#21763=CARTESIAN_POINT('Ctrl Pts',(0.493566643319589,1.06879852693625,-29.0845850068529));
#21764=CARTESIAN_POINT('Ctrl Pts',(0.632274348520021,0.991765068167532,
-29.0951921758155));
#21765=CARTESIAN_POINT('Ctrl Pts',(0.843248468532104,0.814363861741656,
-29.1139772739316));
#21766=CARTESIAN_POINT('Ctrl Pts',(0.946872694845539,0.704265996517511,
-29.1240859924559));
#21767=CARTESIAN_POINT('Ctrl Pts',(1.10143556399853,0.414582166282656,-29.1465111538702));
#21768=CARTESIAN_POINT('Ctrl Pts',(1.14628465443799,0.262803931594657,-29.1570879992228));
#21769=CARTESIAN_POINT('Ctrl Pts',(1.17306196823584,-0.0177920846726962,
-29.1763004957296));
#21770=CARTESIAN_POINT('Ctrl Pts',(1.16777374859159,-0.169443851360738,
-29.186453026994));
#21771=CARTESIAN_POINT('Ctrl Pts',(1.07311149596803,-0.482141027412298,
-29.2087592290279));
#21772=CARTESIAN_POINT('Ctrl Pts',(0.998645675280905,-0.620862503467564,
-29.219279511185));
#21773=CARTESIAN_POINT('Ctrl Pts',(0.802434704990756,-0.861103744062567,
-29.2404283224797));
#21774=CARTESIAN_POINT('Ctrl Pts',(0.686156399960795,-0.956092045564654,
-29.2504904286183));
#21775=CARTESIAN_POINT('Ctrl Pts',(0.418179775124541,-1.09915266243817,
-29.2712204214321));
#21776=CARTESIAN_POINT('Ctrl Pts',(0.268798826463751,-1.14470235742467,
-29.2816567601266));
#21777=CARTESIAN_POINT('Ctrl Pts',(-0.0370622684688349,-1.17652270127989,
-29.3026320878529));
#21778=CARTESIAN_POINT('Ctrl Pts',(-0.189446380573858,-1.16172356518029,
-29.312893287516));
#21779=CARTESIAN_POINT('Ctrl Pts',(-0.481918237226863,-1.0723120858856,
-29.3337532413817));
#21780=CARTESIAN_POINT('Ctrl Pts',(-0.618455614369146,-1.00003027230852,
-29.3440814066923));
#21781=CARTESIAN_POINT('Ctrl Pts',(-0.854289106561791,-0.809574565893434,
-29.3647679855936));
#21782=CARTESIAN_POINT('Ctrl Pts',(-0.950818687642273,-0.693822895932154,
-29.374867056474));
#21783=CARTESIAN_POINT('Ctrl Pts',(-1.09602778432126,-0.424466988073762,
-29.3957304813277));
#21784=CARTESIAN_POINT('Ctrl Pts',(-1.14228730776674,-0.27886861171115,
-29.4059495558328));
#21785=CARTESIAN_POINT('Ctrl Pts',(-1.17969101994449,0.044954897808365,
-29.428203702503));
#21786=CARTESIAN_POINT('Ctrl Pts',(-1.15666344894799,0.197955069125252,
-29.4385479305756));
#21787=CARTESIAN_POINT('Ctrl Pts',(-1.07946856224424,0.464460329139423,
-29.4574599672389));
#21788=CARTESIAN_POINT('Ctrl Pts',(-1.01165109460016,0.599360219704595,
-29.4675668039155));
#21789=CARTESIAN_POINT('Ctrl Pts',(-0.811053751559636,0.858554997261854,
-29.4899490985111));
#21790=CARTESIAN_POINT('Ctrl Pts',(-0.685118451514121,0.951996193221797,
-29.5004201706339));
#21791=CARTESIAN_POINT('Ctrl Pts',(-0.448246304615079,1.08615128492057,
-29.5189722506929));
#21792=CARTESIAN_POINT('Ctrl Pts',(-0.307294849336651,1.1350476484419,-29.5289665694992));
#21793=CARTESIAN_POINT('Ctrl Pts',(0.0292016419244812,1.18278509811256,
-29.5521807517825));
#21794=CARTESIAN_POINT('Ctrl Pts',(0.189862921386267,1.15554169754148,-29.5630272484508));
#21795=CARTESIAN_POINT('Ctrl Pts',(0.435078569175386,1.09139610098499,-29.5802999567135));
#21796=CARTESIAN_POINT('Ctrl Pts',(0.568753885931894,1.02925174324196,-29.5901831320031));
#21797=CARTESIAN_POINT('Ctrl Pts',(0.803121960948698,0.858973369535553,
-29.6099718141569));
#21798=CARTESIAN_POINT('Ctrl Pts',(0.903532701937406,0.751044251113624,
-29.6198549894432));
#21799=CARTESIAN_POINT('Ctrl Pts',(1.04031459198799,0.537652390835985,-29.6371276977058));
#21800=CARTESIAN_POINT('Ctrl Pts',(1.11587167131852,0.393273107848698,-29.647974194374));
#21801=CARTESIAN_POINT('Ctrl Pts',(1.17445379308505,0.0584942439088389,
-29.6711883766573));
#21802=CARTESIAN_POINT('Ctrl Pts',(1.17150698299789,-0.0906683634061496,
-29.6811826954637));
#21803=CARTESIAN_POINT('Ctrl Pts',(1.11711542772956,-0.357403365460141,
-29.6997347755227));
#21804=CARTESIAN_POINT('Ctrl Pts',(1.06716371732723,-0.506049870726459,
-29.7102058476456));
#21805=CARTESIAN_POINT('Ctrl Pts',(0.882642823167698,-0.776924872095252,
-29.7325881422412));
#21806=CARTESIAN_POINT('Ctrl Pts',(0.775302153215673,-0.883109475340821,
-29.7426949789176));
#21807=CARTESIAN_POINT('Ctrl Pts',(0.545695120922612,-1.03888082979983,
-29.7616070155808));
#21808=CARTESIAN_POINT('Ctrl Pts',(0.407299221774572,-1.10806100432971,
-29.7719512436533));
#21809=CARTESIAN_POINT('Ctrl Pts',(0.0877663802010367,-1.17255492774913,
-29.7942053903235));
#21810=CARTESIAN_POINT('Ctrl Pts',(-0.0650008832968425,-1.17355187918509,
-29.8044244648287));
#21811=CARTESIAN_POINT('Ctrl Pts',(-0.366045653279393,-1.1186853746269,
-29.8252878896825));
#21812=CARTESIAN_POINT('Ctrl Pts',(-0.505961314281856,-1.06264952067055,
-29.835386960563));
#21813=CARTESIAN_POINT('Ctrl Pts',(-0.759972011863936,-0.897212591118072,
-29.8560735394644));
#21814=CARTESIAN_POINT('Ctrl Pts',(-0.870908471580342,-0.789694137648721,
-29.866401704775));
#21815=CARTESIAN_POINT('Ctrl Pts',(-1.04632261567739,-0.539166539140322,
-29.8872616586407));
#21816=CARTESIAN_POINT('Ctrl Pts',(-1.10748671081375,-0.398813820899789,
-29.8975228583038));
#21817=CARTESIAN_POINT('Ctrl Pts',(-1.17174004169197,-0.0980896064647195,
-29.9184981860302));
#21818=CARTESIAN_POINT('Ctrl Pts',(-1.17458095923193,0.0580557480090229,
-29.9289345247246));
#21819=CARTESIAN_POINT('Ctrl Pts',(-1.12133155849894,0.357124825114116,
-29.9496645175385));
#21820=CARTESIAN_POINT('Ctrl Pts',(-1.06692428771502,0.497065064247667,
-29.9597266236771));
#21821=CARTESIAN_POINT('Ctrl Pts',(-0.899073814666838,0.757911412204344,
-29.9808754349719));
#21822=CARTESIAN_POINT('Ctrl Pts',(-0.790153055006915,0.871599909795898,
-29.9913957171291));
#21823=CARTESIAN_POINT('Ctrl Pts',(-0.522012612882761,1.05825780349356,
-30.0137019191631));
#21824=CARTESIAN_POINT('Ctrl Pts',(-0.379417361706643,1.11015017237937,
-30.0238544504275));
#21825=CARTESIAN_POINT('Ctrl Pts',(-0.104280046962013,1.17139237118361,
-30.0430669469342));
#21826=CARTESIAN_POINT('Ctrl Pts',(0.0539287632978684,1.17564040536612,
-30.0536437922867));
#21827=CARTESIAN_POINT('Ctrl Pts',(0.377197010975957,1.11815960801922,-30.0760689537009));
#21828=CARTESIAN_POINT('Ctrl Pts',(0.513927950087557,1.05362922373644,-30.0861776722252));
#21829=CARTESIAN_POINT('Ctrl Pts',(0.747841111914757,0.907800899737507,
-30.1049627703414));
#21830=CARTESIAN_POINT('Ctrl Pts',(0.863967323007248,0.799686680741322,
-30.1155699393042));
#21831=CARTESIAN_POINT('Ctrl Pts',(1.0373733146488,0.553985095242675,-30.136112426456));
#21832=CARTESIAN_POINT('Ctrl Pts',(1.09762881343296,0.419173795090939,-30.1460123069918));
#21833=CARTESIAN_POINT('Ctrl Pts',(1.16276126940395,0.154335596280958,-30.1645976950093));
#21834=CARTESIAN_POINT('Ctrl Pts',(1.18066367741776,-0.00367979153003583,
-30.1752142761586));
#21835=CARTESIAN_POINT('Ctrl Pts',(1.13041480057629,-0.3239389012259,-30.1973572083032));
#21836=CARTESIAN_POINT('Ctrl Pts',(1.0795205548877,-0.463955778317747,-30.2073382677245));
#21837=CARTESIAN_POINT('Ctrl Pts',(0.94230830189785,-0.69825914566429,-30.2258424020917));
#21838=CARTESIAN_POINT('Ctrl Pts',(0.847055326004478,-0.823158197369149,
-30.2363291398121));
#21839=CARTESIAN_POINT('Ctrl Pts',(0.58473977016008,-1.02017668863558,-30.2587333398721));
#21840=CARTESIAN_POINT('Ctrl Pts',(0.449064049193789,-1.0859423776572,-30.2688267952486));
#21841=CARTESIAN_POINT('Ctrl Pts',(0.182033422095448,-1.15920947493991,
-30.2877001470212));
#21842=CARTESIAN_POINT('Ctrl Pts',(0.0285175083644867,-1.18025875562043,
-30.2980583573751));
#21843=CARTESIAN_POINT('Ctrl Pts',(-0.294874600697877,-1.13826266613818,
-30.320322632698));
#21844=CARTESIAN_POINT('Ctrl Pts',(-0.439600076520509,-1.09001309956843,
-30.3305283149136));
#21845=CARTESIAN_POINT('Ctrl Pts',(-0.705575432041423,-0.941860126973669,
-30.3512852188952));
#21846=CARTESIAN_POINT('Ctrl Pts',(-0.820426902272163,-0.844168464163858,
-30.3613874349407));
#21847=CARTESIAN_POINT('Ctrl Pts',(-1.00840900073707,-0.604724253435611,
-30.3821622194308));
#21848=CARTESIAN_POINT('Ctrl Pts',(-1.07871456427403,-0.467372055691335,
-30.3924781493725));
#21849=CARTESIAN_POINT('Ctrl Pts',(-1.16412445259044,-0.173935093258004,
-30.413322136256));
#21850=CARTESIAN_POINT('Ctrl Pts',(-1.17695775141982,-0.0212095663596662,
-30.423593955019));
#21851=CARTESIAN_POINT('Ctrl Pts',(-1.14090836976858,0.284233085157663,
-30.4445727801414));
#21852=CARTESIAN_POINT('Ctrl Pts',(-1.09334014169999,0.432850881490699,
-30.455000234412));
#21853=CARTESIAN_POINT('Ctrl Pts',(-0.978811871527169,0.640759463375194,
-30.4711994029217));
#21854=CARTESIAN_POINT('Ctrl Pts',(-0.930094913191883,0.710148119341155,
-30.4769583006743));
#21855=CARTESIAN_POINT('Ctrl Pts',(-0.817158075588233,0.837048534600839,
-30.4885647662489));
#21856=CARTESIAN_POINT('Ctrl Pts',(-0.753940691570741,0.893899928191477,
-30.49433436965));
#21857=CARTESIAN_POINT('Ctrl Pts',(-0.685457288884346,0.943445592256226,
-30.5000986093145));
#21858=CARTESIAN_POINT('Ctrl Pts',(-0.8405914827566,-0.809484597174,-26.82357429354));
#21859=CARTESIAN_POINT('Ctrl Pts',(-1.038951010123,-0.603502507076,-26.84307429354));
#21860=CARTESIAN_POINT('Ctrl Pts',(-1.27612225025,-0.0402741620545,-26.88207429354));
#21861=CARTESIAN_POINT('Ctrl Pts',(-0.9736143708746,0.8262775865961,-26.94057429354));
#21862=CARTESIAN_POINT('Ctrl Pts',(-0.1679846215786,1.265800345569,-26.99907429354));
#21863=CARTESIAN_POINT('Ctrl Pts',(0.7243492415226,1.051581514981,-27.05757429354));
#21864=CARTESIAN_POINT('Ctrl Pts',(1.242561604939,0.2941860805683,-27.11607429354));
#21865=CARTESIAN_POINT('Ctrl Pts',(1.118965951462,-0.6151566299544,-27.17457429354));
#21866=CARTESIAN_POINT('Ctrl Pts',(0.4174071783611,-1.206762071712,-27.23307429354));
#21867=CARTESIAN_POINT('Ctrl Pts',(-0.4997495938417,-1.175054711072,-27.29157429354));
#21868=CARTESIAN_POINT('Ctrl Pts',(-1.158777391072,-0.5364123471407,-27.35007429354));
#21869=CARTESIAN_POINT('Ctrl Pts',(-1.219277621892,0.3792958445976,-27.40857429354));
#21870=CARTESIAN_POINT('Ctrl Pts',(-0.6500008921559,1.099091485012,-27.46707429354));
#21871=CARTESIAN_POINT('Ctrl Pts',(0.2550119921671,1.251188290122,-27.52557429354));
#21872=CARTESIAN_POINT('Ctrl Pts',(1.028306986882,0.7570257552148,-27.58407429354));
#21873=CARTESIAN_POINT('Ctrl Pts',(1.270464502452,-0.128153038634,-27.64257429354));
#21874=CARTESIAN_POINT('Ctrl Pts',(0.8564061976507,-0.9471386793648,-27.70107429354));
#21875=CARTESIAN_POINT('Ctrl Pts',(0.,-1.276911607479,-27.75957429354));
#21876=CARTESIAN_POINT('Ctrl Pts',(-0.8564061976507,-0.9471386793648,-27.81807429354));
#21877=CARTESIAN_POINT('Ctrl Pts',(-1.270464502452,-0.128153038634,-27.87657429354));
#21878=CARTESIAN_POINT('Ctrl Pts',(-1.028306986882,0.7570257552148,-27.93507429354));
#21879=CARTESIAN_POINT('Ctrl Pts',(-0.2550119921671,1.251188290122,-27.99357429354));
#21880=CARTESIAN_POINT('Ctrl Pts',(0.6500008921559,1.099091485012,-28.05207429354));
#21881=CARTESIAN_POINT('Ctrl Pts',(1.219277621892,0.3792958445976,-28.11057429354));
#21882=CARTESIAN_POINT('Ctrl Pts',(1.158777391072,-0.5364123471407,-28.16907429354));
#21883=CARTESIAN_POINT('Ctrl Pts',(0.4997495938416,-1.175054711072,-28.22757429354));
#21884=CARTESIAN_POINT('Ctrl Pts',(-0.4174071783611,-1.206762071712,-28.28607429354));
#21885=CARTESIAN_POINT('Ctrl Pts',(-1.118965951462,-0.6151566299543,-28.34457429354));
#21886=CARTESIAN_POINT('Ctrl Pts',(-1.242561604939,0.2941860805683,-28.40307429354));
#21887=CARTESIAN_POINT('Ctrl Pts',(-0.7243492415226,1.051581514981,-28.46157429354));
#21888=CARTESIAN_POINT('Ctrl Pts',(0.1679846215786,1.265800345569,-28.52007429354));
#21889=CARTESIAN_POINT('Ctrl Pts',(0.9736143708746,0.8262775865961,-28.57857429354));
#21890=CARTESIAN_POINT('Ctrl Pts',(1.27612225025,-0.04027416205452,-28.63707429354));
#21891=CARTESIAN_POINT('Ctrl Pts',(1.038951010123,-0.603502507076,-28.67607429354));
#21892=CARTESIAN_POINT('Ctrl Pts',(0.8405914827566,-0.809484597174,-28.69557429354));
#21893=CARTESIAN_POINT('Ctrl Pts',(-0.8405914827566,-0.809484597174,-26.88906643118));
#21894=CARTESIAN_POINT('Ctrl Pts',(-1.038951010123,-0.603502507076,-26.90856643118));
#21895=CARTESIAN_POINT('Ctrl Pts',(-1.27612225025,-0.0402741620545,-26.94756643118));
#21896=CARTESIAN_POINT('Ctrl Pts',(-0.9736143708746,0.8262775865961,-27.00606643118));
#21897=CARTESIAN_POINT('Ctrl Pts',(-0.1679846215786,1.265800345569,-27.06456643118));
#21898=CARTESIAN_POINT('Ctrl Pts',(0.7243492415226,1.051581514981,-27.12306643118));
#21899=CARTESIAN_POINT('Ctrl Pts',(1.242561604939,0.2941860805683,-27.18156643118));
#21900=CARTESIAN_POINT('Ctrl Pts',(1.118965951462,-0.6151566299544,-27.24006643118));
#21901=CARTESIAN_POINT('Ctrl Pts',(0.4174071783611,-1.206762071712,-27.29856643118));
#21902=CARTESIAN_POINT('Ctrl Pts',(-0.4997495938417,-1.175054711072,-27.35706643118));
#21903=CARTESIAN_POINT('Ctrl Pts',(-1.158777391072,-0.5364123471407,-27.41556643118));
#21904=CARTESIAN_POINT('Ctrl Pts',(-1.219277621892,0.3792958445976,-27.47406643118));
#21905=CARTESIAN_POINT('Ctrl Pts',(-0.6500008921559,1.099091485012,-27.53256643118));
#21906=CARTESIAN_POINT('Ctrl Pts',(0.2550119921671,1.251188290122,-27.59106643118));
#21907=CARTESIAN_POINT('Ctrl Pts',(1.028306986882,0.7570257552148,-27.64956643118));
#21908=CARTESIAN_POINT('Ctrl Pts',(1.270464502452,-0.128153038634,-27.70806643118));
#21909=CARTESIAN_POINT('Ctrl Pts',(0.8564061976507,-0.9471386793648,-27.76656643118));
#21910=CARTESIAN_POINT('Ctrl Pts',(0.,-1.276911607479,-27.82506643118));
#21911=CARTESIAN_POINT('Ctrl Pts',(-0.8564061976507,-0.9471386793648,-27.88356643118));
#21912=CARTESIAN_POINT('Ctrl Pts',(-1.270464502452,-0.128153038634,-27.94206643118));
#21913=CARTESIAN_POINT('Ctrl Pts',(-1.028306986882,0.7570257552148,-28.00056643118));
#21914=CARTESIAN_POINT('Ctrl Pts',(-0.2550119921671,1.251188290122,-28.05906643118));
#21915=CARTESIAN_POINT('Ctrl Pts',(0.6500008921559,1.099091485012,-28.11756643118));
#21916=CARTESIAN_POINT('Ctrl Pts',(1.219277621892,0.3792958445976,-28.17606643118));
#21917=CARTESIAN_POINT('Ctrl Pts',(1.158777391072,-0.5364123471407,-28.23456643118));
#21918=CARTESIAN_POINT('Ctrl Pts',(0.4997495938416,-1.175054711072,-28.29306643118));
#21919=CARTESIAN_POINT('Ctrl Pts',(-0.4174071783611,-1.206762071712,-28.35156643118));
#21920=CARTESIAN_POINT('Ctrl Pts',(-1.118965951462,-0.6151566299543,-28.41006643118));
#21921=CARTESIAN_POINT('Ctrl Pts',(-1.242561604939,0.2941860805683,-28.46856643118));
#21922=CARTESIAN_POINT('Ctrl Pts',(-0.7243492415226,1.051581514981,-28.52706643118));
#21923=CARTESIAN_POINT('Ctrl Pts',(0.1679846215786,1.265800345569,-28.58556643118));
#21924=CARTESIAN_POINT('Ctrl Pts',(0.9736143708746,0.8262775865961,-28.64406643118));
#21925=CARTESIAN_POINT('Ctrl Pts',(1.27612225025,-0.04027416205452,-28.70256643118));
#21926=CARTESIAN_POINT('Ctrl Pts',(1.038951010123,-0.603502507076,-28.74156643118));
#21927=CARTESIAN_POINT('Ctrl Pts',(0.8405914827566,-0.809484597174,-28.76106643118));
#21928=CARTESIAN_POINT('Ctrl Pts',(-0.8405914827566,-0.809484597174,-26.95455856882));
#21929=CARTESIAN_POINT('Ctrl Pts',(-1.038951010123,-0.603502507076,-26.97405856882));
#21930=CARTESIAN_POINT('Ctrl Pts',(-1.27612225025,-0.0402741620545,-27.01305856882));
#21931=CARTESIAN_POINT('Ctrl Pts',(-0.9736143708746,0.8262775865961,-27.07155856882));
#21932=CARTESIAN_POINT('Ctrl Pts',(-0.1679846215786,1.265800345569,-27.13005856882));
#21933=CARTESIAN_POINT('Ctrl Pts',(0.7243492415226,1.051581514981,-27.18855856882));
#21934=CARTESIAN_POINT('Ctrl Pts',(1.242561604939,0.2941860805683,-27.24705856882));
#21935=CARTESIAN_POINT('Ctrl Pts',(1.118965951462,-0.6151566299544,-27.30555856882));
#21936=CARTESIAN_POINT('Ctrl Pts',(0.4174071783611,-1.206762071712,-27.36405856882));
#21937=CARTESIAN_POINT('Ctrl Pts',(-0.4997495938417,-1.175054711072,-27.42255856882));
#21938=CARTESIAN_POINT('Ctrl Pts',(-1.158777391072,-0.5364123471407,-27.48105856882));
#21939=CARTESIAN_POINT('Ctrl Pts',(-1.219277621892,0.3792958445976,-27.53955856882));
#21940=CARTESIAN_POINT('Ctrl Pts',(-0.6500008921559,1.099091485012,-27.59805856882));
#21941=CARTESIAN_POINT('Ctrl Pts',(0.2550119921671,1.251188290122,-27.65655856882));
#21942=CARTESIAN_POINT('Ctrl Pts',(1.028306986882,0.7570257552148,-27.71505856882));
#21943=CARTESIAN_POINT('Ctrl Pts',(1.270464502452,-0.128153038634,-27.77355856882));
#21944=CARTESIAN_POINT('Ctrl Pts',(0.8564061976507,-0.9471386793648,-27.83205856882));
#21945=CARTESIAN_POINT('Ctrl Pts',(0.,-1.276911607479,-27.89055856882));
#21946=CARTESIAN_POINT('Ctrl Pts',(-0.8564061976507,-0.9471386793648,-27.94905856882));
#21947=CARTESIAN_POINT('Ctrl Pts',(-1.270464502452,-0.128153038634,-28.00755856882));
#21948=CARTESIAN_POINT('Ctrl Pts',(-1.028306986882,0.7570257552148,-28.06605856882));
#21949=CARTESIAN_POINT('Ctrl Pts',(-0.2550119921671,1.251188290122,-28.12455856882));
#21950=CARTESIAN_POINT('Ctrl Pts',(0.6500008921559,1.099091485012,-28.18305856882));
#21951=CARTESIAN_POINT('Ctrl Pts',(1.219277621892,0.3792958445976,-28.24155856882));
#21952=CARTESIAN_POINT('Ctrl Pts',(1.158777391072,-0.5364123471407,-28.30005856882));
#21953=CARTESIAN_POINT('Ctrl Pts',(0.4997495938416,-1.175054711072,-28.35855856882));
#21954=CARTESIAN_POINT('Ctrl Pts',(-0.4174071783611,-1.206762071712,-28.41705856882));
#21955=CARTESIAN_POINT('Ctrl Pts',(-1.118965951462,-0.6151566299543,-28.47555856882));
#21956=CARTESIAN_POINT('Ctrl Pts',(-1.242561604939,0.2941860805683,-28.53405856882));
#21957=CARTESIAN_POINT('Ctrl Pts',(-0.7243492415226,1.051581514981,-28.59255856882));
#21958=CARTESIAN_POINT('Ctrl Pts',(0.1679846215786,1.265800345569,-28.65105856882));
#21959=CARTESIAN_POINT('Ctrl Pts',(0.9736143708746,0.8262775865961,-28.70955856882));
#21960=CARTESIAN_POINT('Ctrl Pts',(1.27612225025,-0.04027416205452,-28.76805856882));
#21961=CARTESIAN_POINT('Ctrl Pts',(1.038951010123,-0.603502507076,-28.80705856882));
#21962=CARTESIAN_POINT('Ctrl Pts',(0.8405914827566,-0.809484597174,-28.82655856882));
#21963=CARTESIAN_POINT('Ctrl Pts',(-0.8405914827566,-0.809484597174,-27.02005070646));
#21964=CARTESIAN_POINT('Ctrl Pts',(-1.038951010123,-0.603502507076,-27.03955070646));
#21965=CARTESIAN_POINT('Ctrl Pts',(-1.27612225025,-0.0402741620545,-27.07855070646));
#21966=CARTESIAN_POINT('Ctrl Pts',(-0.9736143708746,0.8262775865961,-27.13705070646));
#21967=CARTESIAN_POINT('Ctrl Pts',(-0.1679846215786,1.265800345569,-27.19555070646));
#21968=CARTESIAN_POINT('Ctrl Pts',(0.7243492415226,1.051581514981,-27.25405070646));
#21969=CARTESIAN_POINT('Ctrl Pts',(1.242561604939,0.2941860805683,-27.31255070646));
#21970=CARTESIAN_POINT('Ctrl Pts',(1.118965951462,-0.6151566299544,-27.37105070646));
#21971=CARTESIAN_POINT('Ctrl Pts',(0.4174071783611,-1.206762071712,-27.42955070646));
#21972=CARTESIAN_POINT('Ctrl Pts',(-0.4997495938417,-1.175054711072,-27.48805070646));
#21973=CARTESIAN_POINT('Ctrl Pts',(-1.158777391072,-0.5364123471407,-27.54655070646));
#21974=CARTESIAN_POINT('Ctrl Pts',(-1.219277621892,0.3792958445976,-27.60505070646));
#21975=CARTESIAN_POINT('Ctrl Pts',(-0.6500008921559,1.099091485012,-27.66355070646));
#21976=CARTESIAN_POINT('Ctrl Pts',(0.2550119921671,1.251188290122,-27.72205070646));
#21977=CARTESIAN_POINT('Ctrl Pts',(1.028306986882,0.7570257552148,-27.78055070646));
#21978=CARTESIAN_POINT('Ctrl Pts',(1.270464502452,-0.128153038634,-27.83905070646));
#21979=CARTESIAN_POINT('Ctrl Pts',(0.8564061976507,-0.9471386793648,-27.89755070646));
#21980=CARTESIAN_POINT('Ctrl Pts',(0.,-1.276911607479,-27.95605070646));
#21981=CARTESIAN_POINT('Ctrl Pts',(-0.8564061976507,-0.9471386793648,-28.01455070646));
#21982=CARTESIAN_POINT('Ctrl Pts',(-1.270464502452,-0.128153038634,-28.07305070646));
#21983=CARTESIAN_POINT('Ctrl Pts',(-1.028306986882,0.7570257552148,-28.13155070646));
#21984=CARTESIAN_POINT('Ctrl Pts',(-0.2550119921671,1.251188290122,-28.19005070646));
#21985=CARTESIAN_POINT('Ctrl Pts',(0.6500008921559,1.099091485012,-28.24855070646));
#21986=CARTESIAN_POINT('Ctrl Pts',(1.219277621892,0.3792958445976,-28.30705070646));
#21987=CARTESIAN_POINT('Ctrl Pts',(1.158777391072,-0.5364123471407,-28.36555070646));
#21988=CARTESIAN_POINT('Ctrl Pts',(0.4997495938416,-1.175054711072,-28.42405070646));
#21989=CARTESIAN_POINT('Ctrl Pts',(-0.4174071783611,-1.206762071712,-28.48255070646));
#21990=CARTESIAN_POINT('Ctrl Pts',(-1.118965951462,-0.6151566299543,-28.54105070646));
#21991=CARTESIAN_POINT('Ctrl Pts',(-1.242561604939,0.2941860805683,-28.59955070646));
#21992=CARTESIAN_POINT('Ctrl Pts',(-0.7243492415226,1.051581514981,-28.65805070646));
#21993=CARTESIAN_POINT('Ctrl Pts',(0.1679846215786,1.265800345569,-28.71655070646));
#21994=CARTESIAN_POINT('Ctrl Pts',(0.9736143708746,0.8262775865961,-28.77505070646));
#21995=CARTESIAN_POINT('Ctrl Pts',(1.27612225025,-0.04027416205452,-28.83355070646));
#21996=CARTESIAN_POINT('Ctrl Pts',(1.038951010123,-0.603502507076,-28.87255070646));
#21997=CARTESIAN_POINT('Ctrl Pts',(0.8405914827566,-0.809484597174,-28.89205070646));
#21998=CARTESIAN_POINT('',(-1.10987074437248,-0.360618864706213,-26.9000774755696));
#21999=CARTESIAN_POINT('',(-1.10987074442631,-0.360618864754735,-27.0155475173803));
#22000=CARTESIAN_POINT('',(-1.109870874299,-0.360618907335,-26.90007747308));
#22001=CARTESIAN_POINT('Ctrl Pts',(-1.1090896887684,-0.360362786612198,
-27.0155263221856));
#22002=CARTESIAN_POINT('Ctrl Pts',(-1.1353675790678,-0.280038839228305,
-27.021289639903));
#22003=CARTESIAN_POINT('Ctrl Pts',(-1.15309370880972,-0.196900618773424,
-27.0270583193289));
#22004=CARTESIAN_POINT('Ctrl Pts',(-1.16987757186606,-0.0278535081970832,
-27.0386648185785));
#22005=CARTESIAN_POINT('Ctrl Pts',(-1.16850615302417,0.0569319254105346,
-27.0444246367462));
#22006=CARTESIAN_POINT('Ctrl Pts',(-1.13895411984996,0.29246549187405,-27.0606247655881));
#22007=CARTESIAN_POINT('Ctrl Pts',(-1.09008227583705,0.440659717710459,
-27.0710522198587));
#22008=CARTESIAN_POINT('Ctrl Pts',(-0.939712152246719,0.708957308483853,
-27.0920310449811));
#22009=CARTESIAN_POINT('Ctrl Pts',(-0.839559983040467,0.824971631429354,
-27.102302863744));
#22010=CARTESIAN_POINT('Ctrl Pts',(-0.597984012908985,1.01216444806353,
-27.1231468506276));
#22011=CARTESIAN_POINT('Ctrl Pts',(-0.460372021004354,1.08196013685235,
-27.1334627805692));
#22012=CARTESIAN_POINT('Ctrl Pts',(-0.167549532895036,1.16518146736364,
-27.1542375650593));
#22013=CARTESIAN_POINT('Ctrl Pts',(-0.0172110229777723,1.17670768237989,
-27.1643397811049));
#22014=CARTESIAN_POINT('Ctrl Pts',(0.285049692098096,1.14022956352786,-27.1850966850866));
#22015=CARTESIAN_POINT('Ctrl Pts',(0.43049544521667,1.09419678253459,-27.1953023673022));
#22016=CARTESIAN_POINT('Ctrl Pts',(0.716809839346208,0.938087220208753,
-27.2175666426251));
#22017=CARTESIAN_POINT('Ctrl Pts',(0.828634365706049,0.830823604335811,
-27.2279248529789));
#22018=CARTESIAN_POINT('Ctrl Pts',(1.00160136178627,0.614592612986834,-27.2467982047513));
#22019=CARTESIAN_POINT('Ctrl Pts',(1.07270922365843,0.481638865043252,-27.2568916601276));
#22020=CARTESIAN_POINT('Ctrl Pts',(1.16912240263033,0.168062342229928,-27.2792958601875));
#22021=CARTESIAN_POINT('Ctrl Pts',(1.17276985827545,0.0110285923520621,
-27.2897825979079));
#22022=CARTESIAN_POINT('Ctrl Pts',(1.14605683889197,-0.259178152412114,
-27.3082867322752));
#22023=CARTESIAN_POINT('Ctrl Pts',(1.1049312931433,-0.402369072521155,-27.3182677916966));
#22024=CARTESIAN_POINT('Ctrl Pts',(0.957339906864926,-0.69099968362001,
-27.3404107238413));
#22025=CARTESIAN_POINT('Ctrl Pts',(0.849977439951136,-0.808314046320928,
-27.3510273049907));
#22026=CARTESIAN_POINT('Ctrl Pts',(0.641616188680965,-0.984288752852637,
-27.3696126930084));
#22027=CARTESIAN_POINT('Ctrl Pts',(0.513628372088824,-1.05793609215418,
-27.3795125735442));
#22028=CARTESIAN_POINT('Ctrl Pts',(0.228920209503694,-1.15478736582146,
-27.400055060696));
#22029=CARTESIAN_POINT('Ctrl Pts',(0.0714241877483168,-1.17399633203817,
-27.4106622296586));
#22030=CARTESIAN_POINT('Ctrl Pts',(-0.203531273591206,-1.15448321757536,
-27.4294473277747));
#22031=CARTESIAN_POINT('Ctrl Pts',(-0.352078935195878,-1.12632096557171,
-27.4395560462991));
#22032=CARTESIAN_POINT('Ctrl Pts',(-0.64739480628011,-0.982811598955728,
-27.4619812077134));
#22033=CARTESIAN_POINT('Ctrl Pts',(-0.772891490596436,-0.886382061656004,
-27.472558053066));
#22034=CARTESIAN_POINT('Ctrl Pts',(-0.959484992736287,-0.675114426088524,
-27.4917705495728));
#22035=CARTESIAN_POINT('Ctrl Pts',(-1.04434540511724,-0.549317232093508,
-27.5019230808371));
#22036=CARTESIAN_POINT('Ctrl Pts',(-1.1515608225355,-0.240698826534252,
-27.5242292828711));
#22037=CARTESIAN_POINT('Ctrl Pts',(-1.172855145901,-0.0847008837209633,
-27.5347495650282));
#22038=CARTESIAN_POINT('Ctrl Pts',(-1.1553273946675,0.2249882773451,-27.555898376323));
#22039=CARTESIAN_POINT('Ctrl Pts',(-1.11708899258416,0.370182100385514,
-27.5659604824617));
#22040=CARTESIAN_POINT('Ctrl Pts',(-0.984380269778333,0.643433278699838,
-27.5866904752756));
#22041=CARTESIAN_POINT('Ctrl Pts',(-0.890301982635328,0.768087674628798,
-27.59712681397));
#22042=CARTESIAN_POINT('Ctrl Pts',(-0.66155868775765,0.973611514425885,
-27.6181021416964));
#22043=CARTESIAN_POINT('Ctrl Pts',(-0.529578637445949,1.0512078955982,-27.6283633413595));
#22044=CARTESIAN_POINT('Ctrl Pts',(-0.240409186122318,1.15078313340772,
-27.6492232952252));
#22045=CARTESIAN_POINT('Ctrl Pts',(-0.087461943617362,1.17256057451052,
-27.6595514605358));
#22046=CARTESIAN_POINT('Ctrl Pts',(0.215278414854982,1.15709812005245,-27.6802380394372));
#22047=CARTESIAN_POINT('Ctrl Pts',(0.361409610940379,1.12019171609551,-27.6903371103176));
#22048=CARTESIAN_POINT('Ctrl Pts',(0.637209668148432,0.98762997462939,-27.7112005351714));
#22049=CARTESIAN_POINT('Ctrl Pts',(0.76021498715122,0.897029079457893,-27.7214196096765));
#22050=CARTESIAN_POINT('Ctrl Pts',(0.980813909196912,0.657035707477414,
-27.7436737563467));
#22051=CARTESIAN_POINT('Ctrl Pts',(1.05211545721986,0.519720702111876,-27.7540179844193));
#22052=CARTESIAN_POINT('Ctrl Pts',(1.14631134349229,0.258739401713321,-27.7729300210825));
#22053=CARTESIAN_POINT('Ctrl Pts',(1.17073802586279,0.10974099037791,-27.783036857759));
#22054=CARTESIAN_POINT('Ctrl Pts',(1.1608022340359,-0.217860149407178,-27.8054191523545));
#22055=CARTESIAN_POINT('Ctrl Pts',(1.11384179304919,-0.367478577023206,
-27.8158902244773));
#22056=CARTESIAN_POINT('Ctrl Pts',(1.00106258513422,-0.615242280715572,
-27.8344423045362));
#22057=CARTESIAN_POINT('Ctrl Pts',(0.915771023800586,-0.737649456469355,
-27.8444366233426));
#22058=CARTESIAN_POINT('Ctrl Pts',(0.671599012721525,-0.974057539532169,
-27.8676508056259));
#22059=CARTESIAN_POINT('Ctrl Pts',(0.525608038221144,-1.04645149616782,
-27.8784973022941));
#22060=CARTESIAN_POINT('Ctrl Pts',(0.289520576217103,-1.13869075984127,
-27.8957700105567));
#22061=CARTESIAN_POINT('Ctrl Pts',(0.144847436238182,-1.1669872981076,-27.9056531858431));
#22062=CARTESIAN_POINT('Ctrl Pts',(-0.144847436238183,-1.1669872981076,
-27.9254418679969));
#22063=CARTESIAN_POINT('Ctrl Pts',(-0.289520576217105,-1.13869075984127,
-27.9353250432865));
#22064=CARTESIAN_POINT('Ctrl Pts',(-0.525608038221115,-1.04645149616783,
-27.9525977515491));
#22065=CARTESIAN_POINT('Ctrl Pts',(-0.671599012721508,-0.974057539532187,
-27.9634442482174));
#22066=CARTESIAN_POINT('Ctrl Pts',(-0.915771023800589,-0.737649456469351,
-27.9866584305007));
#22067=CARTESIAN_POINT('Ctrl Pts',(-1.00106258513423,-0.615242280715567,
-27.9966527493071));
#22068=CARTESIAN_POINT('Ctrl Pts',(-1.11384179304919,-0.367478577023195,
-28.0152048293662));
#22069=CARTESIAN_POINT('Ctrl Pts',(-1.1608022340359,-0.217860149407165,
-28.025675901489));
#22070=CARTESIAN_POINT('Ctrl Pts',(-1.17073802586279,0.109740990377929,
-28.0480581960845));
#22071=CARTESIAN_POINT('Ctrl Pts',(-1.14631134349228,0.258739401713341,
-28.0581650327611));
#22072=CARTESIAN_POINT('Ctrl Pts',(-1.05211545721985,0.519720702111896,
-28.0770770694243));
#22073=CARTESIAN_POINT('Ctrl Pts',(-0.980813909196899,0.657035707477435,
-28.0874212974969));
#22074=CARTESIAN_POINT('Ctrl Pts',(-0.760214987151199,0.897029079457912,
-28.1096754441671));
#22075=CARTESIAN_POINT('Ctrl Pts',(-0.637209668148406,0.987629974629407,
-28.1198945186723));
#22076=CARTESIAN_POINT('Ctrl Pts',(-0.361409610940352,1.12019171609552,
-28.140757943526));
#22077=CARTESIAN_POINT('Ctrl Pts',(-0.215278414854954,1.15709812005246,
-28.1508570144065));
#22078=CARTESIAN_POINT('Ctrl Pts',(0.0874619436173922,1.17256057451051,
-28.1715435933079));
#22079=CARTESIAN_POINT('Ctrl Pts',(0.240409186122349,1.15078313340772,-28.1818717586184));
#22080=CARTESIAN_POINT('Ctrl Pts',(0.529578637445975,1.05120789559819,-28.202731712484));
#22081=CARTESIAN_POINT('Ctrl Pts',(0.661558687757671,0.97361151442587,-28.212992912147));
#22082=CARTESIAN_POINT('Ctrl Pts',(0.890301982635341,0.768087674628783,
-28.2339682398733));
#22083=CARTESIAN_POINT('Ctrl Pts',(0.984380269778343,0.643433278699822,
-28.2444045785678));
#22084=CARTESIAN_POINT('Ctrl Pts',(1.11708899258417,0.370182100385499,-28.2651345713816));
#22085=CARTESIAN_POINT('Ctrl Pts',(1.1553273946675,0.224988277345085,-28.2751966775203));
#22086=CARTESIAN_POINT('Ctrl Pts',(1.17285514590099,-0.0847008837209673,
-28.2963454888151));
#22087=CARTESIAN_POINT('Ctrl Pts',(1.15156082253549,-0.240698826534245,
-28.3068657709722));
#22088=CARTESIAN_POINT('Ctrl Pts',(1.04434540511724,-0.549317232093477,
-28.3291719730061));
#22089=CARTESIAN_POINT('Ctrl Pts',(0.959484992736284,-0.675114426088482,
-28.3393245042704));
#22090=CARTESIAN_POINT('Ctrl Pts',(0.77289149059643,-0.886382061655964,
-28.3585370007771));
#22091=CARTESIAN_POINT('Ctrl Pts',(0.647394806280091,-0.982811598955699,
-28.3691138461296));
#22092=CARTESIAN_POINT('Ctrl Pts',(0.352078935195832,-1.12632096557171,
-28.3915390075439));
#22093=CARTESIAN_POINT('Ctrl Pts',(0.203531273591148,-1.15448321757536,
-28.4016477260684));
#22094=CARTESIAN_POINT('Ctrl Pts',(-0.0714241877483651,-1.17399633203817,
-28.4204328241847));
#22095=CARTESIAN_POINT('Ctrl Pts',(-0.228920209503715,-1.15478736582145,
-28.4310399931476));
#22096=CARTESIAN_POINT('Ctrl Pts',(-0.513628372088804,-1.05793609215417,
-28.4515824802994));
#22097=CARTESIAN_POINT('Ctrl Pts',(-0.641616188680927,-0.984288752852624,
-28.4614823608352));
#22098=CARTESIAN_POINT('Ctrl Pts',(-0.849977439951157,-0.808314046320862,
-28.4800677488528));
#22099=CARTESIAN_POINT('Ctrl Pts',(-0.957339906864942,-0.69099968361991,
-28.4906843300021));
#22100=CARTESIAN_POINT('Ctrl Pts',(-1.1049312931433,-0.402369072521084,
-28.5128272621466));
#22101=CARTESIAN_POINT('Ctrl Pts',(-1.14605683889198,-0.25917815241204,
-28.5228083215678));
#22102=CARTESIAN_POINT('Ctrl Pts',(-1.17276985827545,0.011028592352134,
-28.5413124559349));
#22103=CARTESIAN_POINT('Ctrl Pts',(-1.16912240263032,0.168062342229976,
-28.5517991936552));
#22104=CARTESIAN_POINT('Ctrl Pts',(-1.07270922365842,0.481638865043274,
-28.5742033937153));
#22105=CARTESIAN_POINT('Ctrl Pts',(-1.00160136178626,0.614592612986856,
-28.5842968490919));
#22106=CARTESIAN_POINT('Ctrl Pts',(-0.828634365706032,0.830823604335828,
-28.6031702008645));
#22107=CARTESIAN_POINT('Ctrl Pts',(-0.716809839346184,0.938087220208773,
-28.6135284112185));
#22108=CARTESIAN_POINT('Ctrl Pts',(-0.430495445216628,1.0941967825346,-28.6357926865415));
#22109=CARTESIAN_POINT('Ctrl Pts',(-0.285049692098049,1.14022956352787,
-28.645998368757));
#22110=CARTESIAN_POINT('Ctrl Pts',(0.0172110229778327,1.17670768237989,
-28.6667552727386));
#22111=CARTESIAN_POINT('Ctrl Pts',(0.167549532895092,1.16518146736363,-28.6768574887841));
#22112=CARTESIAN_POINT('Ctrl Pts',(0.460372021004397,1.08196013685233,-28.6976322732742));
#22113=CARTESIAN_POINT('Ctrl Pts',(0.597984012909024,1.01216444806351,-28.7079482032158));
#22114=CARTESIAN_POINT('Ctrl Pts',(0.839559983040498,0.824971631429321,
-28.7287921900993));
#22115=CARTESIAN_POINT('Ctrl Pts',(0.939712152246743,0.708957308483815,
-28.7390640088623));
#22116=CARTESIAN_POINT('Ctrl Pts',(1.09008227583707,0.440659717710412,-28.7600428339848));
#22117=CARTESIAN_POINT('Ctrl Pts',(1.13895411984998,0.292465491873993,-28.7704702882555));
#22118=CARTESIAN_POINT('Ctrl Pts',(1.16850615302413,0.0569319254108322,
-28.7866704170975));
#22119=CARTESIAN_POINT('Ctrl Pts',(1.16987757186605,-0.0278535081964251,
-28.7924302352651));
#22120=CARTESIAN_POINT('Ctrl Pts',(1.15309371461848,-0.1969005602683,-28.8040367304978));
#22121=CARTESIAN_POINT('Ctrl Pts',(1.13536760373153,-0.280038723551826,
-28.809805405914));
#22122=CARTESIAN_POINT('Ctrl Pts',(1.10908974361186,-0.360362618971496,
-28.8155687196295));
#22123=CARTESIAN_POINT('Ctrl Pts',(-1.10908974361187,-0.360362618971445,
-26.9000562803705));
#22124=CARTESIAN_POINT('Ctrl Pts',(-1.13536760373151,-0.280038723551868,
-26.905819594086));
#22125=CARTESIAN_POINT('Ctrl Pts',(-1.15309371461845,-0.196900560268445,
-26.9115882695022));
#22126=CARTESIAN_POINT('Ctrl Pts',(-1.16987757186605,-0.0278535081965757,
-26.9231947647349));
#22127=CARTESIAN_POINT('Ctrl Pts',(-1.16850615302414,0.0569319254107759,
-26.9289545829025));
#22128=CARTESIAN_POINT('Ctrl Pts',(-1.13895411984997,0.292465491874028,
-26.9451547117445));
#22129=CARTESIAN_POINT('Ctrl Pts',(-1.09008227583706,0.440659717710443,
-26.9555821660152));
#22130=CARTESIAN_POINT('Ctrl Pts',(-0.939712152246728,0.708957308483841,
-26.9765609911377));
#22131=CARTESIAN_POINT('Ctrl Pts',(-0.839559983040477,0.824971631429344,
-26.9868328099007));
#22132=CARTESIAN_POINT('Ctrl Pts',(-0.597984012908997,1.01216444806352,
-27.0076767967842));
#22133=CARTESIAN_POINT('Ctrl Pts',(-0.460372021004369,1.08196013685234,
-27.0179927267258));
#22134=CARTESIAN_POINT('Ctrl Pts',(-0.167549532895057,1.16518146736364,
-27.0387675112159));
#22135=CARTESIAN_POINT('Ctrl Pts',(-0.0172110229777962,1.17670768237989,
-27.0488697272614));
#22136=CARTESIAN_POINT('Ctrl Pts',(0.285049692098077,1.14022956352786,-27.069626631243));
#22137=CARTESIAN_POINT('Ctrl Pts',(0.430495445216654,1.09419678253459,-27.0798323134585));
#22138=CARTESIAN_POINT('Ctrl Pts',(0.716809839346204,0.938087220208758,
-27.1020965887815));
#22139=CARTESIAN_POINT('Ctrl Pts',(0.828634365706049,0.830823604335812,
-27.1124547991355));
#22140=CARTESIAN_POINT('Ctrl Pts',(1.00160136178628,0.614592612986832,-27.1313281509081));
#22141=CARTESIAN_POINT('Ctrl Pts',(1.07270922365843,0.481638865043245,-27.1414216062847));
#22142=CARTESIAN_POINT('Ctrl Pts',(1.16912240263033,0.168062342229917,-27.1638258063448));
#22143=CARTESIAN_POINT('Ctrl Pts',(1.17276985827545,0.0110285923520512,
-27.1743125440651));
#22144=CARTESIAN_POINT('Ctrl Pts',(1.14605683889197,-0.25917815241212,-27.1928166784322));
#22145=CARTESIAN_POINT('Ctrl Pts',(1.1049312931433,-0.402369072521154,-27.2027977378534));
#22146=CARTESIAN_POINT('Ctrl Pts',(0.957339906864935,-0.690999683619994,
-27.2249406699979));
#22147=CARTESIAN_POINT('Ctrl Pts',(0.849977439951153,-0.80831404632091,
-27.2355572511472));
#22148=CARTESIAN_POINT('Ctrl Pts',(0.64161618868098,-0.984288752852628,
-27.2541426391648));
#22149=CARTESIAN_POINT('Ctrl Pts',(0.513628372088837,-1.05793609215418,
-27.2640425197005));
#22150=CARTESIAN_POINT('Ctrl Pts',(0.228920209503699,-1.15478736582146,
-27.2845850068524));
#22151=CARTESIAN_POINT('Ctrl Pts',(0.0714241877483137,-1.17399633203818,
-27.2951921758153));
#22152=CARTESIAN_POINT('Ctrl Pts',(-0.203531273591216,-1.15448321757536,
-27.3139772739317));
#22153=CARTESIAN_POINT('Ctrl Pts',(-0.352078935195889,-1.12632096557171,
-27.3240859924561));
#22154=CARTESIAN_POINT('Ctrl Pts',(-0.647394806280115,-0.982811598955724,
-27.3465111538704));
#22155=CARTESIAN_POINT('Ctrl Pts',(-0.772891490596438,-0.886382061656001,
-27.3570879992229));
#22156=CARTESIAN_POINT('Ctrl Pts',(-0.959484992736288,-0.675114426088524,
-27.3763004957296));
#22157=CARTESIAN_POINT('Ctrl Pts',(-1.04434540511724,-0.549317232093508,
-27.3864530269939));
#22158=CARTESIAN_POINT('Ctrl Pts',(-1.1515608225355,-0.240698826534257,
-27.4087592290278));
#22159=CARTESIAN_POINT('Ctrl Pts',(-1.172855145901,-0.084700883720971,-27.4192795111849));
#22160=CARTESIAN_POINT('Ctrl Pts',(-1.1553273946675,0.224988277345099,-27.4404283224797));
#22161=CARTESIAN_POINT('Ctrl Pts',(-1.11708899258416,0.370182100385512,
-27.4504904286184));
#22162=CARTESIAN_POINT('Ctrl Pts',(-0.984380269778341,0.643433278699826,
-27.4712204214322));
#22163=CARTESIAN_POINT('Ctrl Pts',(-0.890301982635338,0.768087674628786,
-27.4816567601267));
#22164=CARTESIAN_POINT('Ctrl Pts',(-0.661558687757666,0.973611514425873,
-27.502632087853));
#22165=CARTESIAN_POINT('Ctrl Pts',(-0.52957863744597,1.05120789559819,-27.512893287516));
#22166=CARTESIAN_POINT('Ctrl Pts',(-0.240409186122344,1.15078313340772,
-27.5337532413816));
#22167=CARTESIAN_POINT('Ctrl Pts',(-0.0874619436173883,1.17256057451051,
-27.5440814066922));
#22168=CARTESIAN_POINT('Ctrl Pts',(0.215278414854953,1.15709812005246,-27.5647679855935));
#22169=CARTESIAN_POINT('Ctrl Pts',(0.361409610940351,1.12019171609552,-27.574867056474));
#22170=CARTESIAN_POINT('Ctrl Pts',(0.637209668148408,0.987629974629406,
-27.5957304813277));
#22171=CARTESIAN_POINT('Ctrl Pts',(0.7602149871512,0.897029079457911,-27.6059495558329));
#22172=CARTESIAN_POINT('Ctrl Pts',(0.980813909196898,0.657035707477434,
-27.6282037025032));
#22173=CARTESIAN_POINT('Ctrl Pts',(1.05211545721985,0.519720702111898,-27.6385479305757));
#22174=CARTESIAN_POINT('Ctrl Pts',(1.14631134349228,0.258739401713341,-27.6574599672389));
#22175=CARTESIAN_POINT('Ctrl Pts',(1.17073802586279,0.109740990377928,-27.6675668039155));
#22176=CARTESIAN_POINT('Ctrl Pts',(1.1608022340359,-0.217860149407165,-27.689949098511));
#22177=CARTESIAN_POINT('Ctrl Pts',(1.11384179304919,-0.367478577023196,
-27.7004201706339));
#22178=CARTESIAN_POINT('Ctrl Pts',(1.00106258513423,-0.615242280715565,
-27.7189722506929));
#22179=CARTESIAN_POINT('Ctrl Pts',(0.91577102380059,-0.73764945646935,-27.7289665694993));
#22180=CARTESIAN_POINT('Ctrl Pts',(0.671599012721526,-0.974057539532169,
-27.7521807517826));
#22181=CARTESIAN_POINT('Ctrl Pts',(0.525608038221143,-1.04645149616782,
-27.7630272484509));
#22182=CARTESIAN_POINT('Ctrl Pts',(0.289520576217104,-1.13869075984127,
-27.7802999567135));
#22183=CARTESIAN_POINT('Ctrl Pts',(0.144847436238183,-1.1669872981076,-27.7901831320031));
#22184=CARTESIAN_POINT('Ctrl Pts',(-0.144847436238183,-1.1669872981076,
-27.8099718141569));
#22185=CARTESIAN_POINT('Ctrl Pts',(-0.289520576217104,-1.13869075984127,
-27.8198549894433));
#22186=CARTESIAN_POINT('Ctrl Pts',(-0.525608038221108,-1.04645149616784,
-27.8371276977059));
#22187=CARTESIAN_POINT('Ctrl Pts',(-0.671599012721502,-0.974057539532192,
-27.8479741943741));
#22188=CARTESIAN_POINT('Ctrl Pts',(-0.915771023800586,-0.737649456469355,
-27.8711883766574));
#22189=CARTESIAN_POINT('Ctrl Pts',(-1.00106258513422,-0.615242280715573,
-27.8811826954638));
#22190=CARTESIAN_POINT('Ctrl Pts',(-1.11384179304919,-0.367478577023206,
-27.8997347755227));
#22191=CARTESIAN_POINT('Ctrl Pts',(-1.1608022340359,-0.21786014940718,-27.9102058476455));
#22192=CARTESIAN_POINT('Ctrl Pts',(-1.17073802586279,0.10974099037791,-27.932588142241));
#22193=CARTESIAN_POINT('Ctrl Pts',(-1.14631134349229,0.25873940171332,-27.9426949789175));
#22194=CARTESIAN_POINT('Ctrl Pts',(-1.05211545721986,0.519720702111875,
-27.9616070155807));
#22195=CARTESIAN_POINT('Ctrl Pts',(-0.980813909196912,0.657035707477414,
-27.9719512436533));
#22196=CARTESIAN_POINT('Ctrl Pts',(-0.76021498715122,0.897029079457893,
-27.9942053903235));
#22197=CARTESIAN_POINT('Ctrl Pts',(-0.637209668148432,0.98762997462939,
-28.0044244648287));
#22198=CARTESIAN_POINT('Ctrl Pts',(-0.361409610940396,1.1201917160955,-28.0252878896824));
#22199=CARTESIAN_POINT('Ctrl Pts',(-0.215278414855001,1.15709812005245,
-28.0353869605628));
#22200=CARTESIAN_POINT('Ctrl Pts',(0.0874619436173592,1.17256057451052,
-28.0560735394642));
#22201=CARTESIAN_POINT('Ctrl Pts',(0.240409186122314,1.15078313340772,-28.0664017047748));
#22202=CARTESIAN_POINT('Ctrl Pts',(0.529578637445944,1.0512078955982,-28.0872616586405));
#22203=CARTESIAN_POINT('Ctrl Pts',(0.661558687757645,0.973611514425888,
-28.0975228583036));
#22204=CARTESIAN_POINT('Ctrl Pts',(0.890301982635324,0.768087674628803,
-28.11849818603));
#22205=CARTESIAN_POINT('Ctrl Pts',(0.984380269778329,0.643433278699844,
-28.1289345247244));
#22206=CARTESIAN_POINT('Ctrl Pts',(1.11708899258416,0.370182100385531,-28.1496645175383));
#22207=CARTESIAN_POINT('Ctrl Pts',(1.1553273946675,0.224988277345117,-28.159726623677));
#22208=CARTESIAN_POINT('Ctrl Pts',(1.172855145901,-0.0847008837209511,-28.1808754349718));
#22209=CARTESIAN_POINT('Ctrl Pts',(1.1515608225355,-0.240698826534231,-28.1913957171289));
#22210=CARTESIAN_POINT('Ctrl Pts',(1.04434540511724,-0.549317232093467,
-28.2137019191629));
#22211=CARTESIAN_POINT('Ctrl Pts',(0.959484992736289,-0.675114426088475,
-28.2238544504272));
#22212=CARTESIAN_POINT('Ctrl Pts',(0.772891490596436,-0.886382061655959,
-28.243066946934));
#22213=CARTESIAN_POINT('Ctrl Pts',(0.647394806280094,-0.982811598955698,
-28.2536437922866));
#22214=CARTESIAN_POINT('Ctrl Pts',(0.352078935195833,-1.12632096557171,
-28.2760689537009));
#22215=CARTESIAN_POINT('Ctrl Pts',(0.203531273591151,-1.15448321757536,
-28.2861776722252));
#22216=CARTESIAN_POINT('Ctrl Pts',(-0.0714241877483557,-1.17399633203817,
-28.3049627703414));
#22217=CARTESIAN_POINT('Ctrl Pts',(-0.228920209503697,-1.15478736582145,
-28.315569939304));
#22218=CARTESIAN_POINT('Ctrl Pts',(-0.513628372088781,-1.05793609215418,
-28.3361124264558));
#22219=CARTESIAN_POINT('Ctrl Pts',(-0.641616188680906,-0.984288752852638,
-28.3460123069916));
#22220=CARTESIAN_POINT('Ctrl Pts',(-0.849977439951128,-0.80831404632089,
-28.3645976950093));
#22221=CARTESIAN_POINT('Ctrl Pts',(-0.957339906864927,-0.690999683619937,
-28.3752142761587));
#22222=CARTESIAN_POINT('Ctrl Pts',(-1.1049312931433,-0.402369072521088,
-28.3973572083034));
#22223=CARTESIAN_POINT('Ctrl Pts',(-1.14605683889198,-0.259178152412038,
-28.4073382677248));
#22224=CARTESIAN_POINT('Ctrl Pts',(-1.17276985827545,0.0110285923521394,
-28.425842402092));
#22225=CARTESIAN_POINT('Ctrl Pts',(-1.16912240263032,0.168062342229981,
-28.4363291398125));
#22226=CARTESIAN_POINT('Ctrl Pts',(-1.07270922365842,0.481638865043275,
-28.4587333398723));
#22227=CARTESIAN_POINT('Ctrl Pts',(-1.00160136178626,0.614592612986852,
-28.4688267952487));
#22228=CARTESIAN_POINT('Ctrl Pts',(-0.828634365706037,0.830823604335824,
-28.4877001470211));
#22229=CARTESIAN_POINT('Ctrl Pts',(-0.716809839346193,0.938087220208765,
-28.4980583573749));
#22230=CARTESIAN_POINT('Ctrl Pts',(-0.430495445216648,1.0941967825346,-28.5203226326978));
#22231=CARTESIAN_POINT('Ctrl Pts',(-0.285049692098074,1.14022956352786,
-28.5305283149134));
#22232=CARTESIAN_POINT('Ctrl Pts',(0.0172110229777963,1.17670768237989,
-28.5512852188951));
#22233=CARTESIAN_POINT('Ctrl Pts',(0.16754953289506,1.16518146736364,-28.5613874349407));
#22234=CARTESIAN_POINT('Ctrl Pts',(0.460372021004377,1.08196013685234,-28.5821622194308));
#22235=CARTESIAN_POINT('Ctrl Pts',(0.597984012909007,1.01216444806352,-28.5924781493724));
#22236=CARTESIAN_POINT('Ctrl Pts',(0.839559983040483,0.824971631429336,
-28.6133221362559));
#22237=CARTESIAN_POINT('Ctrl Pts',(0.939712152246731,0.708957308483833,
-28.6235939550189));
#22238=CARTESIAN_POINT('Ctrl Pts',(1.09008227583706,0.440659717710434,-28.6445727801413));
#22239=CARTESIAN_POINT('Ctrl Pts',(1.13895411984997,0.292465491874021,-28.6550002344119));
#22240=CARTESIAN_POINT('Ctrl Pts',(1.16850615302418,0.0569319254104148,
-28.6712003632538));
#22241=CARTESIAN_POINT('Ctrl Pts',(1.16987757186606,-0.0278535081972872,
-28.6769601814215));
#22242=CARTESIAN_POINT('Ctrl Pts',(1.15309370880968,-0.19690061877361,-28.6885666806711));
#22243=CARTESIAN_POINT('Ctrl Pts',(1.13536757906777,-0.28003883922839,-28.694335360097));
#22244=CARTESIAN_POINT('Ctrl Pts',(1.1090896887684,-0.360362786612186,-28.7000986778144));
#22245=CARTESIAN_POINT('Ctrl Pts',(0.2042496867001,1.148974072566,-25.02357429354));
#22246=CARTESIAN_POINT('Ctrl Pts',(0.485799150132,1.098923865977,-25.04307429354));
#22247=CARTESIAN_POINT('Ctrl Pts',(1.008732028848,0.7826683203553,-25.08207429354));
#22248=CARTESIAN_POINT('Ctrl Pts',(1.273344351706,-0.09619644100725,-25.14057429354));
#22249=CARTESIAN_POINT('Ctrl Pts',(0.8799211891228,-0.9253151078751,-25.19907429354));
#22250=CARTESIAN_POINT('Ctrl Pts',(0.03209325983472,-1.276509118266,-25.25757429354));
#22251=CARTESIAN_POINT('Ctrl Pts',(-0.8323352153661,-0.9683609251365,-25.31607429354));
#22252=CARTESIAN_POINT('Ctrl Pts',(-1.266842465797,-0.1600395162514,-25.37457429354));
#22253=CARTESIAN_POINT('Ctrl Pts',(-1.047006449646,0.7309452405402,-25.43307429354));
#22254=CARTESIAN_POINT('Ctrl Pts',(-0.2863739154552,1.244384671677,-25.49157429354));
#22255=CARTESIAN_POINT('Ctrl Pts',(0.6221753352776,1.115078965991,-25.55007429354));
#22256=CARTESIAN_POINT('Ctrl Pts',(1.209360820682,0.4098166204233,-25.60857429354));
#22257=CARTESIAN_POINT('Ctrl Pts',(1.171891533923,-0.5071227513611,-25.66707429354));
#22258=CARTESIAN_POINT('Ctrl Pts',(0.5291209893422,-1.162124878025,-25.72557429354));
#22259=CARTESIAN_POINT('Ctrl Pts',(-0.3869492533009,-1.216870382867,-25.78407429354));
#22260=CARTESIAN_POINT('Ctrl Pts',(-1.103153839379,-0.6430823119665,-25.84257429354));
#22261=CARTESIAN_POINT('Ctrl Pts',(-1.249561315594,0.262868354685,-25.90107429354));
#22262=CARTESIAN_POINT('Ctrl Pts',(-0.7505498113574,1.033043190765,-25.95957429354));
#22263=CARTESIAN_POINT('Ctrl Pts',(0.1361330203811,1.269634220587,-26.01807429354));
#22264=CARTESIAN_POINT('Ctrl Pts',(0.9525009070881,0.850438284238,-26.07657429354));
#22265=CARTESIAN_POINT('Ctrl Pts',(1.276886402343,-0.00802301942994,-26.13507429354));
#22266=CARTESIAN_POINT('Ctrl Pts',(0.9417390602074,-0.8623403017182,-26.19357429354));
#22267=CARTESIAN_POINT('Ctrl Pts',(0.1201679976972,-1.271244628134,-26.25207429354));
#22268=CARTESIAN_POINT('Ctrl Pts',(-0.7634718132617,-1.023530188774,-26.31057429354));
#22269=CARTESIAN_POINT('Ctrl Pts',(-1.252765868871,-0.2471455563325,-26.36907429354));
#22270=CARTESIAN_POINT('Ctrl Pts',(-1.094985744155,0.6568937894785,-26.42757429354));
#22271=CARTESIAN_POINT('Ctrl Pts',(-0.3716274479098,1.221636807823,-26.48607429354));
#22272=CARTESIAN_POINT('Ctrl Pts',(0.5436824759227,1.155383851922,-26.54457429354));
#22273=CARTESIAN_POINT('Ctrl Pts',(1.178171694542,0.49235784776,-26.60307429354));
#22274=CARTESIAN_POINT('Ctrl Pts',(1.204114952343,-0.4249855149138,-26.66157429354));
#22275=CARTESIAN_POINT('Ctrl Pts',(0.6081163618214,-1.122792874227,-26.72007429354));
#22276=CARTESIAN_POINT('Ctrl Pts',(-0.3019967923042,-1.240748778247,-26.77857429354));
#22277=CARTESIAN_POINT('Ctrl Pts',(-1.056077145856,-0.7175033572827,-26.83707429354));
#22278=CARTESIAN_POINT('Ctrl Pts',(-1.195258896894,-0.1224362972325,-26.87607429354));
#22279=CARTESIAN_POINT('Ctrl Pts',(-1.155855903054,0.1607995190315,-26.89557429354));
#22280=CARTESIAN_POINT('Ctrl Pts',(0.2042496867001,1.148974072566,-25.08906643118));
#22281=CARTESIAN_POINT('Ctrl Pts',(0.485799150132,1.098923865977,-25.10856643118));
#22282=CARTESIAN_POINT('Ctrl Pts',(1.008732028848,0.7826683203553,-25.14756643118));
#22283=CARTESIAN_POINT('Ctrl Pts',(1.273344351706,-0.09619644100725,-25.20606643118));
#22284=CARTESIAN_POINT('Ctrl Pts',(0.8799211891228,-0.9253151078751,-25.26456643118));
#22285=CARTESIAN_POINT('Ctrl Pts',(0.03209325983472,-1.276509118266,-25.32306643118));
#22286=CARTESIAN_POINT('Ctrl Pts',(-0.8323352153661,-0.9683609251365,-25.38156643118));
#22287=CARTESIAN_POINT('Ctrl Pts',(-1.266842465797,-0.1600395162514,-25.44006643118));
#22288=CARTESIAN_POINT('Ctrl Pts',(-1.047006449646,0.7309452405402,-25.49856643118));
#22289=CARTESIAN_POINT('Ctrl Pts',(-0.2863739154552,1.244384671677,-25.55706643118));
#22290=CARTESIAN_POINT('Ctrl Pts',(0.6221753352776,1.115078965991,-25.61556643118));
#22291=CARTESIAN_POINT('Ctrl Pts',(1.209360820682,0.4098166204233,-25.67406643118));
#22292=CARTESIAN_POINT('Ctrl Pts',(1.171891533923,-0.5071227513611,-25.73256643118));
#22293=CARTESIAN_POINT('Ctrl Pts',(0.5291209893422,-1.162124878025,-25.79106643118));
#22294=CARTESIAN_POINT('Ctrl Pts',(-0.3869492533009,-1.216870382867,-25.84956643118));
#22295=CARTESIAN_POINT('Ctrl Pts',(-1.103153839379,-0.6430823119665,-25.90806643118));
#22296=CARTESIAN_POINT('Ctrl Pts',(-1.249561315594,0.262868354685,-25.96656643118));
#22297=CARTESIAN_POINT('Ctrl Pts',(-0.7505498113574,1.033043190765,-26.02506643118));
#22298=CARTESIAN_POINT('Ctrl Pts',(0.1361330203811,1.269634220587,-26.08356643118));
#22299=CARTESIAN_POINT('Ctrl Pts',(0.9525009070881,0.850438284238,-26.14206643118));
#22300=CARTESIAN_POINT('Ctrl Pts',(1.276886402343,-0.00802301942994,-26.20056643118));
#22301=CARTESIAN_POINT('Ctrl Pts',(0.9417390602074,-0.8623403017182,-26.25906643118));
#22302=CARTESIAN_POINT('Ctrl Pts',(0.1201679976972,-1.271244628134,-26.31756643118));
#22303=CARTESIAN_POINT('Ctrl Pts',(-0.7634718132617,-1.023530188774,-26.37606643118));
#22304=CARTESIAN_POINT('Ctrl Pts',(-1.252765868871,-0.2471455563325,-26.43456643118));
#22305=CARTESIAN_POINT('Ctrl Pts',(-1.094985744155,0.6568937894785,-26.49306643118));
#22306=CARTESIAN_POINT('Ctrl Pts',(-0.3716274479098,1.221636807823,-26.55156643118));
#22307=CARTESIAN_POINT('Ctrl Pts',(0.5436824759227,1.155383851922,-26.61006643118));
#22308=CARTESIAN_POINT('Ctrl Pts',(1.178171694542,0.49235784776,-26.66856643118));
#22309=CARTESIAN_POINT('Ctrl Pts',(1.204114952343,-0.4249855149138,-26.72706643118));
#22310=CARTESIAN_POINT('Ctrl Pts',(0.6081163618214,-1.122792874227,-26.78556643118));
#22311=CARTESIAN_POINT('Ctrl Pts',(-0.3019967923042,-1.240748778247,-26.84406643118));
#22312=CARTESIAN_POINT('Ctrl Pts',(-1.056077145856,-0.7175033572827,-26.90256643118));
#22313=CARTESIAN_POINT('Ctrl Pts',(-1.195258896894,-0.1224362972325,-26.94156643118));
#22314=CARTESIAN_POINT('Ctrl Pts',(-1.155855903054,0.1607995190315,-26.96106643118));
#22315=CARTESIAN_POINT('Ctrl Pts',(0.2042496867001,1.148974072566,-25.15455856882));
#22316=CARTESIAN_POINT('Ctrl Pts',(0.485799150132,1.098923865977,-25.17405856882));
#22317=CARTESIAN_POINT('Ctrl Pts',(1.008732028848,0.7826683203553,-25.21305856882));
#22318=CARTESIAN_POINT('Ctrl Pts',(1.273344351706,-0.09619644100725,-25.27155856882));
#22319=CARTESIAN_POINT('Ctrl Pts',(0.8799211891228,-0.9253151078751,-25.33005856882));
#22320=CARTESIAN_POINT('Ctrl Pts',(0.03209325983473,-1.276509118266,-25.38855856882));
#22321=CARTESIAN_POINT('Ctrl Pts',(-0.8323352153661,-0.9683609251365,-25.44705856882));
#22322=CARTESIAN_POINT('Ctrl Pts',(-1.266842465797,-0.1600395162514,-25.50555856882));
#22323=CARTESIAN_POINT('Ctrl Pts',(-1.047006449646,0.7309452405402,-25.56405856882));
#22324=CARTESIAN_POINT('Ctrl Pts',(-0.2863739154552,1.244384671677,-25.62255856882));
#22325=CARTESIAN_POINT('Ctrl Pts',(0.6221753352776,1.115078965991,-25.68105856882));
#22326=CARTESIAN_POINT('Ctrl Pts',(1.209360820682,0.4098166204233,-25.73955856882));
#22327=CARTESIAN_POINT('Ctrl Pts',(1.171891533923,-0.5071227513611,-25.79805856882));
#22328=CARTESIAN_POINT('Ctrl Pts',(0.5291209893422,-1.162124878025,-25.85655856882));
#22329=CARTESIAN_POINT('Ctrl Pts',(-0.3869492533009,-1.216870382867,-25.91505856882));
#22330=CARTESIAN_POINT('Ctrl Pts',(-1.103153839379,-0.6430823119665,-25.97355856882));
#22331=CARTESIAN_POINT('Ctrl Pts',(-1.249561315594,0.262868354685,-26.03205856882));
#22332=CARTESIAN_POINT('Ctrl Pts',(-0.7505498113574,1.033043190765,-26.09055856882));
#22333=CARTESIAN_POINT('Ctrl Pts',(0.1361330203811,1.269634220587,-26.14905856882));
#22334=CARTESIAN_POINT('Ctrl Pts',(0.9525009070881,0.850438284238,-26.20755856882));
#22335=CARTESIAN_POINT('Ctrl Pts',(1.276886402343,-0.008023019429937,-26.26605856882));
#22336=CARTESIAN_POINT('Ctrl Pts',(0.9417390602074,-0.8623403017182,-26.32455856882));
#22337=CARTESIAN_POINT('Ctrl Pts',(0.1201679976972,-1.271244628134,-26.38305856882));
#22338=CARTESIAN_POINT('Ctrl Pts',(-0.7634718132616,-1.023530188774,-26.44155856882));
#22339=CARTESIAN_POINT('Ctrl Pts',(-1.252765868871,-0.2471455563325,-26.50005856882));
#22340=CARTESIAN_POINT('Ctrl Pts',(-1.094985744155,0.6568937894785,-26.55855856882));
#22341=CARTESIAN_POINT('Ctrl Pts',(-0.3716274479098,1.221636807823,-26.61705856882));
#22342=CARTESIAN_POINT('Ctrl Pts',(0.5436824759227,1.155383851922,-26.67555856882));
#22343=CARTESIAN_POINT('Ctrl Pts',(1.178171694542,0.49235784776,-26.73405856882));
#22344=CARTESIAN_POINT('Ctrl Pts',(1.204114952343,-0.4249855149138,-26.79255856882));
#22345=CARTESIAN_POINT('Ctrl Pts',(0.6081163618214,-1.122792874227,-26.85105856882));
#22346=CARTESIAN_POINT('Ctrl Pts',(-0.3019967923042,-1.240748778247,-26.90955856882));
#22347=CARTESIAN_POINT('Ctrl Pts',(-1.056077145856,-0.7175033572827,-26.96805856882));
#22348=CARTESIAN_POINT('Ctrl Pts',(-1.195258896894,-0.1224362972325,-27.00705856882));
#22349=CARTESIAN_POINT('Ctrl Pts',(-1.155855903054,0.1607995190315,-27.02655856882));
#22350=CARTESIAN_POINT('Ctrl Pts',(0.2042496867001,1.148974072566,-25.22005070646));
#22351=CARTESIAN_POINT('Ctrl Pts',(0.485799150132,1.098923865977,-25.23955070646));
#22352=CARTESIAN_POINT('Ctrl Pts',(1.008732028848,0.7826683203553,-25.27855070646));
#22353=CARTESIAN_POINT('Ctrl Pts',(1.273344351706,-0.09619644100725,-25.33705070646));
#22354=CARTESIAN_POINT('Ctrl Pts',(0.8799211891228,-0.9253151078751,-25.39555070646));
#22355=CARTESIAN_POINT('Ctrl Pts',(0.03209325983472,-1.276509118266,-25.45405070646));
#22356=CARTESIAN_POINT('Ctrl Pts',(-0.8323352153661,-0.9683609251365,-25.51255070646));
#22357=CARTESIAN_POINT('Ctrl Pts',(-1.266842465797,-0.1600395162514,-25.57105070646));
#22358=CARTESIAN_POINT('Ctrl Pts',(-1.047006449646,0.7309452405402,-25.62955070646));
#22359=CARTESIAN_POINT('Ctrl Pts',(-0.2863739154552,1.244384671677,-25.68805070646));
#22360=CARTESIAN_POINT('Ctrl Pts',(0.6221753352776,1.115078965991,-25.74655070646));
#22361=CARTESIAN_POINT('Ctrl Pts',(1.209360820682,0.4098166204233,-25.80505070646));
#22362=CARTESIAN_POINT('Ctrl Pts',(1.171891533923,-0.5071227513611,-25.86355070646));
#22363=CARTESIAN_POINT('Ctrl Pts',(0.5291209893422,-1.162124878025,-25.92205070646));
#22364=CARTESIAN_POINT('Ctrl Pts',(-0.3869492533009,-1.216870382867,-25.98055070646));
#22365=CARTESIAN_POINT('Ctrl Pts',(-1.103153839379,-0.6430823119665,-26.03905070646));
#22366=CARTESIAN_POINT('Ctrl Pts',(-1.249561315594,0.262868354685,-26.09755070646));
#22367=CARTESIAN_POINT('Ctrl Pts',(-0.7505498113574,1.033043190765,-26.15605070646));
#22368=CARTESIAN_POINT('Ctrl Pts',(0.1361330203811,1.269634220587,-26.21455070646));
#22369=CARTESIAN_POINT('Ctrl Pts',(0.9525009070881,0.850438284238,-26.27305070646));
#22370=CARTESIAN_POINT('Ctrl Pts',(1.276886402343,-0.008023019429937,-26.33155070646));
#22371=CARTESIAN_POINT('Ctrl Pts',(0.9417390602074,-0.8623403017182,-26.39005070646));
#22372=CARTESIAN_POINT('Ctrl Pts',(0.1201679976972,-1.271244628134,-26.44855070646));
#22373=CARTESIAN_POINT('Ctrl Pts',(-0.7634718132616,-1.023530188774,-26.50705070646));
#22374=CARTESIAN_POINT('Ctrl Pts',(-1.252765868871,-0.2471455563325,-26.56555070646));
#22375=CARTESIAN_POINT('Ctrl Pts',(-1.094985744155,0.6568937894785,-26.62405070646));
#22376=CARTESIAN_POINT('Ctrl Pts',(-0.3716274479098,1.221636807823,-26.68255070646));
#22377=CARTESIAN_POINT('Ctrl Pts',(0.5436824759227,1.155383851922,-26.74105070646));
#22378=CARTESIAN_POINT('Ctrl Pts',(1.178171694542,0.49235784776,-26.79955070646));
#22379=CARTESIAN_POINT('Ctrl Pts',(1.204114952343,-0.4249855149138,-26.85805070646));
#22380=CARTESIAN_POINT('Ctrl Pts',(0.6081163618214,-1.122792874227,-26.91655070646));
#22381=CARTESIAN_POINT('Ctrl Pts',(-0.3019967923042,-1.240748778247,-26.97505070646));
#22382=CARTESIAN_POINT('Ctrl Pts',(-1.056077145856,-0.7175033572827,-27.03355070646));
#22383=CARTESIAN_POINT('Ctrl Pts',(-1.195258896894,-0.1224362972325,-27.07255070646));
#22384=CARTESIAN_POINT('Ctrl Pts',(-1.155855903054,0.1607995190315,-27.09205070646));
#22385=CARTESIAN_POINT('',(0.685937843384214,0.944112445532598,-25.1000774755696));
#22386=CARTESIAN_POINT('',(0.685937843399239,0.94411244560349,-25.2155475173803));
#22387=CARTESIAN_POINT('',(0.6859379234404,0.9441125563889,-25.10007747308));
#22388=CARTESIAN_POINT('Ctrl Pts',(0.685456475053999,0.943446181037267,
-25.2155263221855));
#22389=CARTESIAN_POINT('Ctrl Pts',(0.753928966560715,0.893908498927705,
-25.2212896399029));
#22390=CARTESIAN_POINT('Ctrl Pts',(0.817137126651638,0.837067423340081,
-25.2270583193288));
#22391=CARTESIAN_POINT('Ctrl Pts',(0.930078955634944,0.710170745214693,
-25.2386648185784));
#22392=CARTESIAN_POINT('Ctrl Pts',(0.978805081969252,0.640771788780588,
-25.244424636746));
#22393=CARTESIAN_POINT('Ctrl Pts',(1.09334014170001,0.432850881490653,-25.260624765588));
#22394=CARTESIAN_POINT('Ctrl Pts',(1.1409083697686,0.284233085157616,-25.2710522198586));
#22395=CARTESIAN_POINT('Ctrl Pts',(1.17695775141982,-0.0212095663597187,
-25.292031044981));
#22396=CARTESIAN_POINT('Ctrl Pts',(1.16412445259043,-0.173935093258059,
-25.302302863744));
#22397=CARTESIAN_POINT('Ctrl Pts',(1.07871456427401,-0.467372055691385,
-25.3231468506275));
#22398=CARTESIAN_POINT('Ctrl Pts',(1.00840900073704,-0.604724253435656,
-25.3334627805692));
#22399=CARTESIAN_POINT('Ctrl Pts',(0.820426902272126,-0.844168464163895,
-25.3542375650593));
#22400=CARTESIAN_POINT('Ctrl Pts',(0.705575432041381,-0.941860126973701,
-25.3643397811048));
#22401=CARTESIAN_POINT('Ctrl Pts',(0.439600076520464,-1.09001309956845,
-25.3850966850864));
#22402=CARTESIAN_POINT('Ctrl Pts',(0.294874600697833,-1.13826266613819,
-25.395302367302));
#22403=CARTESIAN_POINT('Ctrl Pts',(-0.0285175083645314,-1.18025875562043,
-25.4175666426249));
#22404=CARTESIAN_POINT('Ctrl Pts',(-0.182033422095494,-1.1592094749399,
-25.4279248529788));
#22405=CARTESIAN_POINT('Ctrl Pts',(-0.449064049193832,-1.08594237765718,
-25.4467982047514));
#22406=CARTESIAN_POINT('Ctrl Pts',(-0.58473977016012,-1.02017668863555,
-25.4568916601279));
#22407=CARTESIAN_POINT('Ctrl Pts',(-0.847055326004509,-0.823158197369117,
-25.4792958601879));
#22408=CARTESIAN_POINT('Ctrl Pts',(-0.942308301897876,-0.698259145664254,
-25.4897825979083));
#22409=CARTESIAN_POINT('Ctrl Pts',(-1.07952055488772,-0.463955778317708,
-25.5082867322755));
#22410=CARTESIAN_POINT('Ctrl Pts',(-1.1304148005763,-0.32393890122586,-25.5182677916968));
#22411=CARTESIAN_POINT('Ctrl Pts',(-1.18066367741776,-0.00367979153001349,
-25.5404107238414));
#22412=CARTESIAN_POINT('Ctrl Pts',(-1.16276126940395,0.154335596280979,
-25.5510273049907));
#22413=CARTESIAN_POINT('Ctrl Pts',(-1.09762881343295,0.419173795090977,
-25.5696126930082));
#22414=CARTESIAN_POINT('Ctrl Pts',(-1.03737331464878,0.553985095242714,
-25.579512573544));
#22415=CARTESIAN_POINT('Ctrl Pts',(-0.863967323007216,0.799686680741356,
-25.6000550606958));
#22416=CARTESIAN_POINT('Ctrl Pts',(-0.74784111191472,0.907800899737537,
-25.6106622296586));
#22417=CARTESIAN_POINT('Ctrl Pts',(-0.513927950087508,1.05362922373647,
-25.6294473277748));
#22418=CARTESIAN_POINT('Ctrl Pts',(-0.377197010975904,1.11815960801924,
-25.6395560462991));
#22419=CARTESIAN_POINT('Ctrl Pts',(-0.0539287632978119,1.17564040536612,
-25.6619812077133));
#22420=CARTESIAN_POINT('Ctrl Pts',(0.104280046962069,1.17139237118361,-25.6725580530658));
#22421=CARTESIAN_POINT('Ctrl Pts',(0.379417361706695,1.11015017237935,-25.6917705495726));
#22422=CARTESIAN_POINT('Ctrl Pts',(0.522012612882813,1.05825780349353,-25.7019230808369));
#22423=CARTESIAN_POINT('Ctrl Pts',(0.790153055006959,0.871599909795858,
-25.7242292828709));
#22424=CARTESIAN_POINT('Ctrl Pts',(0.899073814666876,0.7579114122043,-25.7347495650281));
#22425=CARTESIAN_POINT('Ctrl Pts',(1.06692428771505,0.497065064247596,-25.7558983763229));
#22426=CARTESIAN_POINT('Ctrl Pts',(1.12133155849896,0.357124825114038,-25.7659604824616));
#22427=CARTESIAN_POINT('Ctrl Pts',(1.17458095923193,0.058055748008961,-25.7866904752754));
#22428=CARTESIAN_POINT('Ctrl Pts',(1.17174004169197,-0.0980896064647793,
-25.7971268139698));
#22429=CARTESIAN_POINT('Ctrl Pts',(1.10748671081373,-0.398813820899846,
-25.8181021416962));
#22430=CARTESIAN_POINT('Ctrl Pts',(1.04632261567736,-0.539166539140376,
-25.8283633413593));
#22431=CARTESIAN_POINT('Ctrl Pts',(0.870908471580301,-0.789694137648766,
-25.849223295225));
#22432=CARTESIAN_POINT('Ctrl Pts',(0.759972011863893,-0.897212591118109,
-25.8595514605356));
#22433=CARTESIAN_POINT('Ctrl Pts',(0.505961314281782,-1.06264952067059,
-25.880238039437));
#22434=CARTESIAN_POINT('Ctrl Pts',(0.366045653279312,-1.11868537462692,
-25.8903371103175));
#22435=CARTESIAN_POINT('Ctrl Pts',(0.0650008832967905,-1.17355187918509,
-25.9112005351713));
#22436=CARTESIAN_POINT('Ctrl Pts',(-0.0877663802010868,-1.17255492774913,
-25.9214196096765));
#22437=CARTESIAN_POINT('Ctrl Pts',(-0.407299221774617,-1.10806100432969,
-25.9436737563468));
#22438=CARTESIAN_POINT('Ctrl Pts',(-0.545695120922654,-1.03888082979981,
-25.9540179844193));
#22439=CARTESIAN_POINT('Ctrl Pts',(-0.775302153215706,-0.883109475340792,
-25.9729300210824));
#22440=CARTESIAN_POINT('Ctrl Pts',(-0.882642823167725,-0.776924872095221,
-25.9830368577589));
#22441=CARTESIAN_POINT('Ctrl Pts',(-1.06716371732725,-0.506049870726424,
-26.0054191523544));
#22442=CARTESIAN_POINT('Ctrl Pts',(-1.11711542772957,-0.357403365460102,
-26.0158902244773));
#22443=CARTESIAN_POINT('Ctrl Pts',(-1.17150698299789,-0.0906683634061106,
-26.0344423045363));
#22444=CARTESIAN_POINT('Ctrl Pts',(-1.17445379308505,0.0584942439088762,
-26.0444366233427));
#22445=CARTESIAN_POINT('Ctrl Pts',(-1.11587167131851,0.393273107848679,
-26.067650805626));
#22446=CARTESIAN_POINT('Ctrl Pts',(-1.04031459198801,0.537652390835965,
-26.0784973022942));
#22447=CARTESIAN_POINT('Ctrl Pts',(-0.903532701937386,0.751044251113647,
-26.0957700105568));
#22448=CARTESIAN_POINT('Ctrl Pts',(-0.803121960948684,0.858973369535563,
-26.1056531858431));
#22449=CARTESIAN_POINT('Ctrl Pts',(-0.568753885931908,1.02925174324195,
-26.1254418679969));
#22450=CARTESIAN_POINT('Ctrl Pts',(-0.435078569175414,1.09139610098497,
-26.1353250432865));
#22451=CARTESIAN_POINT('Ctrl Pts',(-0.18986292138628,1.15554169754148,-26.1525977515492));
#22452=CARTESIAN_POINT('Ctrl Pts',(-0.0292016419244966,1.18278509811256,
-26.1634442482175));
#22453=CARTESIAN_POINT('Ctrl Pts',(0.307294849336613,1.13504764844191,-26.1866584305008));
#22454=CARTESIAN_POINT('Ctrl Pts',(0.448246304615041,1.08615128492058,-26.1966527493071));
#22455=CARTESIAN_POINT('Ctrl Pts',(0.685118451514085,0.951996193221822,
-26.2152048293661));
#22456=CARTESIAN_POINT('Ctrl Pts',(0.811053751559603,0.858554997261884,
-26.2256759014889));
#22457=CARTESIAN_POINT('Ctrl Pts',(1.01165109460014,0.599360219704633,-26.2480581960845));
#22458=CARTESIAN_POINT('Ctrl Pts',(1.07946856224422,0.464460329139464,-26.2581650327611));
#22459=CARTESIAN_POINT('Ctrl Pts',(1.15666344894798,0.197955069125299,-26.2770770694244));
#22460=CARTESIAN_POINT('Ctrl Pts',(1.17969101994448,0.0449548978084111,
-26.287421297497));
#22461=CARTESIAN_POINT('Ctrl Pts',(1.14228730776675,-0.278868611711105,
-26.3096754441672));
#22462=CARTESIAN_POINT('Ctrl Pts',(1.09602778432128,-0.424466988073717,
-26.3198945186723));
#22463=CARTESIAN_POINT('Ctrl Pts',(0.950818687642312,-0.693822895932095,
-26.3407579435259));
#22464=CARTESIAN_POINT('Ctrl Pts',(0.854289106561841,-0.809574565893386,
-26.3508570144063));
#22465=CARTESIAN_POINT('Ctrl Pts',(0.618455614369187,-1.00003027230849,
-26.3715435933077));
#22466=CARTESIAN_POINT('Ctrl Pts',(0.481918237226907,-1.07231208588558,
-26.3818717586183));
#22467=CARTESIAN_POINT('Ctrl Pts',(0.189446380573906,-1.16172356518028,
-26.402731712484));
#22468=CARTESIAN_POINT('Ctrl Pts',(0.0370622684688799,-1.17652270127989,
-26.4129929121471));
#22469=CARTESIAN_POINT('Ctrl Pts',(-0.268798826463713,-1.14470235742468,
-26.4339682398734));
#22470=CARTESIAN_POINT('Ctrl Pts',(-0.418179775124505,-1.09915266243818,
-26.4444045785679));
#22471=CARTESIAN_POINT('Ctrl Pts',(-0.686156399960757,-0.956092045564685,
-26.4651345713817));
#22472=CARTESIAN_POINT('Ctrl Pts',(-0.802434704990725,-0.861103744062606,
-26.4751966775203));
#22473=CARTESIAN_POINT('Ctrl Pts',(-0.998645675280886,-0.620862503467603,
-26.496345488815));
#22474=CARTESIAN_POINT('Ctrl Pts',(-1.07311149596802,-0.482141027412342,
-26.5068657709721));
#22475=CARTESIAN_POINT('Ctrl Pts',(-1.16777374859158,-0.169443851360786,
-26.529171973006));
#22476=CARTESIAN_POINT('Ctrl Pts',(-1.17306196823584,-0.0177920846727423,
-26.5393245042704));
#22477=CARTESIAN_POINT('Ctrl Pts',(-1.146284654438,0.262803931594615,-26.5585370007772));
#22478=CARTESIAN_POINT('Ctrl Pts',(-1.10143556399854,0.414582166282618,
-26.5691138461298));
#22479=CARTESIAN_POINT('Ctrl Pts',(-0.946872694845563,0.704265996517479,
-26.591539007544));
#22480=CARTESIAN_POINT('Ctrl Pts',(-0.843248468532132,0.814363861741629,
-26.6016477260684));
#22481=CARTESIAN_POINT('Ctrl Pts',(-0.632274348520049,0.991765068167514,
-26.6204328241844));
#22482=CARTESIAN_POINT('Ctrl Pts',(-0.493566643319621,1.06879852693624,
-26.6310399931471));
#22483=CARTESIAN_POINT('Ctrl Pts',(-0.206305151023379,1.15779145978755,
-26.6515824802988));
#22484=CARTESIAN_POINT('Ctrl Pts',(-0.059472012414958,1.17343886176815,
-26.6614823608346));
#22485=CARTESIAN_POINT('Ctrl Pts',(0.212531118107488,1.1535440042497,-26.6800677488523));
#22486=CARTESIAN_POINT('Ctrl Pts',(0.368344830676723,1.12174076584227,-26.6906843300017));
#22487=CARTESIAN_POINT('Ctrl Pts',(0.657401586964124,0.974985736585933,
-26.7128272621465));
#22488=CARTESIAN_POINT('Ctrl Pts',(0.774838363480133,0.883314838061018,
-26.722808321568));
#22489=CARTESIAN_POINT('Ctrl Pts',(0.955273189774572,0.680414508389969,
-26.7413124559353));
#22490=CARTESIAN_POINT('Ctrl Pts',(1.04462445846149,0.551227615412156,-26.7517991936558));
#22491=CARTESIAN_POINT('Ctrl Pts',(1.15094021376586,0.240868634693924,-26.7742033937157));
#22492=CARTESIAN_POINT('Ctrl Pts',(1.17156099735573,0.091510640611728,-26.784296849092));
#22493=CARTESIAN_POINT('Ctrl Pts',(1.15872514586447,-0.185091355529303,
-26.8031702008644));
#22494=CARTESIAN_POINT('Ctrl Pts',(1.13130517516905,-0.337598251087985,
-26.8135284112181));
#22495=CARTESIAN_POINT('Ctrl Pts',(0.991430863060781,-0.632184918383263,
-26.8357926865412));
#22496=CARTESIAN_POINT('Ctrl Pts',(0.900820166817858,-0.754917089197195,
-26.8459983687569));
#22497=CARTESIAN_POINT('Ctrl Pts',(0.677727411882154,-0.962092897940218,
-26.8667552727386));
#22498=CARTESIAN_POINT('Ctrl Pts',(0.549326063249094,-1.04113475309212,
-26.8768574887843));
#22499=CARTESIAN_POINT('Ctrl Pts',(0.263511423283125,-1.14592402246405,
-26.8976322732743));
#22500=CARTESIAN_POINT('Ctrl Pts',(0.111156106659097,-1.17034442347985,
-26.9079482032157));
#22501=CARTESIAN_POINT('Ctrl Pts',(-0.194312135562308,-1.16089704614949,
-26.9287921900991));
#22502=CARTESIAN_POINT('Ctrl Pts',(-0.343528450555829,-1.12590745534024,
-26.939064008862));
#22503=CARTESIAN_POINT('Ctrl Pts',(-0.622881803069089,-0.997235485886526,
-26.9600428339845));
#22504=CARTESIAN_POINT('Ctrl Pts',(-0.749526335843654,-0.906069987879729,
-26.9704702882552));
#22505=CARTESIAN_POINT('Ctrl Pts',(-0.911877589686957,-0.732889579140318,
-26.9866704170972));
#22506=CARTESIAN_POINT('Ctrl Pts',(-0.962822718320104,-0.665102822246633,
-26.9924302352649));
#22507=CARTESIAN_POINT('Ctrl Pts',(-1.04860765672717,-0.518475580504917,
-27.0040367304977));
#22508=CARTESIAN_POINT('Ctrl Pts',(-1.08313431805629,-0.440796246967627,
-27.009805405914));
#22509=CARTESIAN_POINT('Ctrl Pts',(-1.10908828377811,-0.360367111878606,
-27.0155687196296));
#22510=CARTESIAN_POINT('Ctrl Pts',(0.685456617960072,0.943446077649226,
-25.1000562803705));
#22511=CARTESIAN_POINT('Ctrl Pts',(0.75392905450701,0.893908419840442,-25.1058195940861));
#22512=CARTESIAN_POINT('Ctrl Pts',(0.817137165739417,0.837067379422799,
-25.1115882695023));
#22513=CARTESIAN_POINT('Ctrl Pts',(0.930078955635281,0.710170745214216,
-25.1231947647351));
#22514=CARTESIAN_POINT('Ctrl Pts',(0.978805081969397,0.640771788780325,
-25.1289545829027));
#22515=CARTESIAN_POINT('Ctrl Pts',(1.09334014170002,0.432850881490647,-25.1451547117447));
#22516=CARTESIAN_POINT('Ctrl Pts',(1.1409083697686,0.284233085157607,-25.1555821660154));
#22517=CARTESIAN_POINT('Ctrl Pts',(1.17695775141982,-0.0212095663597268,
-25.1765609911379));
#22518=CARTESIAN_POINT('Ctrl Pts',(1.16412445259043,-0.173935093258066,
-25.1868328099009));
#22519=CARTESIAN_POINT('Ctrl Pts',(1.07871456427401,-0.46737205569139,-25.2076767967844));
#22520=CARTESIAN_POINT('Ctrl Pts',(1.00840900073704,-0.60472425343566,-25.217992726726));
#22521=CARTESIAN_POINT('Ctrl Pts',(0.820426902272119,-0.844168464163902,
-25.238767511216));
#22522=CARTESIAN_POINT('Ctrl Pts',(0.705575432041372,-0.941860126973706,
-25.2488697272616));
#22523=CARTESIAN_POINT('Ctrl Pts',(0.439600076520457,-1.09001309956845,
-25.2696266312433));
#22524=CARTESIAN_POINT('Ctrl Pts',(0.294874600697824,-1.13826266613819,
-25.2798323134589));
#22525=CARTESIAN_POINT('Ctrl Pts',(-0.0285175083645393,-1.18025875562043,
-25.3020965887819));
#22526=CARTESIAN_POINT('Ctrl Pts',(-0.182033422095502,-1.1592094749399,
-25.3124547991358));
#22527=CARTESIAN_POINT('Ctrl Pts',(-0.449064049193836,-1.08594237765718,
-25.3313281509083));
#22528=CARTESIAN_POINT('Ctrl Pts',(-0.584739770160119,-1.02017668863555,
-25.3414216062847));
#22529=CARTESIAN_POINT('Ctrl Pts',(-0.847055326004502,-0.823158197369123,
-25.3638258063445));
#22530=CARTESIAN_POINT('Ctrl Pts',(-0.942308301897868,-0.698259145664264,
-25.3743125440648));
#22531=CARTESIAN_POINT('Ctrl Pts',(-1.07952055488771,-0.463955778317722,
-25.392816678432));
#22532=CARTESIAN_POINT('Ctrl Pts',(-1.1304148005763,-0.323938901225872,
-25.4027977378532));
#22533=CARTESIAN_POINT('Ctrl Pts',(-1.18066367741776,-0.00367979152997945,
-25.4249406699978));
#22534=CARTESIAN_POINT('Ctrl Pts',(-1.16276126940394,0.154335596281021,
-25.4355572511473));
#22535=CARTESIAN_POINT('Ctrl Pts',(-1.09762881343295,0.419173795090975,
-25.4541426391649));
#22536=CARTESIAN_POINT('Ctrl Pts',(-1.03737331464878,0.553985095242714,
-25.4640425197008));
#22537=CARTESIAN_POINT('Ctrl Pts',(-0.863967323007212,0.799686680741361,
-25.4845850068527));
#22538=CARTESIAN_POINT('Ctrl Pts',(-0.747841111914714,0.907800899737542,
-25.4951921758154));
#22539=CARTESIAN_POINT('Ctrl Pts',(-0.513927950087493,1.05362922373647,
-25.5139772739317));
#22540=CARTESIAN_POINT('Ctrl Pts',(-0.377197010975882,1.11815960801925,
-25.5240859924561));
#22541=CARTESIAN_POINT('Ctrl Pts',(-0.0539287632977854,1.17564040536612,
-25.5465111538705));
#22542=CARTESIAN_POINT('Ctrl Pts',(0.104280046962098,1.1713923711836,-25.5570879992231));
#22543=CARTESIAN_POINT('Ctrl Pts',(0.37941736170672,1.11015017237934,-25.5763004957299));
#22544=CARTESIAN_POINT('Ctrl Pts',(0.522012612882833,1.05825780349352,-25.5864530269942));
#22545=CARTESIAN_POINT('Ctrl Pts',(0.790153055006974,0.871599909795844,
-25.608759229028));
#22546=CARTESIAN_POINT('Ctrl Pts',(0.899073814666888,0.757911412204285,
-25.6192795111851));
#22547=CARTESIAN_POINT('Ctrl Pts',(1.06692428771506,0.497065064247585,-25.6404283224799));
#22548=CARTESIAN_POINT('Ctrl Pts',(1.12133155849896,0.357124825114025,-25.6504904286186));
#22549=CARTESIAN_POINT('Ctrl Pts',(1.17458095923193,0.0580557480089442,
-25.6712204214325));
#22550=CARTESIAN_POINT('Ctrl Pts',(1.17174004169196,-0.0980896064647949,
-25.6816567601269));
#22551=CARTESIAN_POINT('Ctrl Pts',(1.10748671081372,-0.398813820899856,
-25.7026320878532));
#22552=CARTESIAN_POINT('Ctrl Pts',(1.04632261567736,-0.539166539140384,
-25.7128932875163));
#22553=CARTESIAN_POINT('Ctrl Pts',(0.870908471580299,-0.789694137648768,
-25.7337532413819));
#22554=CARTESIAN_POINT('Ctrl Pts',(0.759972011863892,-0.897212591118109,
-25.7440814066925));
#22555=CARTESIAN_POINT('Ctrl Pts',(0.50596131428179,-1.06264952067058,-25.7647679855938));
#22556=CARTESIAN_POINT('Ctrl Pts',(0.366045653279324,-1.11868537462692,
-25.7748670564742));
#22557=CARTESIAN_POINT('Ctrl Pts',(0.0650008832968025,-1.17355187918509,
-25.7957304813279));
#22558=CARTESIAN_POINT('Ctrl Pts',(-0.0877663802010743,-1.17255492774913,
-25.8059495558329));
#22559=CARTESIAN_POINT('Ctrl Pts',(-0.407299221774608,-1.10806100432969,
-25.8282037025031));
#22560=CARTESIAN_POINT('Ctrl Pts',(-0.545695120922647,-1.03888082979981,
-25.8385479305757));
#22561=CARTESIAN_POINT('Ctrl Pts',(-0.7753021532157,-0.883109475340797,
-25.857459967239));
#22562=CARTESIAN_POINT('Ctrl Pts',(-0.882642823167722,-0.776924872095225,
-25.8675668039156));
#22563=CARTESIAN_POINT('Ctrl Pts',(-1.06716371732725,-0.506049870726427,
-25.8899490985112));
#22564=CARTESIAN_POINT('Ctrl Pts',(-1.11711542772957,-0.357403365460107,
-25.9004201706339));
#22565=CARTESIAN_POINT('Ctrl Pts',(-1.17150698299789,-0.090668363406114,
-25.9189722506929));
#22566=CARTESIAN_POINT('Ctrl Pts',(-1.17445379308505,0.0584942439088722,
-25.9289665694992));
#22567=CARTESIAN_POINT('Ctrl Pts',(-1.11587167131851,0.393273107848691,
-25.9521807517825));
#22568=CARTESIAN_POINT('Ctrl Pts',(-1.040314591988,0.537652390835977,-25.9630272484508));
#22569=CARTESIAN_POINT('Ctrl Pts',(-0.903532701937388,0.751044251113644,
-25.9802999567134));
#22570=CARTESIAN_POINT('Ctrl Pts',(-0.803121960948686,0.858973369535562,
-25.9901831320031));
#22571=CARTESIAN_POINT('Ctrl Pts',(-0.568753885931907,1.02925174324195,
-26.0099718141569));
#22572=CARTESIAN_POINT('Ctrl Pts',(-0.435078569175412,1.09139610098497,
-26.0198549894432));
#22573=CARTESIAN_POINT('Ctrl Pts',(-0.189862921386252,1.15554169754149,
-26.0371276977058));
#22574=CARTESIAN_POINT('Ctrl Pts',(-0.0292016419244725,1.18278509811255,
-26.047974194374));
#22575=CARTESIAN_POINT('Ctrl Pts',(0.307294849336617,1.13504764844191,-26.0711883766573));
#22576=CARTESIAN_POINT('Ctrl Pts',(0.448246304615045,1.08615128492058,-26.0811826954637));
#22577=CARTESIAN_POINT('Ctrl Pts',(0.685118451514086,0.951996193221821,
-26.0997347755227));
#22578=CARTESIAN_POINT('Ctrl Pts',(0.811053751559604,0.858554997261884,
-26.1102058476456));
#22579=CARTESIAN_POINT('Ctrl Pts',(1.01165109460013,0.599360219704635,-26.1325881422411));
#22580=CARTESIAN_POINT('Ctrl Pts',(1.07946856224422,0.46446032913947,-26.1426949789175));
#22581=CARTESIAN_POINT('Ctrl Pts',(1.15666344894798,0.197955069125303,-26.1616070155807));
#22582=CARTESIAN_POINT('Ctrl Pts',(1.17969101994448,0.0449548978084168,
-26.1719512436532));
#22583=CARTESIAN_POINT('Ctrl Pts',(1.14228730776675,-0.278868611711097,
-26.1942053903234));
#22584=CARTESIAN_POINT('Ctrl Pts',(1.09602778432128,-0.42446698807371,-26.2044244648286));
#22585=CARTESIAN_POINT('Ctrl Pts',(0.950818687642318,-0.693822895932088,
-26.2252878896824));
#22586=CARTESIAN_POINT('Ctrl Pts',(0.854289106561847,-0.809574565893382,
-26.235386960563));
#22587=CARTESIAN_POINT('Ctrl Pts',(0.618455614369189,-1.00003027230849,
-26.2560735394644));
#22588=CARTESIAN_POINT('Ctrl Pts',(0.48191823722691,-1.07231208588558,-26.2664017047749));
#22589=CARTESIAN_POINT('Ctrl Pts',(0.189446380573901,-1.16172356518028,
-26.2872616586406));
#22590=CARTESIAN_POINT('Ctrl Pts',(0.0370622684688708,-1.17652270127989,
-26.2975228583036));
#22591=CARTESIAN_POINT('Ctrl Pts',(-0.268798826463742,-1.14470235742468,
-26.3184981860299));
#22592=CARTESIAN_POINT('Ctrl Pts',(-0.418179775124553,-1.09915266243818,
-26.3289345247243));
#22593=CARTESIAN_POINT('Ctrl Pts',(-0.686156399960817,-0.95609204556468,
-26.3496645175382));
#22594=CARTESIAN_POINT('Ctrl Pts',(-0.802434704990775,-0.861103744062606,
-26.3597266236769));
#22595=CARTESIAN_POINT('Ctrl Pts',(-0.99864567528091,-0.620862503467622,
-26.3808754349718));
#22596=CARTESIAN_POINT('Ctrl Pts',(-1.07311149596802,-0.482141027412377,
-26.391395717129));
#22597=CARTESIAN_POINT('Ctrl Pts',(-1.16777374859159,-0.169443851360826,
-26.413701919163));
#22598=CARTESIAN_POINT('Ctrl Pts',(-1.17306196823585,-0.0177920846727685,
-26.4238544504273));
#22599=CARTESIAN_POINT('Ctrl Pts',(-1.146284654438,0.262803931594613,-26.443066946934));
#22600=CARTESIAN_POINT('Ctrl Pts',(-1.10143556399854,0.414582166282623,
-26.4536437922865));
#22601=CARTESIAN_POINT('Ctrl Pts',(-0.946872694845556,0.704265996517489,
-26.4760689537007));
#22602=CARTESIAN_POINT('Ctrl Pts',(-0.843248468532123,0.814363861741638,
-26.4861776722252));
#22603=CARTESIAN_POINT('Ctrl Pts',(-0.632274348520029,0.991765068167528,
-26.5049627703415));
#22604=CARTESIAN_POINT('Ctrl Pts',(-0.493566643319589,1.06879852693625,
-26.5155699393044));
#22605=CARTESIAN_POINT('Ctrl Pts',(-0.206305151023333,1.15779145978756,
-26.5361124264564));
#22606=CARTESIAN_POINT('Ctrl Pts',(-0.0594720124149067,1.17343886176816,
-26.5460123069922));
#22607=CARTESIAN_POINT('Ctrl Pts',(0.212531118107504,1.15354400424969,-26.5645976950098));
#22608=CARTESIAN_POINT('Ctrl Pts',(0.368344830676736,1.12174076584227,-26.5752142761591));
#22609=CARTESIAN_POINT('Ctrl Pts',(0.657401586964147,0.974985736585916,
-26.5973572083036));
#22610=CARTESIAN_POINT('Ctrl Pts',(0.774838363480147,0.883314838061005,
-26.6073382677247));
#22611=CARTESIAN_POINT('Ctrl Pts',(0.955273189774578,0.680414508389961,
-26.6258424020917));
#22612=CARTESIAN_POINT('Ctrl Pts',(1.04462445846149,0.551227615412151,-26.6363291398119));
#22613=CARTESIAN_POINT('Ctrl Pts',(1.15094021376586,0.240868634693926,-26.6587333398718));
#22614=CARTESIAN_POINT('Ctrl Pts',(1.17156099735573,0.0915106406117304,
-26.6688267952484));
#22615=CARTESIAN_POINT('Ctrl Pts',(1.15872514586447,-0.185091355529294,
-26.687700147021));
#22616=CARTESIAN_POINT('Ctrl Pts',(1.13130517516905,-0.33759825108798,-26.698058357375));
#22617=CARTESIAN_POINT('Ctrl Pts',(0.991430863060781,-0.632184918383261,
-26.720322632698));
#22618=CARTESIAN_POINT('Ctrl Pts',(0.90082016681786,-0.754917089197193,
-26.7305283149135));
#22619=CARTESIAN_POINT('Ctrl Pts',(0.677727411882152,-0.96209289794022,
-26.7512852188951));
#22620=CARTESIAN_POINT('Ctrl Pts',(0.549326063249092,-1.04113475309212,
-26.7613874349405));
#22621=CARTESIAN_POINT('Ctrl Pts',(0.263511423283129,-1.14592402246405,
-26.7821622194306));
#22622=CARTESIAN_POINT('Ctrl Pts',(0.111156106659096,-1.17034442347985,
-26.7924781493724));
#22623=CARTESIAN_POINT('Ctrl Pts',(-0.194312135562315,-1.16089704614949,
-26.813322136256));
#22624=CARTESIAN_POINT('Ctrl Pts',(-0.343528450555845,-1.12590745534024,
-26.8235939550191));
#22625=CARTESIAN_POINT('Ctrl Pts',(-0.622881803069112,-0.997235485886511,
-26.8445727801415));
#22626=CARTESIAN_POINT('Ctrl Pts',(-0.749526335843675,-0.906069987879712,
-26.8550002344121));
#22627=CARTESIAN_POINT('Ctrl Pts',(-0.911877589687278,-0.732889579139973,
-26.8712003632541));
#22628=CARTESIAN_POINT('Ctrl Pts',(-0.962822718320643,-0.665102822245911,
-26.8769601814217));
#22629=CARTESIAN_POINT('Ctrl Pts',(-1.04860768641633,-0.51847552975876,
-26.8885666806712));
#22630=CARTESIAN_POINT('Ctrl Pts',(-1.08313436609589,-0.440796138886276,
-26.8943353600971));
#22631=CARTESIAN_POINT('Ctrl Pts',(-1.10908833794558,-0.360366944018197,
-26.9000986778144));
#22632=CARTESIAN_POINT('Ctrl Pts',(0.5101085474843,-1.049594504429,-23.22357429354));
#22633=CARTESIAN_POINT('Ctrl Pts',(0.2529114735039,-1.174593659124,-23.24307429354));
#22634=CARTESIAN_POINT('Ctrl Pts',(-0.3560404579669,-1.226109782198,-23.28207429354));
#22635=CARTESIAN_POINT('Ctrl Pts',(-1.086700069569,-0.6706284754496,-23.34057429354));
#22636=CARTESIAN_POINT('Ctrl Pts',(-1.255757769843,0.2313909492768,-23.39907429354));
#22637=CARTESIAN_POINT('Ctrl Pts',(-0.776277226745,1.013853625323,-23.45757429354));
#22638=CARTESIAN_POINT('Ctrl Pts',(0.1041850635563,1.27265480968,-23.51607429354));
#22639=CARTESIAN_POINT('Ctrl Pts',(0.930828216589,0.8741060067922,-23.57457429354));
#22640=CARTESIAN_POINT('Ctrl Pts',(1.276684843607,0.02406782860266,-23.63307429354));
#22641=CARTESIAN_POINT('Ctrl Pts',(0.9631123225395,-0.8384019827806,-23.69157429354));
#22642=CARTESIAN_POINT('Ctrl Pts',(0.1520765516308,-1.267823319973,-23.75007429354));
#22643=CARTESIAN_POINT('Ctrl Pts',(-0.737509290634,-1.042393065597,-23.80857429354));
#22644=CARTESIAN_POINT('Ctrl Pts',(-1.24615944086,-0.2785496368411,-23.86707429354));
#22645=CARTESIAN_POINT('Ctrl Pts',(-1.111147737084,0.6291692616945,-23.92557429354));
#22646=CARTESIAN_POINT('Ctrl Pts',(-0.4022099431193,1.211911884167,-23.98407429354));
#22647=CARTESIAN_POINT('Ctrl Pts',(0.5144759044836,1.16868207696,-24.04257429354));
#22648=CARTESIAN_POINT('Ctrl Pts',(1.165426482007,0.5218087469177,-24.10107429354));
#22649=CARTESIAN_POINT('Ctrl Pts',(1.214415105026,-0.3945873870257,-24.15957429354));
#22650=CARTESIAN_POINT('Ctrl Pts',(0.6361383436829,-1.107172642825,-24.21807429354));
#22651=CARTESIAN_POINT('Ctrl Pts',(-0.2707143395318,-1.247885010597,-24.27657429354));
#22652=CARTESIAN_POINT('Ctrl Pts',(-1.037738611881,-0.7440442370847,-24.33507429354));
#22653=CARTESIAN_POINT('Ctrl Pts',(-1.268753815782,0.1441076279268,-24.39357429354));
#22654=CARTESIAN_POINT('Ctrl Pts',(-0.8444367967899,0.957825531324,-24.45207429354));
#22655=CARTESIAN_POINT('Ctrl Pts',(0.01604572141757,1.27681078935,-24.51057429354));
#22656=CARTESIAN_POINT('Ctrl Pts',(0.868240364708,0.9363022574552,-24.56907429354));
#22657=CARTESIAN_POINT('Ctrl Pts',(1.271974557398,0.1121782326973,-24.62757429354));
#22658=CARTESIAN_POINT('Ctrl Pts',(1.018713020232,-0.7698878052547,-24.68607429354));
#22659=CARTESIAN_POINT('Ctrl Pts',(0.2392692263315,-1.254293712509,-24.74457429354));
#22660=CARTESIAN_POINT('Ctrl Pts',(-0.6637602414119,-1.090837812872,-24.80307429354));
#22661=CARTESIAN_POINT('Ctrl Pts',(-1.223949677731,-0.3639405071239,-24.86157429354));
#22662=CARTESIAN_POINT('Ctrl Pts',(-1.151937564121,0.5509166872562,-24.92007429354));
#22663=CARTESIAN_POINT('Ctrl Pts',(-0.4849732964329,1.181296108108,-24.97857429354));
#22664=CARTESIAN_POINT('Ctrl Pts',(0.4326464664874,1.20121898118,-25.03707429354));
#22665=CARTESIAN_POINT('Ctrl Pts',(0.8950185104062,0.8016085974549,-25.07607429354));
#22666=CARTESIAN_POINT('Ctrl Pts',(1.029622654482,0.5493055100063,-25.09557429354));
#22667=CARTESIAN_POINT('Ctrl Pts',(0.5101085474843,-1.049594504429,-23.28906643118));
#22668=CARTESIAN_POINT('Ctrl Pts',(0.2529114735039,-1.174593659124,-23.30856643118));
#22669=CARTESIAN_POINT('Ctrl Pts',(-0.3560404579669,-1.226109782198,-23.34756643118));
#22670=CARTESIAN_POINT('Ctrl Pts',(-1.086700069569,-0.6706284754496,-23.40606643118));
#22671=CARTESIAN_POINT('Ctrl Pts',(-1.255757769843,0.2313909492768,-23.46456643118));
#22672=CARTESIAN_POINT('Ctrl Pts',(-0.776277226745,1.013853625323,-23.52306643118));
#22673=CARTESIAN_POINT('Ctrl Pts',(0.1041850635563,1.27265480968,-23.58156643118));
#22674=CARTESIAN_POINT('Ctrl Pts',(0.930828216589,0.8741060067922,-23.64006643118));
#22675=CARTESIAN_POINT('Ctrl Pts',(1.276684843607,0.02406782860266,-23.69856643118));
#22676=CARTESIAN_POINT('Ctrl Pts',(0.9631123225395,-0.8384019827806,-23.75706643118));
#22677=CARTESIAN_POINT('Ctrl Pts',(0.1520765516308,-1.267823319973,-23.81556643118));
#22678=CARTESIAN_POINT('Ctrl Pts',(-0.737509290634,-1.042393065597,-23.87406643118));
#22679=CARTESIAN_POINT('Ctrl Pts',(-1.24615944086,-0.2785496368411,-23.93256643118));
#22680=CARTESIAN_POINT('Ctrl Pts',(-1.111147737084,0.6291692616945,-23.99106643118));
#22681=CARTESIAN_POINT('Ctrl Pts',(-0.4022099431193,1.211911884167,-24.04956643118));
#22682=CARTESIAN_POINT('Ctrl Pts',(0.5144759044836,1.16868207696,-24.10806643118));
#22683=CARTESIAN_POINT('Ctrl Pts',(1.165426482007,0.5218087469177,-24.16656643118));
#22684=CARTESIAN_POINT('Ctrl Pts',(1.214415105026,-0.3945873870257,-24.22506643118));
#22685=CARTESIAN_POINT('Ctrl Pts',(0.6361383436829,-1.107172642825,-24.28356643118));
#22686=CARTESIAN_POINT('Ctrl Pts',(-0.2707143395318,-1.247885010597,-24.34206643118));
#22687=CARTESIAN_POINT('Ctrl Pts',(-1.037738611881,-0.7440442370847,-24.40056643118));
#22688=CARTESIAN_POINT('Ctrl Pts',(-1.268753815782,0.1441076279268,-24.45906643118));
#22689=CARTESIAN_POINT('Ctrl Pts',(-0.8444367967899,0.957825531324,-24.51756643118));
#22690=CARTESIAN_POINT('Ctrl Pts',(0.01604572141757,1.27681078935,-24.57606643118));
#22691=CARTESIAN_POINT('Ctrl Pts',(0.868240364708,0.9363022574552,-24.63456643118));
#22692=CARTESIAN_POINT('Ctrl Pts',(1.271974557398,0.1121782326973,-24.69306643118));
#22693=CARTESIAN_POINT('Ctrl Pts',(1.018713020232,-0.7698878052547,-24.75156643118));
#22694=CARTESIAN_POINT('Ctrl Pts',(0.2392692263315,-1.254293712509,-24.81006643118));
#22695=CARTESIAN_POINT('Ctrl Pts',(-0.6637602414119,-1.090837812872,-24.86856643118));
#22696=CARTESIAN_POINT('Ctrl Pts',(-1.223949677731,-0.3639405071239,-24.92706643118));
#22697=CARTESIAN_POINT('Ctrl Pts',(-1.151937564121,0.5509166872562,-24.98556643118));
#22698=CARTESIAN_POINT('Ctrl Pts',(-0.4849732964329,1.181296108108,-25.04406643118));
#22699=CARTESIAN_POINT('Ctrl Pts',(0.4326464664874,1.20121898118,-25.10256643118));
#22700=CARTESIAN_POINT('Ctrl Pts',(0.8950185104062,0.8016085974549,-25.14156643118));
#22701=CARTESIAN_POINT('Ctrl Pts',(1.029622654482,0.5493055100063,-25.16106643118));
#22702=CARTESIAN_POINT('Ctrl Pts',(0.5101085474843,-1.049594504429,-23.35455856882));
#22703=CARTESIAN_POINT('Ctrl Pts',(0.2529114735039,-1.174593659124,-23.37405856882));
#22704=CARTESIAN_POINT('Ctrl Pts',(-0.3560404579669,-1.226109782198,-23.41305856882));
#22705=CARTESIAN_POINT('Ctrl Pts',(-1.086700069569,-0.6706284754496,-23.47155856882));
#22706=CARTESIAN_POINT('Ctrl Pts',(-1.255757769843,0.2313909492768,-23.53005856882));
#22707=CARTESIAN_POINT('Ctrl Pts',(-0.776277226745,1.013853625323,-23.58855856882));
#22708=CARTESIAN_POINT('Ctrl Pts',(0.1041850635563,1.27265480968,-23.64705856882));
#22709=CARTESIAN_POINT('Ctrl Pts',(0.930828216589,0.8741060067922,-23.70555856882));
#22710=CARTESIAN_POINT('Ctrl Pts',(1.276684843607,0.02406782860266,-23.76405856882));
#22711=CARTESIAN_POINT('Ctrl Pts',(0.9631123225395,-0.8384019827806,-23.82255856882));
#22712=CARTESIAN_POINT('Ctrl Pts',(0.1520765516308,-1.267823319973,-23.88105856882));
#22713=CARTESIAN_POINT('Ctrl Pts',(-0.737509290634,-1.042393065597,-23.93955856882));
#22714=CARTESIAN_POINT('Ctrl Pts',(-1.24615944086,-0.2785496368411,-23.99805856882));
#22715=CARTESIAN_POINT('Ctrl Pts',(-1.111147737084,0.6291692616945,-24.05655856882));
#22716=CARTESIAN_POINT('Ctrl Pts',(-0.4022099431193,1.211911884167,-24.11505856882));
#22717=CARTESIAN_POINT('Ctrl Pts',(0.5144759044836,1.16868207696,-24.17355856882));
#22718=CARTESIAN_POINT('Ctrl Pts',(1.165426482007,0.5218087469177,-24.23205856882));
#22719=CARTESIAN_POINT('Ctrl Pts',(1.214415105026,-0.3945873870257,-24.29055856882));
#22720=CARTESIAN_POINT('Ctrl Pts',(0.6361383436829,-1.107172642825,-24.34905856882));
#22721=CARTESIAN_POINT('Ctrl Pts',(-0.2707143395318,-1.247885010597,-24.40755856882));
#22722=CARTESIAN_POINT('Ctrl Pts',(-1.037738611881,-0.7440442370847,-24.46605856882));
#22723=CARTESIAN_POINT('Ctrl Pts',(-1.268753815782,0.1441076279268,-24.52455856882));
#22724=CARTESIAN_POINT('Ctrl Pts',(-0.8444367967899,0.957825531324,-24.58305856882));
#22725=CARTESIAN_POINT('Ctrl Pts',(0.01604572141757,1.27681078935,-24.64155856882));
#22726=CARTESIAN_POINT('Ctrl Pts',(0.868240364708,0.9363022574552,-24.70005856882));
#22727=CARTESIAN_POINT('Ctrl Pts',(1.271974557398,0.1121782326973,-24.75855856882));
#22728=CARTESIAN_POINT('Ctrl Pts',(1.018713020232,-0.7698878052547,-24.81705856882));
#22729=CARTESIAN_POINT('Ctrl Pts',(0.2392692263315,-1.254293712509,-24.87555856882));
#22730=CARTESIAN_POINT('Ctrl Pts',(-0.6637602414119,-1.090837812872,-24.93405856882));
#22731=CARTESIAN_POINT('Ctrl Pts',(-1.223949677731,-0.3639405071239,-24.99255856882));
#22732=CARTESIAN_POINT('Ctrl Pts',(-1.151937564121,0.5509166872562,-25.05105856882));
#22733=CARTESIAN_POINT('Ctrl Pts',(-0.4849732964329,1.181296108108,-25.10955856882));
#22734=CARTESIAN_POINT('Ctrl Pts',(0.4326464664874,1.20121898118,-25.16805856882));
#22735=CARTESIAN_POINT('Ctrl Pts',(0.8950185104062,0.8016085974549,-25.20705856882));
#22736=CARTESIAN_POINT('Ctrl Pts',(1.029622654482,0.5493055100063,-25.22655856882));
#22737=CARTESIAN_POINT('Ctrl Pts',(0.5101085474843,-1.049594504429,-23.42005070646));
#22738=CARTESIAN_POINT('Ctrl Pts',(0.2529114735039,-1.174593659124,-23.43955070646));
#22739=CARTESIAN_POINT('Ctrl Pts',(-0.3560404579669,-1.226109782198,-23.47855070646));
#22740=CARTESIAN_POINT('Ctrl Pts',(-1.086700069569,-0.6706284754496,-23.53705070646));
#22741=CARTESIAN_POINT('Ctrl Pts',(-1.255757769843,0.2313909492768,-23.59555070646));
#22742=CARTESIAN_POINT('Ctrl Pts',(-0.776277226745,1.013853625323,-23.65405070646));
#22743=CARTESIAN_POINT('Ctrl Pts',(0.1041850635563,1.27265480968,-23.71255070646));
#22744=CARTESIAN_POINT('Ctrl Pts',(0.930828216589,0.8741060067922,-23.77105070646));
#22745=CARTESIAN_POINT('Ctrl Pts',(1.276684843607,0.02406782860266,-23.82955070646));
#22746=CARTESIAN_POINT('Ctrl Pts',(0.9631123225395,-0.8384019827806,-23.88805070646));
#22747=CARTESIAN_POINT('Ctrl Pts',(0.1520765516308,-1.267823319973,-23.94655070646));
#22748=CARTESIAN_POINT('Ctrl Pts',(-0.737509290634,-1.042393065597,-24.00505070646));
#22749=CARTESIAN_POINT('Ctrl Pts',(-1.24615944086,-0.2785496368411,-24.06355070646));
#22750=CARTESIAN_POINT('Ctrl Pts',(-1.111147737084,0.6291692616945,-24.12205070646));
#22751=CARTESIAN_POINT('Ctrl Pts',(-0.4022099431193,1.211911884167,-24.18055070646));
#22752=CARTESIAN_POINT('Ctrl Pts',(0.5144759044836,1.16868207696,-24.23905070646));
#22753=CARTESIAN_POINT('Ctrl Pts',(1.165426482007,0.5218087469177,-24.29755070646));
#22754=CARTESIAN_POINT('Ctrl Pts',(1.214415105026,-0.3945873870257,-24.35605070646));
#22755=CARTESIAN_POINT('Ctrl Pts',(0.6361383436829,-1.107172642825,-24.41455070646));
#22756=CARTESIAN_POINT('Ctrl Pts',(-0.2707143395318,-1.247885010597,-24.47305070646));
#22757=CARTESIAN_POINT('Ctrl Pts',(-1.037738611881,-0.7440442370847,-24.53155070646));
#22758=CARTESIAN_POINT('Ctrl Pts',(-1.268753815782,0.1441076279268,-24.59005070646));
#22759=CARTESIAN_POINT('Ctrl Pts',(-0.8444367967899,0.957825531324,-24.64855070646));
#22760=CARTESIAN_POINT('Ctrl Pts',(0.01604572141757,1.27681078935,-24.70705070646));
#22761=CARTESIAN_POINT('Ctrl Pts',(0.868240364708,0.9363022574552,-24.76555070646));
#22762=CARTESIAN_POINT('Ctrl Pts',(1.271974557398,0.1121782326973,-24.82405070646));
#22763=CARTESIAN_POINT('Ctrl Pts',(1.018713020232,-0.7698878052547,-24.88255070646));
#22764=CARTESIAN_POINT('Ctrl Pts',(0.2392692263315,-1.254293712509,-24.94105070646));
#22765=CARTESIAN_POINT('Ctrl Pts',(-0.6637602414119,-1.090837812872,-24.99955070646));
#22766=CARTESIAN_POINT('Ctrl Pts',(-1.223949677731,-0.3639405071239,-25.05805070646));
#22767=CARTESIAN_POINT('Ctrl Pts',(-1.151937564121,0.5509166872562,-25.11655070646));
#22768=CARTESIAN_POINT('Ctrl Pts',(-0.4849732964329,1.181296108108,-25.17505070646));
#22769=CARTESIAN_POINT('Ctrl Pts',(0.4326464664874,1.20121898118,-25.23355070646));
#22770=CARTESIAN_POINT('Ctrl Pts',(0.8950185104062,0.8016085974549,-25.27255070646));
#22771=CARTESIAN_POINT('Ctrl Pts',(1.029622654482,0.5493055100063,-25.29205070646));
#22772=CARTESIAN_POINT('',(7.7598198018898E-11,-1.1661651967976,-23.3000561186915));
#22773=CARTESIAN_POINT('',(-8.83583665353582E-11,-1.16616519683289,-23.4155261737951));
#22774=CARTESIAN_POINT('Ctrl Pts',(5.00307097096597E-18,-1.16616519645645,
-23.3000561186915));
#22775=CARTESIAN_POINT('Ctrl Pts',(2.42851199960663E-16,-1.16616519645645,
-23.3193082457943));
#22776=CARTESIAN_POINT('Ctrl Pts',(8.88178419700125E-15,-1.16616519645645,
-23.3385603728972));
#22777=CARTESIAN_POINT('Ctrl Pts',(8.88178419700125E-15,-1.16616519645645,
-23.377050391265));
#22778=CARTESIAN_POINT('Ctrl Pts',(2.5533440660903E-16,-1.16616519645645,
-23.3962882825301));
#22779=CARTESIAN_POINT('Ctrl Pts',(5.53195026095858E-18,-1.16616519645645,
-23.4155261737951));
#22780=CARTESIAN_POINT('Ctrl Pts',(-1.33558877062777E-10,-1.16616519645672,
-23.4155261731434));
#22781=CARTESIAN_POINT('Ctrl Pts',(-0.0845144697814676,-1.1663356487857,
-23.4212895959207));
#22782=CARTESIAN_POINT('Ctrl Pts',(-0.169062851789874,-1.15750290857422,
-23.4270583806262));
#22783=CARTESIAN_POINT('Ctrl Pts',(-0.335023329548445,-1.12122637131796,
-23.4386649290137));
#22784=CARTESIAN_POINT('Ctrl Pts',(-0.415234485903957,-1.09372210750977,
-23.4444246931359));
#22785=CARTESIAN_POINT('Ctrl Pts',(-0.630107390685444,-0.992832930186848,
-23.4606247655878));
#22786=CARTESIAN_POINT('Ctrl Pts',(-0.75594624449798,-0.900558510223427,
-23.4710522198585));
#22787=CARTESIAN_POINT('Ctrl Pts',(-0.964645492873469,-0.67463950922821,
-23.492031044981));
#22788=CARTESIAN_POINT('Ctrl Pts',(-1.04403294838599,-0.543538738702725,
-23.502302863744));
#22789=CARTESIAN_POINT('Ctrl Pts',(-1.14741281624633,-0.255940576564088,
-23.5231468506275));
#22790=CARTESIAN_POINT('Ctrl Pts',(-1.1712680167499,-0.103495740972837,
-23.5334627805691));
#22791=CARTESIAN_POINT('Ctrl Pts',(-1.1599290802664,0.200711799883823,-23.5542375650592));
#22792=CARTESIAN_POINT('Ctrl Pts',(-1.12443400769239,0.347254015711778,
-23.5643397811048));
#22793=CARTESIAN_POINT('Ctrl Pts',(-0.996337557365363,0.623448679756951,
-23.5850966850865));
#22794=CARTESIAN_POINT('Ctrl Pts',(-0.907612571565183,0.747550899402566,
-23.5953023673021));
#22795=CARTESIAN_POINT('Ctrl Pts',(-0.670667541538861,0.971611561905498,
-23.617566642625));
#22796=CARTESIAN_POINT('Ctrl Pts',(-0.534098101668266,1.04481672619882,
-23.6279248529788));
#22797=CARTESIAN_POINT('Ctrl Pts',(-0.275000467066175,1.14249906388745,
-23.6467982047513));
#22798=CARTESIAN_POINT('Ctrl Pts',(-0.126580400966591,1.16904169170034,
-23.6568916601278));
#22799=CARTESIAN_POINT('Ctrl Pts',(0.20144190519578,1.163835599232,-23.6792958601877));
#22800=CARTESIAN_POINT('Ctrl Pts',(0.35191700207576,1.11877843828859,-23.6897825979081));
#22801=CARTESIAN_POINT('Ctrl Pts',(0.600644110469965,1.00987437100721,-23.7082867322753));
#22802=CARTESIAN_POINT('Ctrl Pts',(0.724118275574684,0.926513224982849,
-23.7182677916966));
#22803=CARTESIAN_POINT('Ctrl Pts',(0.953014052479287,0.696953711387198,
-23.7404107238412));
#22804=CARTESIAN_POINT('Ctrl Pts',(1.03140981474657,0.558593805864354,-23.7510273049906));
#22805=CARTESIAN_POINT('Ctrl Pts',(1.13438453848494,0.306051305202018,-23.7696126930082));
#22806=CARTESIAN_POINT('Ctrl Pts',(1.16487691003558,0.161569378790797,-23.779512573544));
#22807=CARTESIAN_POINT('Ctrl Pts',(1.1690082842922,-0.139132863968416,-23.8000550606958));
#22808=CARTESIAN_POINT('Ctrl Pts',(1.13860814951507,-0.294856378754733,
-23.8106622296586));
#22809=CARTESIAN_POINT('Ctrl Pts',(1.03508416460198,-0.550324677970256,
-23.8294473277748));
#22810=CARTESIAN_POINT('Ctrl Pts',(0.962396519410018,-0.68289928505056,
-23.8395560462992));
#22811=CARTESIAN_POINT('Ctrl Pts',(0.734653378267124,-0.919414535474106,
-23.8619812077135));
#22812=CARTESIAN_POINT('Ctrl Pts',(0.604162830263392,-1.00897060908126,
-23.8725580530661));
#22813=CARTESIAN_POINT('Ctrl Pts',(0.345574805573191,-1.12114628543803,
-23.8917705495728));
#22814=CARTESIAN_POINT('Ctrl Pts',(0.199711254916898,-1.16297986281931,
-23.9019230808372));
#22815=CARTESIAN_POINT('Ctrl Pts',(-0.126933676780373,-1.16957945210744,
-23.9242292828711));
#22816=CARTESIAN_POINT('Ctrl Pts',(-0.281876844625177,-1.1416255416875,
-23.9347495650282));
#22817=CARTESIAN_POINT('Ctrl Pts',(-0.570992366278221,-1.02925644591801,
-23.9558983763229));
#22818=CARTESIAN_POINT('Ctrl Pts',(-0.697263581724959,-0.948022205646459,
-23.9659604824616));
#22819=CARTESIAN_POINT('Ctrl Pts',(-0.916131644797461,-0.737369452220616,
-23.9866904752755));
#22820=CARTESIAN_POINT('Ctrl Pts',(-1.00561323080168,-0.609375357425688,
-23.99712681397));
#22821=CARTESIAN_POINT('Ctrl Pts',(-1.13039245242821,-0.328317197026739,
-24.0181021416964));
#22822=CARTESIAN_POINT('Ctrl Pts',(-1.1634069179183,-0.178818109672421,
-24.0283633413595));
#22823=CARTESIAN_POINT('Ctrl Pts',(-1.16875032198559,0.12696882202449,-24.0492232952251));
#22824=CARTESIAN_POINT('Ctrl Pts',(-1.14219860207787,0.279159893052852,
-24.0595514605357));
#22825=CARTESIAN_POINT('Ctrl Pts',(-1.03394101835653,0.562304922521268,
-24.0802380394371));
#22826=CARTESIAN_POINT('Ctrl Pts',(-0.95368391938154,0.689879242768186,
-24.0903371103175));
#22827=CARTESIAN_POINT('Ctrl Pts',(-0.742383306622126,0.911216853453345,
-24.1112005351712));
#22828=CARTESIAN_POINT('Ctrl Pts',(-0.618206000916698,1.00020464731638,
-24.1214196096764));
#22829=CARTESIAN_POINT('Ctrl Pts',(-0.321789924774097,1.13584465913637,
-24.1436737563466));
#22830=CARTESIAN_POINT('Ctrl Pts',(-0.169162204071789,1.16122379076491,
-24.1540179844192));
#22831=CARTESIAN_POINT('Ctrl Pts',(0.108153891961831,1.17016174517532,-24.1729300210824));
#22832=CARTESIAN_POINT('Ctrl Pts',(0.257408061948685,1.14734985937776,-24.1830368577589));
#22833=CARTESIAN_POINT('Ctrl Pts',(0.565904932159938,1.03666604024609,-24.2054191523544));
#22834=CARTESIAN_POINT('Ctrl Pts',(0.693688938373763,0.945769370032585,
-24.2158902244772));
#22835=CARTESIAN_POINT('Ctrl Pts',(0.894475531414044,0.76194677441218,-24.2344423045361));
#22836=CARTESIAN_POINT('Ctrl Pts',(0.984535131627163,0.643003781679394,
-24.2444366233424));
#22837=CARTESIAN_POINT('Ctrl Pts',(1.13391927855465,0.337728284171994,-24.2676508056257));
#22838=CARTESIAN_POINT('Ctrl Pts',(1.1576563306076,0.176511653662717,-24.2784973022939));
#22839=CARTESIAN_POINT('Ctrl Pts',(1.17242604546444,-0.0765243655160787,
-24.2957700105566));
#22840=CARTESIAN_POINT('Ctrl Pts',(1.15463119368819,-0.222860809232089,
-24.3056531858431));
#22841=CARTESIAN_POINT('Ctrl Pts',(1.0651105549098,-0.498377005437864,-24.3254418679969));
#22842=CARTESIAN_POINT('Ctrl Pts',(0.993492488919996,-0.627225226741351,
-24.3353250432864));
#22843=CARTESIAN_POINT('Ctrl Pts',(0.83281269822665,-0.823254245872666,
-24.3525977515491));
#22844=CARTESIAN_POINT('Ctrl Pts',(0.718848261881902,-0.939728950600801,
-24.3634442482174));
#22845=CARTESIAN_POINT('Ctrl Pts',(0.418557513006822,-1.09889621756008,
-24.3866584305006));
#22846=CARTESIAN_POINT('Ctrl Pts',(0.275784828936188,-1.14218741521005,
-24.3966527493069));
#22847=CARTESIAN_POINT('Ctrl Pts',(0.00529685218042203,-1.17288362077003,
-24.4152048293658));
#22848=CARTESIAN_POINT('Ctrl Pts',(-0.15151030268991,-1.17131101737357,
-24.4256759014886));
#22849=CARTESIAN_POINT('Ctrl Pts',(-0.466147829955441,-1.07952619736496,
-24.4480581960842));
#22850=CARTESIAN_POINT('Ctrl Pts',(-0.60030548000498,-1.01025200068753,
-24.4581650327607));
#22851=CARTESIAN_POINT('Ctrl Pts',(-0.819405316722027,-0.840018732202679,
-24.477077069424));
#22852=CARTESIAN_POINT('Ctrl Pts',(-0.927966257295848,-0.7297742600928,
-24.4874212974965));
#22853=CARTESIAN_POINT('Ctrl Pts',(-1.08804470173287,-0.445810187314043,
-24.5096754441668));
#22854=CARTESIAN_POINT('Ctrl Pts',(-1.13620053949762,-0.300827960823797,
-24.519894518672));
#22855=CARTESIAN_POINT('Ctrl Pts',(-1.1770473428035,0.00243731169511532,
-24.5407579435258));
#22856=CARTESIAN_POINT('Ctrl Pts',(-1.16699039578116,0.152821043989816,
-24.5508570144063));
#22857=CARTESIAN_POINT('Ctrl Pts',(-1.08814414820036,0.445522395862589,
-24.5715435933077));
#22858=CARTESIAN_POINT('Ctrl Pts',(-1.02016927375459,0.584254268101373,
-24.5818717586182));
#22859=CARTESIAN_POINT('Ctrl Pts',(-0.836109320261249,0.82850031839418,
-24.6027317124839));
#22860=CARTESIAN_POINT('Ctrl Pts',(-0.721526697841524,0.93004220478004,
-24.612992912147));
#22861=CARTESIAN_POINT('Ctrl Pts',(-0.455376345281851,1.08407964668604,
-24.6339682398733));
#22862=CARTESIAN_POINT('Ctrl Pts',(-0.307751180219848,1.1350330879498,-24.6444045785678));
#22863=CARTESIAN_POINT('Ctrl Pts',(-0.00686461584986442,1.17680732571145,
-24.6651345713816));
#22864=CARTESIAN_POINT('Ctrl Pts',(0.143039231759796,1.16830684838774,-24.6751966775203));
#22865=CARTESIAN_POINT('Ctrl Pts',(0.44298749942166,1.08927751667136,-24.6963454888151));
#22866=CARTESIAN_POINT('Ctrl Pts',(0.584770051659173,1.0208193962577,-24.7068657709722));
#22867=CARTESIAN_POINT('Ctrl Pts',(0.84515221127406,0.823483142780032,-24.7291719730062));
#22868=CARTESIAN_POINT('Ctrl Pts',(0.938569142779572,0.703902623820296,
-24.7393245042705));
#22869=CARTESIAN_POINT('Ctrl Pts',(1.08183604106747,0.461156367959811,-24.7585370007774));
#22870=CARTESIAN_POINT('Ctrl Pts',(1.13476537268836,0.312003562781931,-24.76911384613));
#22871=CARTESIAN_POINT('Ctrl Pts',(1.17999326808417,-0.0132053539141161,
-24.7915390075444));
#22872=CARTESIAN_POINT('Ctrl Pts',(1.16087340945535,-0.163185189932334,
-24.8016477260688));
#22873=CARTESIAN_POINT('Ctrl Pts',(1.09446557386838,-0.430713257112194,
-24.820432824185));
#22874=CARTESIAN_POINT('Ctrl Pts',(1.02752781410787,-0.574564977887768,
-24.8310399931477));
#22875=CARTESIAN_POINT('Ctrl Pts',(0.847437118499067,-0.81540984166698,
-24.8515824802994));
#22876=CARTESIAN_POINT('Ctrl Pts',(0.737843926148438,-0.914375209208886,
-24.8614823608351));
#22877=CARTESIAN_POINT('Ctrl Pts',(0.506094867186335,-1.05815936007466,
-24.8800677488527));
#22878=CARTESIAN_POINT('Ctrl Pts',(0.3613454512501,-1.12401500207983,-24.890684330002));
#22879=CARTESIAN_POINT('Ctrl Pts',(0.0412331811787559,-1.17519098782271,
-24.9128272621465));
#22880=CARTESIAN_POINT('Ctrl Pts',(-0.107657969004568,-1.17005527833936,
-24.9228083215679));
#22881=CARTESIAN_POINT('Ctrl Pts',(-0.372894631319867,-1.11196239336716,
-24.9413124559351));
#22882=CARTESIAN_POINT('Ctrl Pts',(-0.521115476638633,-1.0599673595054,
-24.9517991936555));
#22883=CARTESIAN_POINT('Ctrl Pts',(-0.789551161232938,-0.871372502801514,
-24.9742033937154));
#22884=CARTESIAN_POINT('Ctrl Pts',(-0.894024151828224,-0.762659939827971,
-24.9842968490918));
#22885=CARTESIAN_POINT('Ctrl Pts',(-1.04622230392104,-0.531339500064551,
-25.0031702008643));
#22886=CARTESIAN_POINT('Ctrl Pts',(-1.11368038572552,-0.391841775405243,
-25.0135284112181));
#22887=CARTESIAN_POINT('Ctrl Pts',(-1.17367338871164,-0.0713000974154914,
-25.0357926865411));
#22888=CARTESIAN_POINT('Ctrl Pts',(-1.17250795556528,0.0812519454809356,
-25.0459983687568));
#22889=CARTESIAN_POINT('Ctrl Pts',(-1.11379701051142,0.379991326821873,
-25.0667552727385));
#22890=CARTESIAN_POINT('Ctrl Pts',(-1.05637777413877,0.519409950007744,
-25.0768574887841));
#22891=CARTESIAN_POINT('Ctrl Pts',(-0.886742460300511,0.772183880019224,
-25.0976322732742));
#22892=CARTESIAN_POINT('Ctrl Pts',(-0.777838371540452,0.881492607670503,
-25.1079482032157));
#22893=CARTESIAN_POINT('Ctrl Pts',(-0.525156343273892,1.05339924667952,
-25.1287921900992));
#22894=CARTESIAN_POINT('Ctrl Pts',(-0.383871443144744,1.11279922244327,
-25.1390640088622));
#22895=CARTESIAN_POINT('Ctrl Pts',(-0.0822383474976608,1.17290119324133,
-25.1600428339846));
#22896=CARTESIAN_POINT('Ctrl Pts',(0.0738049670078697,1.17358654470157,
-25.1704702882553));
#22897=CARTESIAN_POINT('Ctrl Pts',(0.30694278066829,1.12890832363893,-25.1866704170972));
#22898=CARTESIAN_POINT('Ctrl Pts',(0.388002311516126,1.10401248060505,-25.1924302352649));
#22899=CARTESIAN_POINT('Ctrl Pts',(0.543589114829183,1.03581167186204,-25.2040367304977));
#22900=CARTESIAN_POINT('Ctrl Pts',(0.617180537264655,0.993262033258738,
-25.2098054059139));
#22901=CARTESIAN_POINT('Ctrl Pts',(0.685452796065063,0.943448854418561,
-25.2155687196295));
#22902=CARTESIAN_POINT('Ctrl Pts',(1.1723987758447E-10,-1.16616519645621,
-23.3000561192829));
#22903=CARTESIAN_POINT('Ctrl Pts',(-0.0845143073622228,-1.16633564847594,
-23.3058195310012));
#22904=CARTESIAN_POINT('Ctrl Pts',(-0.169062527012607,-1.15750294251081,
-23.3115883046236));
#22905=CARTESIAN_POINT('Ctrl Pts',(-0.33502302258755,-1.12122647584571,
-23.3231948531434));
#22906=CARTESIAN_POINT('Ctrl Pts',(-0.415234336721324,-1.09372217755542,
-23.3289546280455));
#22907=CARTESIAN_POINT('Ctrl Pts',(-0.630107390685439,-0.992832930186849,
-23.3451547117448));
#22908=CARTESIAN_POINT('Ctrl Pts',(-0.755946244497973,-0.900558510223433,
-23.3555821660154));
#22909=CARTESIAN_POINT('Ctrl Pts',(-0.964645492873463,-0.674639509228219,
-23.3765609911377));
#22910=CARTESIAN_POINT('Ctrl Pts',(-1.04403294838599,-0.543538738702735,
-23.3868328099007));
#22911=CARTESIAN_POINT('Ctrl Pts',(-1.14741281624633,-0.2559405765641,-23.4076767967842));
#22912=CARTESIAN_POINT('Ctrl Pts',(-1.1712680167499,-0.103495740972848,
-23.4179927267258));
#22913=CARTESIAN_POINT('Ctrl Pts',(-1.1599290802664,0.200711799883798,-23.4387675112159));
#22914=CARTESIAN_POINT('Ctrl Pts',(-1.1244340076924,0.347254015711756,-23.4488697272615));
#22915=CARTESIAN_POINT('Ctrl Pts',(-0.996337557365367,0.623448679756947,
-23.4696266312432));
#22916=CARTESIAN_POINT('Ctrl Pts',(-0.907612571565185,0.747550899402563,
-23.4798323134588));
#22917=CARTESIAN_POINT('Ctrl Pts',(-0.670667541538861,0.971611561905498,
-23.5020965887818));
#22918=CARTESIAN_POINT('Ctrl Pts',(-0.534098101668265,1.04481672619882,
-23.5124547991357));
#22919=CARTESIAN_POINT('Ctrl Pts',(-0.275000467066174,1.14249906388745,
-23.5313281509082));
#22920=CARTESIAN_POINT('Ctrl Pts',(-0.12658040096659,1.16904169170034,-23.5414216062847));
#22921=CARTESIAN_POINT('Ctrl Pts',(0.201441905195779,1.163835599232,-23.5638258063446));
#22922=CARTESIAN_POINT('Ctrl Pts',(0.351917002075758,1.11877843828859,-23.5743125440649));
#22923=CARTESIAN_POINT('Ctrl Pts',(0.600644110469963,1.00987437100721,-23.5928166784321));
#22924=CARTESIAN_POINT('Ctrl Pts',(0.72411827557468,0.926513224982852,-23.6027977378534));
#22925=CARTESIAN_POINT('Ctrl Pts',(0.953014052479293,0.696953711387194,
-23.6249406699979));
#22926=CARTESIAN_POINT('Ctrl Pts',(1.03140981474657,0.558593805864345,-23.6355572511473));
#22927=CARTESIAN_POINT('Ctrl Pts',(1.13438453848494,0.306051305202025,-23.6541426391649));
#22928=CARTESIAN_POINT('Ctrl Pts',(1.16487691003558,0.161569378790804,-23.6640425197007));
#22929=CARTESIAN_POINT('Ctrl Pts',(1.1690082842922,-0.139132863968409,-23.6845850068526));
#22930=CARTESIAN_POINT('Ctrl Pts',(1.13860814951507,-0.294856378754726,
-23.6951921758154));
#22931=CARTESIAN_POINT('Ctrl Pts',(1.03508416460199,-0.550324677970245,
-23.7139772739316));
#22932=CARTESIAN_POINT('Ctrl Pts',(0.962396519410025,-0.682899285050549,
-23.724085992456));
#22933=CARTESIAN_POINT('Ctrl Pts',(0.734653378267133,-0.919414535474099,
-23.7465111538702));
#22934=CARTESIAN_POINT('Ctrl Pts',(0.604162830263402,-1.00897060908125,
-23.7570879992228));
#22935=CARTESIAN_POINT('Ctrl Pts',(0.3455748055732,-1.12114628543803,-23.7763004957295));
#22936=CARTESIAN_POINT('Ctrl Pts',(0.199711254916905,-1.16297986281931,
-23.7864530269939));
#22937=CARTESIAN_POINT('Ctrl Pts',(-0.126933676780369,-1.16957945210744,
-23.8087592290278));
#22938=CARTESIAN_POINT('Ctrl Pts',(-0.281876844625174,-1.14162554168751,
-23.819279511185));
#22939=CARTESIAN_POINT('Ctrl Pts',(-0.570992366278222,-1.02925644591801,
-23.8404283224798));
#22940=CARTESIAN_POINT('Ctrl Pts',(-0.697263581724958,-0.948022205646458,
-23.8504904286185));
#22941=CARTESIAN_POINT('Ctrl Pts',(-0.916131644797455,-0.737369452220623,
-23.8712204214323));
#22942=CARTESIAN_POINT('Ctrl Pts',(-1.00561323080168,-0.609375357425699,
-23.8816567601267));
#22943=CARTESIAN_POINT('Ctrl Pts',(-1.13039245242821,-0.328317197026754,
-23.902632087853));
#22944=CARTESIAN_POINT('Ctrl Pts',(-1.1634069179183,-0.17881810967244,-23.9128932875161));
#22945=CARTESIAN_POINT('Ctrl Pts',(-1.16875032198559,0.126968822024469,
-23.9337532413817));
#22946=CARTESIAN_POINT('Ctrl Pts',(-1.14219860207787,0.279159893052831,
-23.9440814066923));
#22947=CARTESIAN_POINT('Ctrl Pts',(-1.03394101835655,0.562304922521242,
-23.9647679855936));
#22948=CARTESIAN_POINT('Ctrl Pts',(-0.953683919381558,0.689879242768163,
-23.9748670564741));
#22949=CARTESIAN_POINT('Ctrl Pts',(-0.742383306622142,0.911216853453332,
-23.9957304813278));
#22950=CARTESIAN_POINT('Ctrl Pts',(-0.618206000916717,1.00020464731637,
-24.005949555833));
#22951=CARTESIAN_POINT('Ctrl Pts',(-0.321789924774117,1.13584465913636,
-24.0282037025032));
#22952=CARTESIAN_POINT('Ctrl Pts',(-0.169162204071811,1.16122379076491,
-24.0385479305758));
#22953=CARTESIAN_POINT('Ctrl Pts',(0.108153891961813,1.17016174517532,-24.057459967239));
#22954=CARTESIAN_POINT('Ctrl Pts',(0.25740806194867,1.14734985937777,-24.0675668039155));
#22955=CARTESIAN_POINT('Ctrl Pts',(0.565904932159931,1.03666604024609,-24.089949098511));
#22956=CARTESIAN_POINT('Ctrl Pts',(0.69368893837376,0.945769370032588,-24.1004201706339));
#22957=CARTESIAN_POINT('Ctrl Pts',(0.894475531414044,0.76194677441218,-24.118972250693));
#22958=CARTESIAN_POINT('Ctrl Pts',(0.984535131627164,0.643003781679392,
-24.1289665694994));
#22959=CARTESIAN_POINT('Ctrl Pts',(1.13391927855465,0.337728284171982,-24.1521807517827));
#22960=CARTESIAN_POINT('Ctrl Pts',(1.15765633060761,0.176511653662702,-24.163027248451));
#22961=CARTESIAN_POINT('Ctrl Pts',(1.17242604546444,-0.0765243655160832,
-24.1802999567137));
#22962=CARTESIAN_POINT('Ctrl Pts',(1.15463119368819,-0.222860809232091,
-24.1901831320031));
#22963=CARTESIAN_POINT('Ctrl Pts',(1.0651105549098,-0.498377005437862,-24.2099718141569));
#22964=CARTESIAN_POINT('Ctrl Pts',(0.993492488919999,-0.627225226741345,
-24.2198549894433));
#22965=CARTESIAN_POINT('Ctrl Pts',(0.832812698226625,-0.823254245872699,
-24.237127697706));
#22966=CARTESIAN_POINT('Ctrl Pts',(0.71884826188187,-0.939728950600817,
-24.2479741943742));
#22967=CARTESIAN_POINT('Ctrl Pts',(0.418557513006823,-1.09889621756008,
-24.2711883766575));
#22968=CARTESIAN_POINT('Ctrl Pts',(0.275784828936185,-1.14218741521005,
-24.2811826954639));
#22969=CARTESIAN_POINT('Ctrl Pts',(0.00529685218041781,-1.17288362077003,
-24.2997347755229));
#22970=CARTESIAN_POINT('Ctrl Pts',(-0.151510302689914,-1.17131101737357,
-24.3102058476458));
#22971=CARTESIAN_POINT('Ctrl Pts',(-0.466147829955446,-1.07952619736495,
-24.3325881422413));
#22972=CARTESIAN_POINT('Ctrl Pts',(-0.600305480004984,-1.01025200068752,
-24.3426949789178));
#22973=CARTESIAN_POINT('Ctrl Pts',(-0.819405316722026,-0.840018732202679,
-24.361607015581));
#22974=CARTESIAN_POINT('Ctrl Pts',(-0.927966257295847,-0.729774260092801,
-24.3719512436536));
#22975=CARTESIAN_POINT('Ctrl Pts',(-1.08804470173286,-0.445810187314049,
-24.3942053903238));
#22976=CARTESIAN_POINT('Ctrl Pts',(-1.13620053949761,-0.300827960823807,
-24.4044244648289));
#22977=CARTESIAN_POINT('Ctrl Pts',(-1.1770473428035,0.00243731169510533,
-24.4252878896826));
#22978=CARTESIAN_POINT('Ctrl Pts',(-1.16699039578116,0.152821043989804,
-24.435386960563));
#22979=CARTESIAN_POINT('Ctrl Pts',(-1.08814414820037,0.445522395862568,
-24.4560735394643));
#22980=CARTESIAN_POINT('Ctrl Pts',(-1.0201692737546,0.58425426810135,-24.4664017047749));
#22981=CARTESIAN_POINT('Ctrl Pts',(-0.836109320261269,0.828500318394159,
-24.4872616586406));
#22982=CARTESIAN_POINT('Ctrl Pts',(-0.721526697841547,0.930042204780023,
-24.4975228583036));
#22983=CARTESIAN_POINT('Ctrl Pts',(-0.455376345281878,1.08407964668603,
-24.51849818603));
#22984=CARTESIAN_POINT('Ctrl Pts',(-0.30775118021988,1.13503308794979,-24.5289345247244));
#22985=CARTESIAN_POINT('Ctrl Pts',(-0.00686461584989813,1.17680732571145,
-24.5496645175382));
#22986=CARTESIAN_POINT('Ctrl Pts',(0.143039231759763,1.16830684838775,-24.5597266236769));
#22987=CARTESIAN_POINT('Ctrl Pts',(0.442987499421629,1.08927751667137,-24.5808754349717));
#22988=CARTESIAN_POINT('Ctrl Pts',(0.584770051659144,1.02081939625772,-24.5913957171289));
#22989=CARTESIAN_POINT('Ctrl Pts',(0.845152211274036,0.823483142780056,
-24.6137019191628));
#22990=CARTESIAN_POINT('Ctrl Pts',(0.938569142779552,0.703902623820324,
-24.6238544504271));
#22991=CARTESIAN_POINT('Ctrl Pts',(1.08183604106745,0.461156367959846,-24.6430669469338));
#22992=CARTESIAN_POINT('Ctrl Pts',(1.13476537268834,0.312003562781974,-24.6536437922862));
#22993=CARTESIAN_POINT('Ctrl Pts',(1.17999326808417,-0.0132053539140601,
-24.6760689537004));
#22994=CARTESIAN_POINT('Ctrl Pts',(1.16087340945535,-0.163185189932275,
-24.6861776722248));
#22995=CARTESIAN_POINT('Ctrl Pts',(1.0944655738684,-0.430713257112141,-24.704962770341));
#22996=CARTESIAN_POINT('Ctrl Pts',(1.0275278141079,-0.57456497788772,-24.7155699393038));
#22997=CARTESIAN_POINT('Ctrl Pts',(0.847437118499099,-0.815409841666948,
-24.7361124264557));
#22998=CARTESIAN_POINT('Ctrl Pts',(0.737843926148467,-0.914375209208864,
-24.7460123069917));
#22999=CARTESIAN_POINT('Ctrl Pts',(0.506094867186354,-1.05815936007465,
-24.7645976950094));
#23000=CARTESIAN_POINT('Ctrl Pts',(0.361345451250116,-1.12401500207983,
-24.7752142761589));
#23001=CARTESIAN_POINT('Ctrl Pts',(0.041233181178773,-1.17519098782271,
-24.7973572083035));
#23002=CARTESIAN_POINT('Ctrl Pts',(-0.10765796900455,-1.17005527833937,
-24.8073382677247));
#23003=CARTESIAN_POINT('Ctrl Pts',(-0.372894631319849,-1.11196239336716,
-24.8258424020919));
#23004=CARTESIAN_POINT('Ctrl Pts',(-0.521115476638615,-1.05996735950541,
-24.8363291398122));
#23005=CARTESIAN_POINT('Ctrl Pts',(-0.789551161232922,-0.871372502801528,
-24.8587333398721));
#23006=CARTESIAN_POINT('Ctrl Pts',(-0.894024151828209,-0.762659939827989,
-24.8688267952486));
#23007=CARTESIAN_POINT('Ctrl Pts',(-1.04622230392103,-0.531339500064575,
-24.8877001470211));
#23008=CARTESIAN_POINT('Ctrl Pts',(-1.11368038572551,-0.391841775405268,
-24.8980583573751));
#23009=CARTESIAN_POINT('Ctrl Pts',(-1.17367338871164,-0.0713000974155191,
-24.920322632698));
#23010=CARTESIAN_POINT('Ctrl Pts',(-1.17250795556528,0.0812519454809048,
-24.9305283149136));
#23011=CARTESIAN_POINT('Ctrl Pts',(-1.11379701051143,0.37999132682184,-24.9512852188952));
#23012=CARTESIAN_POINT('Ctrl Pts',(-1.05637777413879,0.519409950007713,
-24.9613874349407));
#23013=CARTESIAN_POINT('Ctrl Pts',(-0.886742460300535,0.772183880019197,
-24.9821622194308));
#23014=CARTESIAN_POINT('Ctrl Pts',(-0.777838371540479,0.881492607670479,
-24.9924781493724));
#23015=CARTESIAN_POINT('Ctrl Pts',(-0.525156343273925,1.0533992466795,-25.0133221362559));
#23016=CARTESIAN_POINT('Ctrl Pts',(-0.383871443144776,1.11279922244326,
-25.023593955019));
#23017=CARTESIAN_POINT('Ctrl Pts',(-0.0822383474976909,1.17290119324133,
-25.0445727801414));
#23018=CARTESIAN_POINT('Ctrl Pts',(0.0738049670078393,1.17358654470157,
-25.055000234412));
#23019=CARTESIAN_POINT('Ctrl Pts',(0.306942780668673,1.12890832363886,-25.071200363254));
#23020=CARTESIAN_POINT('Ctrl Pts',(0.388002311516887,1.10401248060482,-25.0769601814217));
#23021=CARTESIAN_POINT('Ctrl Pts',(0.543589168675984,1.03581164825843,-25.0885666806713));
#23022=CARTESIAN_POINT('Ctrl Pts',(0.617180639658102,0.993261974056082,
-25.0943353600971));
#23023=CARTESIAN_POINT('Ctrl Pts',(0.685452938553338,0.943448750455471,
-25.1000986778145));
#23024=CARTESIAN_POINT('Origin',(0.,-1.5,-23.2));
#23025=CARTESIAN_POINT('',(0.,-1.5,-23.2));
#23026=CARTESIAN_POINT('',(-8.54668270915563E-15,-1.33934539329655,-23.2));
#23027=CARTESIAN_POINT('',(0.,-1.5,-23.2));
#23028=CARTESIAN_POINT('',(-1.17966937551839E-5,-1.49965598532183,-23.6078060837911));
#23029=CARTESIAN_POINT('',(0.,-1.5,-23.2));
#23030=CARTESIAN_POINT('Ctrl Pts',(4.62482517256554E-17,-1.16616519702491,
-23.4155261734628));
#23031=CARTESIAN_POINT('Ctrl Pts',(5.33250787523106E-15,-1.22186610458458,
-23.4477077782494));
#23032=CARTESIAN_POINT('Ctrl Pts',(4.91669986271183E-12,-1.277567012145,
-23.4798893830346));
#23033=CARTESIAN_POINT('Ctrl Pts',(4.91669986271183E-12,-1.38870769975953,
-23.5441017242884));
#23034=CARTESIAN_POINT('Ctrl Pts',(2.86542950228376E-14,-1.44414747981368,
-23.5761324607567));
#23035=CARTESIAN_POINT('Ctrl Pts',(-2.3555004955933E-17,-1.49958725986734,
-23.6081631972259));
#23036=CARTESIAN_POINT('Ctrl Pts',(-1.84338803809923E-15,-1.33934539329655,
-23.2));
#23037=CARTESIAN_POINT('Ctrl Pts',(-7.75535507767301E-14,-1.31070585588327,
-23.2165467012055));
#23038=CARTESIAN_POINT('Ctrl Pts',(-2.65179795051112E-12,-1.28206631847006,
-23.2330934024111));
#23039=CARTESIAN_POINT('Ctrl Pts',(-2.65179795051112E-12,-1.22433958636177,
-23.2664454420754));
#23040=CARTESIAN_POINT('Ctrl Pts',(-6.50204480007271E-15,-1.1952523916667,
-23.283250780534));
#23041=CARTESIAN_POINT('Ctrl Pts',(1.17253245002305E-16,-1.16616519697187,
-23.3000561189931));
#23042=CARTESIAN_POINT('Origin',(0.,0.,-23.2));
#23043=CARTESIAN_POINT('',(-1.37415215024357,-0.600878825228823,-23.1998750239129));
#23044=CARTESIAN_POINT('Ctrl Pts',(-1.37395140486162,-0.600796654813404,
-23.2));
#23045=CARTESIAN_POINT('Ctrl Pts',(-1.30510436453987,-0.726707931106893,
-23.2));
#23046=CARTESIAN_POINT('Ctrl Pts',(-1.21950806160512,-0.839865179830455,
-23.2));
#23047=CARTESIAN_POINT('Ctrl Pts',(-1.01762571865116,-1.03693888018822,
-23.2));
#23048=CARTESIAN_POINT('Ctrl Pts',(-0.904301269126984,-1.11974701485562,
-23.2));
#23049=CARTESIAN_POINT('Ctrl Pts',(-0.660860104715333,-1.24907445588305,
-23.2));
#23050=CARTESIAN_POINT('Ctrl Pts',(-0.530821098017273,-1.29615412710268,
-23.2));
#23051=CARTESIAN_POINT('Ctrl Pts',(-0.265883748469263,-1.3477441557919,
-23.2));
#23052=CARTESIAN_POINT('Ctrl Pts',(-0.131789325248617,-1.35315533998259,
-23.2));
#23053=CARTESIAN_POINT('Ctrl Pts',(-8.70831184940357E-15,-1.33934539329655,
-23.2));
#23054=CARTESIAN_POINT('',(-1.37630824614812,-0.596469288048168,-23.2));
#23055=CARTESIAN_POINT('Ctrl Pts',(-1.37435083629484,-0.600965705157694,
-23.1998750239129));
#23056=CARTESIAN_POINT('Ctrl Pts',(-1.37500575571379,-0.599467967360972,
-23.1999166826086));
#23057=CARTESIAN_POINT('Ctrl Pts',(-1.37565822682721,-0.597969158987785,
-23.1999583413043));
#23058=CARTESIAN_POINT('Ctrl Pts',(-1.37630824614812,-0.596469288048168,
-23.2));
#23059=CARTESIAN_POINT('Origin',(0.,0.,-23.2));
#23060=CARTESIAN_POINT('Ctrl Pts',(0.6710062646147,-1.380656119664,-23.05156091023));
#23061=CARTESIAN_POINT('Ctrl Pts',(0.3326844530463,-1.545082331076,-23.07106091023));
#23062=CARTESIAN_POINT('Ctrl Pts',(-0.4683422360403,-1.612847596885,-23.11006091023));
#23063=CARTESIAN_POINT('Ctrl Pts',(-1.42946546972,-0.8821571614021,-23.16856091023));
#23064=CARTESIAN_POINT('Ctrl Pts',(-1.651847110892,0.3043759554816,-23.22706091023));
#23065=CARTESIAN_POINT('Ctrl Pts',(-1.021129492522,1.333641902982,-23.28556091023));
#23066=CARTESIAN_POINT('Ctrl Pts',(0.1370469690624,1.674073791154,-23.34406091023));
#23067=CARTESIAN_POINT('Ctrl Pts',(1.224428737161,1.149815288114,-23.40256091023));
#23068=CARTESIAN_POINT('Ctrl Pts',(1.679374972687,0.03165926908636,-23.46106091023));
#23069=CARTESIAN_POINT('Ctrl Pts',(1.266895850185,-1.102849551308,-23.51956091023));
#23070=CARTESIAN_POINT('Ctrl Pts',(0.2000443226221,-1.667718359793,-23.57806091023));
#23071=CARTESIAN_POINT('Ctrl Pts',(-0.9701334287918,-1.371183213173,-23.63656091023));
#23072=CARTESIAN_POINT('Ctrl Pts',(-1.639221290546,-0.3664093696299,-23.69506091023));
#23073=CARTESIAN_POINT('Ctrl Pts',(-1.461624385972,0.8276209410372,-23.75356091023));
#23074=CARTESIAN_POINT('Ctrl Pts',(-0.52907443495,1.594171417921,-23.81206091023));
#23075=CARTESIAN_POINT('Ctrl Pts',(0.6767511671866,1.53730612602,-23.87056091023));
#23076=CARTESIAN_POINT('Ctrl Pts',(1.533023655909,0.686396924418,-23.92906091023));
#23077=CARTESIAN_POINT('Ctrl Pts',(1.597464201167,-0.519047582986,-23.98756091023));
#23078=CARTESIAN_POINT('Ctrl Pts',(0.8367882010172,-1.456395473099,-24.04606091023));
#23079=CARTESIAN_POINT('Ctrl Pts',(-0.3561026739166,-1.641491137051,-24.10456091023));
#23080=CARTESIAN_POINT('Ctrl Pts',(-1.365060658244,-0.9787296188165,-24.16306091023));
#23081=CARTESIAN_POINT('Ctrl Pts',(-1.668942351274,0.1895618522656,-24.22156091023));
#23082=CARTESIAN_POINT('Ctrl Pts',(-1.110787857823,1.259941506756,-24.28006091023));
#23083=CARTESIAN_POINT('Ctrl Pts',(0.02110684019029,1.679540644058,-24.33856091023));
#23084=CARTESIAN_POINT('Ctrl Pts',(1.142099513493,1.231629392261,-24.39706091023));
#23085=CARTESIAN_POINT('Ctrl Pts',(1.673178974659,0.1475613323174,-24.45556091023));
#23086=CARTESIAN_POINT('Ctrl Pts',(1.340034041364,-1.012724728735,-24.51406091023));
#23087=CARTESIAN_POINT('Ctrl Pts',(0.3147391875509,-1.649921262663,-24.57256091023));
#23088=CARTESIAN_POINT('Ctrl Pts',(-0.8731225586908,-1.434908334168,-24.63106091023));
#23089=CARTESIAN_POINT('Ctrl Pts',(-1.610006155319,-0.4787341075376,-24.68956091023));
#23090=CARTESIAN_POINT('Ctrl Pts',(-1.515280082606,0.7246860501608,-24.74806091023));
#23091=CARTESIAN_POINT('Ctrl Pts',(-0.6379428881994,1.553898857047,-24.80656091023));
#23092=CARTESIAN_POINT('Ctrl Pts',(0.569111203504,1.580105774587,-24.86506091023));
#23093=CARTESIAN_POINT('Ctrl Pts',(1.177323984063,1.054450848381,-24.90406091023));
#23094=CARTESIAN_POINT('Ctrl Pts',(1.354384777031,0.7225666776598,-24.92356091023));
#23095=CARTESIAN_POINT('Ctrl Pts',(0.6122628206918,-1.259786167148,-23.12915029444));
#23096=CARTESIAN_POINT('Ctrl Pts',(0.303559493203,-1.409817636753,-23.14865029444));
#23097=CARTESIAN_POINT('Ctrl Pts',(-0.4273410750521,-1.471650372119,-23.18765029444));
#23098=CARTESIAN_POINT('Ctrl Pts',(-1.304322488069,-0.804928449131,-23.24615029444));
#23099=CARTESIAN_POINT('Ctrl Pts',(-1.507235662021,0.2777292715157,-23.30465029444));
#23100=CARTESIAN_POINT('Ctrl Pts',(-0.9317344059998,1.216887824112,-23.36315029444));
#23101=CARTESIAN_POINT('Ctrl Pts',(0.1250491512082,1.527516500918,-23.42165029444));
#23102=CARTESIAN_POINT('Ctrl Pts',(1.117235757524,1.049154365167,-23.48015029444));
#23103=CARTESIAN_POINT('Ctrl Pts',(1.53235358893,0.02888764891485,-23.53865029444));
#23104=CARTESIAN_POINT('Ctrl Pts',(1.15598507445,-1.006300257822,-23.59715029444));
#23105=CARTESIAN_POINT('Ctrl Pts',(0.1825313826277,-1.521717457694,-23.65565029444));
#23106=CARTESIAN_POINT('Ctrl Pts',(-0.8852028079061,-1.251142569086,-23.71415029444));
#23107=CARTESIAN_POINT('Ctrl Pts',(-1.495715172889,-0.3343319518877,-23.77265029444));
#23108=CARTESIAN_POINT('Ctrl Pts',(-1.333666042389,0.7551666184726,-23.83115029444));
#23109=CARTESIAN_POINT('Ctrl Pts',(-0.4827564554623,1.454609204823,-23.88965029444));
#23110=CARTESIAN_POINT('Ctrl Pts',(0.6175047840515,1.402722201892,-23.94815029444));
#23111=CARTESIAN_POINT('Ctrl Pts',(1.398814641906,0.6263061005841,-24.00665029444));
#23112=CARTESIAN_POINT('Ctrl Pts',(1.457613720376,-0.4736074072494,-24.06515029444));
#23113=CARTESIAN_POINT('Ctrl Pts',(0.7635313279386,-1.328894896257,-24.12365029444));
#23114=CARTESIAN_POINT('Ctrl Pts',(-0.3249275589301,-1.497786305004,-24.18215029444));
#23115=CARTESIAN_POINT('Ctrl Pts',(-1.245556015057,-0.8930464419066,-24.24065029444));
#23116=CARTESIAN_POINT('Ctrl Pts',(-1.522834294475,0.1729666032706,-24.29915029444));
#23117=CARTESIAN_POINT('Ctrl Pts',(-1.013543602922,1.149639551094,-24.35765029444));
#23118=CARTESIAN_POINT('Ctrl Pts',(0.01925903555941,1.532504756551,-24.41615029444));
#23119=CARTESIAN_POINT('Ctrl Pts',(1.042114070341,1.123806029122,-24.47465029444));
#23120=CARTESIAN_POINT('Ctrl Pts',(1.5267000214,0.1346430313905,-24.53315029444));
#23121=CARTESIAN_POINT('Ctrl Pts',(1.22272036083,-0.9240654397699,-24.59165029444));
#23122=CARTESIAN_POINT('Ctrl Pts',(0.2871852513371,-1.50547841275,-24.65015029444));
#23123=CARTESIAN_POINT('Ctrl Pts',(-0.7966847834135,-1.309288855323,-24.70865029444));
#23124=CARTESIAN_POINT('Ctrl Pts',(-1.469057685405,-0.4368231870542,-24.76715029444));
#23125=CARTESIAN_POINT('Ctrl Pts',(-1.38262443503,0.6612431933735,-24.82565029444));
#23126=CARTESIAN_POINT('Ctrl Pts',(-0.5820939874436,1.417862317323,-24.88415029444));
#23127=CARTESIAN_POINT('Ctrl Pts',(0.5192881931508,1.441774942437,-24.94265029444));
#23128=CARTESIAN_POINT('Ctrl Pts',(1.07425480411,0.9621386338044,-24.98165029444));
#23129=CARTESIAN_POINT('Ctrl Pts',(1.235814757055,0.6593093619714,-25.00115029444));
#23130=CARTESIAN_POINT('Ctrl Pts',(0.5535193767689,-1.138916214631,-23.20673967864));
#23131=CARTESIAN_POINT('Ctrl Pts',(0.2744345333596,-1.27455294243,-23.22623967864));
#23132=CARTESIAN_POINT('Ctrl Pts',(-0.3863399140639,-1.330453147354,-23.26523967864));
#23133=CARTESIAN_POINT('Ctrl Pts',(-1.179179506419,-0.72769973686,-23.32373967864));
#23134=CARTESIAN_POINT('Ctrl Pts',(-1.362624213149,0.2510825875499,-23.38223967864));
#23135=CARTESIAN_POINT('Ctrl Pts',(-0.8423393194779,1.100133745242,-23.44073967864));
#23136=CARTESIAN_POINT('Ctrl Pts',(0.1130513333539,1.380959210682,-23.49923967864));
#23137=CARTESIAN_POINT('Ctrl Pts',(1.010042777888,0.9484934422207,-23.55773967864));
#23138=CARTESIAN_POINT('Ctrl Pts',(1.385332205172,0.02611602874334,-23.61623967864));
#23139=CARTESIAN_POINT('Ctrl Pts',(1.045074298715,-0.9097509643373,-23.67473967864));
#23140=CARTESIAN_POINT('Ctrl Pts',(0.1650184426333,-1.375716555595,-23.73323967864));
#23141=CARTESIAN_POINT('Ctrl Pts',(-0.8002721870203,-1.131101924998,-23.79173967864));
#23142=CARTESIAN_POINT('Ctrl Pts',(-1.352209055232,-0.3022545341455,-23.85023967864));
#23143=CARTESIAN_POINT('Ctrl Pts',(-1.205707698806,0.682712295908,-23.90873967864));
#23144=CARTESIAN_POINT('Ctrl Pts',(-0.4364384759746,1.315046991726,-23.96723967864));
#23145=CARTESIAN_POINT('Ctrl Pts',(0.5582584009165,1.268138277765,-24.02573967864));
#23146=CARTESIAN_POINT('Ctrl Pts',(1.264605627904,0.5662152767502,-24.08423967864));
#23147=CARTESIAN_POINT('Ctrl Pts',(1.317763239585,-0.4281672315128,-24.14273967864));
#23148=CARTESIAN_POINT('Ctrl Pts',(0.6902744548601,-1.201394319414,-24.20123967864));
#23149=CARTESIAN_POINT('Ctrl Pts',(-0.2937524439436,-1.354081472956,-24.25973967864));
#23150=CARTESIAN_POINT('Ctrl Pts',(-1.12605137187,-0.8073632649967,-24.31823967864));
#23151=CARTESIAN_POINT('Ctrl Pts',(-1.376726237677,0.1563713542756,-24.37673967864));
#23152=CARTESIAN_POINT('Ctrl Pts',(-0.9162993480212,1.039337595432,-24.43523967864));
#23153=CARTESIAN_POINT('Ctrl Pts',(0.01741123092852,1.385468869044,-24.49373967864));
#23154=CARTESIAN_POINT('Ctrl Pts',(0.9421286271891,1.015982665983,-24.55223967864));
#23155=CARTESIAN_POINT('Ctrl Pts',(1.380221068141,0.1217247304635,-24.61073967864));
#23156=CARTESIAN_POINT('Ctrl Pts',(1.105406680295,-0.8354061508049,-24.66923967864));
#23157=CARTESIAN_POINT('Ctrl Pts',(0.2596313151233,-1.361035562837,-24.72773967864));
#23158=CARTESIAN_POINT('Ctrl Pts',(-0.7202470081362,-1.183669376478,-24.78623967864));
#23159=CARTESIAN_POINT('Ctrl Pts',(-1.32810921549,-0.3949122665708,-24.84473967864));
#23160=CARTESIAN_POINT('Ctrl Pts',(-1.249968787454,0.5978003365862,-24.90323967864));
#23161=CARTESIAN_POINT('Ctrl Pts',(-0.5262450866879,1.2818257776,-24.96173967864));
#23162=CARTESIAN_POINT('Ctrl Pts',(0.4694651827977,1.303444110288,-25.02023967864));
#23163=CARTESIAN_POINT('Ctrl Pts',(0.9711856241576,0.8698264192279,-25.05923967864));
#23164=CARTESIAN_POINT('Ctrl Pts',(1.117244737079,0.5960520462829,-25.07873967864));
#23165=CARTESIAN_POINT('Ctrl Pts',(0.494775932846,-1.018046262115,-23.28432906285));
#23166=CARTESIAN_POINT('Ctrl Pts',(0.2453095735162,-1.139288248107,-23.30382906285));
#23167=CARTESIAN_POINT('Ctrl Pts',(-0.3453387530757,-1.189255922589,-23.34282906285));
#23168=CARTESIAN_POINT('Ctrl Pts',(-1.054036524768,-0.6504710245889,-23.40132906285));
#23169=CARTESIAN_POINT('Ctrl Pts',(-1.218012764277,0.224435903584,-23.45982906285));
#23170=CARTESIAN_POINT('Ctrl Pts',(-0.752944232956,0.9833796663719,-23.51832906285));
#23171=CARTESIAN_POINT('Ctrl Pts',(0.1010535154996,1.234401920446,-23.57682906285));
#23172=CARTESIAN_POINT('Ctrl Pts',(0.9028497982508,0.8478325192742,-23.63532906285));
#23173=CARTESIAN_POINT('Ctrl Pts',(1.238310821415,0.02334440857184,-23.69382906285));
#23174=CARTESIAN_POINT('Ctrl Pts',(0.9341635229797,-0.8132016708522,-23.75232906285));
#23175=CARTESIAN_POINT('Ctrl Pts',(0.147505502639,-1.229715653496,-23.81082906285));
#23176=CARTESIAN_POINT('Ctrl Pts',(-0.7153415661346,-1.011061280911,-23.86932906285));
#23177=CARTESIAN_POINT('Ctrl Pts',(-1.208702937575,-0.2701771164033,-23.92782906285));
#23178=CARTESIAN_POINT('Ctrl Pts',(-1.077749355224,0.6102579733435,-23.98632906285));
#23179=CARTESIAN_POINT('Ctrl Pts',(-0.390120496487,1.175484778628,-24.04482906285));
#23180=CARTESIAN_POINT('Ctrl Pts',(0.4990120177814,1.133554353637,-24.10332906285));
#23181=CARTESIAN_POINT('Ctrl Pts',(1.130396613902,0.5061244529163,-24.16182906285));
#23182=CARTESIAN_POINT('Ctrl Pts',(1.177912758794,-0.3827270557762,-24.22032906285));
#23183=CARTESIAN_POINT('Ctrl Pts',(0.6170175817815,-1.073893742571,-24.27882906285));
#23184=CARTESIAN_POINT('Ctrl Pts',(-0.2625773289571,-1.210376640909,-24.33732906285));
#23185=CARTESIAN_POINT('Ctrl Pts',(-1.006546728684,-0.7216800880868,-24.39582906285));
#23186=CARTESIAN_POINT('Ctrl Pts',(-1.230618180878,0.1397761052806,-24.45432906285));
#23187=CARTESIAN_POINT('Ctrl Pts',(-0.8190550931204,0.9290356397707,-24.51282906285));
#23188=CARTESIAN_POINT('Ctrl Pts',(0.01556342629763,1.238432981537,-24.57132906285));
#23189=CARTESIAN_POINT('Ctrl Pts',(0.8421431840371,0.9081593028442,-24.62982906285));
#23190=CARTESIAN_POINT('Ctrl Pts',(1.233742114882,0.1088064295365,-24.68832906285));
#23191=CARTESIAN_POINT('Ctrl Pts',(0.9880929997609,-0.74674686184,-24.74682906285));
#23192=CARTESIAN_POINT('Ctrl Pts',(0.2320773789096,-1.216592712924,-24.80532906285));
#23193=CARTESIAN_POINT('Ctrl Pts',(-0.6438092328589,-1.058049897633,-24.86382906285));
#23194=CARTESIAN_POINT('Ctrl Pts',(-1.187160745576,-0.3530013460875,-24.92232906285));
#23195=CARTESIAN_POINT('Ctrl Pts',(-1.117313139878,0.5343574797989,-24.98082906285));
#23196=CARTESIAN_POINT('Ctrl Pts',(-0.4703961859322,1.145789237877,-25.03932906285));
#23197=CARTESIAN_POINT('Ctrl Pts',(0.4196421724445,1.165113278138,-25.09782906285));
#23198=CARTESIAN_POINT('Ctrl Pts',(0.868116444205,0.7775142046514,-25.13682906285));
#23199=CARTESIAN_POINT('Ctrl Pts',(0.9986747171026,0.5327947305945,-25.15632906285));
#23200=CARTESIAN_POINT('',(0.881417616740998,1.21316726808339,-24.9080680842712));
#23201=CARTESIAN_POINT('',(0.8816778784387,1.213525491562,-24.9078125));
#23202=CARTESIAN_POINT('Ctrl Pts',(0.881292186436105,1.2129552818722,-24.9076220436819));
#23203=CARTESIAN_POINT('Ctrl Pts',(0.813750271409058,1.26196190916497,-24.9033243807288));
#23204=CARTESIAN_POINT('Ctrl Pts',(0.742132286672347,1.30535258528533,-24.8990878485097));
#23205=CARTESIAN_POINT('Ctrl Pts',(0.608818775191422,1.37169837443908,-24.8914037622482));
#23206=CARTESIAN_POINT('Ctrl Pts',(0.548260654619934,1.39706761640043,-24.8879781469134));
#23207=CARTESIAN_POINT('Ctrl Pts',(0.39749304186689,1.44874200558769,-24.8794109477088));
#23208=CARTESIAN_POINT('Ctrl Pts',(0.305935590287384,1.47074921695453,-24.8741977037729));
#23209=CARTESIAN_POINT('Ctrl Pts',(0.15278657673726,1.4927545949536,-24.8656689066726));
#23210=CARTESIAN_POINT('Ctrl Pts',(0.0918784597345684,1.49775789527344,
-24.8623263527439));
#23211=CARTESIAN_POINT('Ctrl Pts',(-0.0886411888191926,1.50144175853413,
-24.852665407421));
#23212=CARTESIAN_POINT('Ctrl Pts',(-0.208315581115914,1.48940022238857,
-24.8466068804931));
#23213=CARTESIAN_POINT('Ctrl Pts',(-0.39236239919342,1.44861653779783,-24.8369761561396));
#23214=CARTESIAN_POINT('Ctrl Pts',(-0.458874442850795,1.4290120499256,-24.8334250708226));
#23215=CARTESIAN_POINT('Ctrl Pts',(-0.63199737795491,1.36460644461159,-24.8237016461764));
#23216=CARTESIAN_POINT('Ctrl Pts',(-0.735128019387501,1.31179606028223,
-24.8173189749409));
#23217=CARTESIAN_POINT('Ctrl Pts',(-0.882982165912429,1.21340966409492,
-24.8075323201994));
#23218=CARTESIAN_POINT('Ctrl Pts',(-0.933036895109152,1.17538518997163,
-24.8040917368683));
#23219=CARTESIAN_POINT('Ctrl Pts',(-1.06916735064738,1.05767099961853,-24.7944542492941));
#23220=CARTESIAN_POINT('Ctrl Pts',(-1.1485937720974,0.970569640255831,-24.7884997685678));
#23221=CARTESIAN_POINT('Ctrl Pts',(-1.25838806744895,0.818037383718444,
-24.7788910714682));
#23222=CARTESIAN_POINT('Ctrl Pts',(-1.2957921674127,0.757516126799102,-24.7752483055596));
#23223=CARTESIAN_POINT('Ctrl Pts',(-1.38323055549452,0.590505260775706,
-24.7653254281035));
#23224=CARTESIAN_POINT('Ctrl Pts',(-1.42510970387548,0.480319881150026,
-24.7588302302505));
#23225=CARTESIAN_POINT('Ctrl Pts',(-1.46898630328235,0.306611347798785,
-24.7489566081849));
#23226=CARTESIAN_POINT('Ctrl Pts',(-1.48049392039261,0.245226787825081,
-24.7455389360445));
#23227=CARTESIAN_POINT('Ctrl Pts',(-1.5024994387051,0.0663503691542141,
-24.7358897487153));
#23228=CARTESIAN_POINT('Ctrl Pts',(-1.50288937912599,-0.0522048494724794,
-24.7299055858667));
#23229=CARTESIAN_POINT('Ctrl Pts',(-1.4817105010691,-0.239134287010421,
-24.7202890613195));
#23230=CARTESIAN_POINT('Ctrl Pts',(-1.4688737986894,-0.308622107701723,
-24.7166706810548));
#23231=CARTESIAN_POINT('Ctrl Pts',(-1.42180898819625,-0.490309138131947,
-24.706791054986));
#23232=CARTESIAN_POINT('Ctrl Pts',(-1.37906692655925,-0.599786657877916,
-24.7003149527047));
#23233=CARTESIAN_POINT('Ctrl Pts',(-1.29526185013709,-0.757783930027831,
-24.6904587784379));
#23234=CARTESIAN_POINT('Ctrl Pts',(-1.26261342105573,-0.811057262292604,
-24.6870394931226));
#23235=CARTESIAN_POINT('Ctrl Pts',(-1.15900292604867,-0.958435669844394,
-24.677393871737));
#23236=CARTESIAN_POINT('Ctrl Pts',(-1.07985190574382,-1.04656613879994,
-24.6714141517122));
#23237=CARTESIAN_POINT('Ctrl Pts',(-0.938821515558382,-1.17101393298127,
-24.6617994293038));
#23238=CARTESIAN_POINT('Ctrl Pts',(-0.882652752376579,-1.21398931661285,
-24.658178068226));
#23239=CARTESIAN_POINT('Ctrl Pts',(-0.725847001858296,-1.31722777390087,
-24.6482956722769));
#23240=CARTESIAN_POINT('Ctrl Pts',(-0.62072554295621,-1.36976964615758,
-24.6418200195264));
#23241=CARTESIAN_POINT('Ctrl Pts',(-0.452588776858701,-1.43077115137843,
-24.631963162524));
#23242=CARTESIAN_POINT('Ctrl Pts',(-0.392626605356742,-1.44839704644404,
-24.6285429153169));
#23243=CARTESIAN_POINT('Ctrl Pts',(-0.216923859472755,-1.48823041094892,
-24.6188968450495));
#23244=CARTESIAN_POINT('Ctrl Pts',(-0.0991174670356461,-1.50051832964543,
-24.6129175660533));
#23245=CARTESIAN_POINT('Ctrl Pts',(0.0889566198733414,-1.49824840253018,
-24.6033027545031));
#23246=CARTESIAN_POINT('Ctrl Pts',(0.159453701695883,-1.49245512572619,
-24.5996808117517));
#23247=CARTESIAN_POINT('Ctrl Pts',(0.345044403354946,-1.46386267850922,
-24.589796258383));
#23248=CARTESIAN_POINT('Ctrl Pts',(0.458284854486528,-1.43232338869741,
-24.5833189041695));
#23249=CARTESIAN_POINT('Ctrl Pts',(0.623927363713742,-1.36479135546227,
-24.5734609757527));
#23250=CARTESIAN_POINT('Ctrl Pts',(0.68021580859676,-1.33765248581722,-24.57004128029));
#23251=CARTESIAN_POINT('Ctrl Pts',(0.837251949738321,-1.24935791899591,
-24.5603955359266));
#23252=CARTESIAN_POINT('Ctrl Pts',(0.932878002667334,-1.17945695385794,
-24.5544160740831));
#23253=CARTESIAN_POINT('Ctrl Pts',(1.07085431523807,-1.05163277204398,-24.5448013759728));
#23254=CARTESIAN_POINT('Ctrl Pts',(1.11925441241422,-1.00005817266383,-24.5411797608701));
#23255=CARTESIAN_POINT('Ctrl Pts',(1.23773373934732,-0.854379964570187,
-24.5312954975683));
#23256=CARTESIAN_POINT('Ctrl Pts',(1.30057562534765,-0.755035607038862,
-24.524818073943));
#23257=CARTESIAN_POINT('Ctrl Pts',(1.37814483295167,-0.593849848204767,
-24.5149601914699));
#23258=CARTESIAN_POINT('Ctrl Pts',(1.40169350712799,-0.535969264020991,
-24.511540594146));
#23259=CARTESIAN_POINT('Ctrl Pts',(1.45894404008101,-0.365186416635365,
-24.5018966389706));
#23260=CARTESIAN_POINT('Ctrl Pts',(1.48298857842733,-0.249234655671714,
-24.4959186763304));
#23261=CARTESIAN_POINT('Ctrl Pts',(1.49961006934388,-0.0619021396642318,
-24.4863049087931));
#23262=CARTESIAN_POINT('Ctrl Pts',(1.50092325670157,0.00882732721460973,
-24.4826826532579));
#23263=CARTESIAN_POINT('Ctrl Pts',(1.49110174781038,0.196414588786735,-24.4727948396999));
#23264=CARTESIAN_POINT('Ctrl Pts',(1.47107248443378,0.312304732375535,-24.4663142250903));
#23265=CARTESIAN_POINT('Ctrl Pts',(1.42047933685597,0.483918369138487,-24.4564543923671));
#23266=CARTESIAN_POINT('Ctrl Pts',(1.39912933998889,0.542625566360721,-24.4530358789866));
#23267=CARTESIAN_POINT('Ctrl Pts',(1.32710453912062,0.707560423036113,-24.443400022294));
#23268=CARTESIAN_POINT('Ctrl Pts',(1.26724730078268,0.809584908205953,-24.4374283054397));
#23269=CARTESIAN_POINT('Ctrl Pts',(1.15401414708386,0.959645746089114,-24.427818696445));
#23270=CARTESIAN_POINT('Ctrl Pts',(1.10752727641671,1.01303417658909,-24.4241940858983));
#23271=CARTESIAN_POINT('Ctrl Pts',(0.9742325963301,1.14581559669533,-24.4142908555267));
#23272=CARTESIAN_POINT('Ctrl Pts',(0.88143995646911,1.21848666838532,-24.407795873451));
#23273=CARTESIAN_POINT('Ctrl Pts',(0.728639877624673,1.31187350357391,-24.3979274052997));
#23274=CARTESIAN_POINT('Ctrl Pts',(0.67349734345046,1.34104294964111,-24.3945138908));
#23275=CARTESIAN_POINT('Ctrl Pts',(0.510072211568302,1.41475472021774,-24.3849160593254));
#23276=CARTESIAN_POINT('Ctrl Pts',(0.397850923756175,1.45014455786576,-24.3789737568079));
#23277=CARTESIAN_POINT('Ctrl Pts',(0.21361703934987,1.48561996992641,-24.3693836366579));
#23278=CARTESIAN_POINT('Ctrl Pts',(0.143103616043984,1.49412400232197,-24.3657478588718));
#23279=CARTESIAN_POINT('Ctrl Pts',(-0.0462245798991654,1.50338481745475,
-24.3557722684762));
#23280=CARTESIAN_POINT('Ctrl Pts',(-0.16497506476068,1.49489169683256,-24.3492099394591));
#23281=CARTESIAN_POINT('Ctrl Pts',(-0.341635297904301,1.46122051886648,
-24.339300929914));
#23282=CARTESIAN_POINT('Ctrl Pts',(-0.40168846752061,1.44588807069254,-24.3359106954327));
#23283=CARTESIAN_POINT('Ctrl Pts',(-0.569165069113878,1.39179256958006,
-24.326492277347));
#23284=CARTESIAN_POINT('Ctrl Pts',(-0.673574380521842,1.34419321597958,
-24.3206893223395));
#23285=CARTESIAN_POINT('Ctrl Pts',(-0.832983653401516,1.24859302731924,
-24.3111902997536));
#23286=CARTESIAN_POINT('Ctrl Pts',(-0.89205425273673,1.20717492033352,-24.3075009205939));
#23287=CARTESIAN_POINT('Ctrl Pts',(-1.04426960828044,1.08314089363536,-24.2971765530218));
#23288=CARTESIAN_POINT('Ctrl Pts',(-1.13034759047191,0.99276491454057,-24.2902882687428));
#23289=CARTESIAN_POINT('Ctrl Pts',(-1.23975512101156,0.845378328185136,
-24.2801829784649));
#23290=CARTESIAN_POINT('Ctrl Pts',(-1.27261687360187,0.795087916784433,
-24.2769030093859));
#23291=CARTESIAN_POINT('Ctrl Pts',(-1.35016124987809,0.659084689820279,
-24.2685413130271));
#23292=CARTESIAN_POINT('Ctrl Pts',(-1.38976628412931,0.570545163521608,
-24.2635940533201));
#23293=CARTESIAN_POINT('Ctrl Pts',(-1.45734660921659,0.370092757231955,
-24.2527865695785));
#23294=CARTESIAN_POINT('Ctrl Pts',(-1.48171110516211,0.256732925585599,
-24.2469103074676));
#23295=CARTESIAN_POINT('Ctrl Pts',(-1.49878345438743,0.0772267943211951,
-24.2372239416081));
#23296=CARTESIAN_POINT('Ctrl Pts',(-1.50069825172818,0.0122604498412598,
-24.2336574519884));
#23297=CARTESIAN_POINT('Ctrl Pts',(-1.49442141966965,-0.166418379349362,
-24.2237960813223));
#23298=CARTESIAN_POINT('Ctrl Pts',(-1.47747513477829,-0.280015777404685,
-24.2174920903743));
#23299=CARTESIAN_POINT('Ctrl Pts',(-1.42862829365822,-0.460529189075349,
-24.2076773817912));
#23300=CARTESIAN_POINT('Ctrl Pts',(-1.40465643945064,-0.528987438284961,
-24.203972765019));
#23301=CARTESIAN_POINT('Ctrl Pts',(-1.32987150064611,-0.701764400345165,
-24.1943537829878));
#23302=CARTESIAN_POINT('Ctrl Pts',(-1.27151458210261,-0.803020441266229,
-24.1884335009969));
#23303=CARTESIAN_POINT('Ctrl Pts',(-1.16311715722858,-0.948414882803426,
-24.1786901896031));
#23304=CARTESIAN_POINT('Ctrl Pts',(-1.12085812636559,-0.99796742210812,
-24.1751161589507));
#23305=CARTESIAN_POINT('Ctrl Pts',(-0.996464372208961,-1.12603876221773,
-24.1652683401806));
#23306=CARTESIAN_POINT('Ctrl Pts',(-0.907991374518774,-1.19866787009211,
-24.158986199618));
#23307=CARTESIAN_POINT('Ctrl Pts',(-0.751094390359184,-1.29958205710181,
-24.1491949064351));
#23308=CARTESIAN_POINT('Ctrl Pts',(-0.687472040199729,-1.33426379509695,
-24.1454937678829));
#23309=CARTESIAN_POINT('Ctrl Pts',(-0.516034566704189,-1.41236834930936,
-24.1358683944185));
#23310=CARTESIAN_POINT('Ctrl Pts',(-0.404651865476461,-1.44841095506151,
-24.1299385363247));
#23311=CARTESIAN_POINT('Ctrl Pts',(-0.226510571785679,-1.48358649221646,
-24.1201828209351));
#23312=CARTESIAN_POINT('Ctrl Pts',(-0.161901953900477,-1.49199639775794,
-24.1166071409542));
#23313=CARTESIAN_POINT('Ctrl Pts',(0.016208666646669,-1.50353686146712,
-24.1067622797767));
#23314=CARTESIAN_POINT('Ctrl Pts',(0.130459101926883,-1.4980701290517,-24.100484909495));
#23315=CARTESIAN_POINT('Ctrl Pts',(0.314420568759343,-1.46771724748399,
-24.0906987270847));
#23316=CARTESIAN_POINT('Ctrl Pts',(0.384857966348204,-1.45077906986724,
-24.0869983458818));
#23317=CARTESIAN_POINT('Ctrl Pts',(0.564433582448083,-1.39373616655142,
-24.0773715740196));
#23318=CARTESIAN_POINT('Ctrl Pts',(0.671265280341864,-1.34575275193793,
-24.071439624749));
#23319=CARTESIAN_POINT('Ctrl Pts',(0.827032804048919,-1.25233919616798,
-24.0616811953725));
#23320=CARTESIAN_POINT('Ctrl Pts',(0.88060050168267,-1.21524032396105,-24.058105150167));
#23321=CARTESIAN_POINT('Ctrl Pts',(1.02044021136514,-1.10434754659587,-24.0482609298713));
#23322=CARTESIAN_POINT('Ctrl Pts',(1.10150410730434,-1.02367874592046,-24.0419846020692));
#23323=CARTESIAN_POINT('Ctrl Pts',(1.21758661059533,-0.877802170786594,
-24.0321995178782));
#23324=CARTESIAN_POINT('Ctrl Pts',(1.25847168705654,-0.818000102121312,
-24.0284992847203));
#23325=CARTESIAN_POINT('Ctrl Pts',(1.35341775156855,-0.655246657205866,
-24.0188722160153));
#23326=CARTESIAN_POINT('Ctrl Pts',(1.40048172163325,-0.547996899633102,
-24.0129398344978));
#23327=CARTESIAN_POINT('Ctrl Pts',(1.45337233543707,-0.374226951070174,
-24.0031808300433));
#23328=CARTESIAN_POINT('Ctrl Pts',(1.46822410367749,-0.310780476710637,
-23.9996046939037));
#23329=CARTESIAN_POINT('Ctrl Pts',(1.49757300893425,-0.134742336175255,
-23.9897607141101));
#23330=CARTESIAN_POINT('Ctrl Pts',(1.50359769498047,-0.0205445865747881,
-23.9834847242317));
#23331=CARTESIAN_POINT('Ctrl Pts',(1.49186521076666,0.1655038259662,-23.9737001202437));
#23332=CARTESIAN_POINT('Ctrl Pts',(1.48208405018167,0.237279392863777,-23.9700000507006));
#23333=CARTESIAN_POINT('Ctrl Pts',(1.443354829439,0.421682017743482,-23.9603728791471));
#23334=CARTESIAN_POINT('Ctrl Pts',(1.40633221427024,0.53280431410137,-23.9544402446658));
#23335=CARTESIAN_POINT('Ctrl Pts',(1.3290170891885,0.697172897033738,-23.9446810631271));
#23336=CARTESIAN_POINT('Ctrl Pts',(1.2974818058085,0.754192951728386,-23.9411050426264));
#23337=CARTESIAN_POINT('Ctrl Pts',(1.20118138229273,0.904458840363217,-23.9312606180205));
#23338=CARTESIAN_POINT('Ctrl Pts',(1.12905258297626,0.993212264983639,-23.9249840655136));
#23339=CARTESIAN_POINT('Ctrl Pts',(0.99555468038911,1.12335461280545,-23.9151984677531));
#23340=CARTESIAN_POINT('Ctrl Pts',(0.94015286025791,1.1700379249029,-23.9114979455082));
#23341=CARTESIAN_POINT('Ctrl Pts',(0.787747907437857,1.28083574158385,-23.9018708469453));
#23342=CARTESIAN_POINT('Ctrl Pts',(0.685767216586177,1.33842155135958,-23.8959387021292));
#23343=CARTESIAN_POINT('Ctrl Pts',(0.518179799229006,1.40848436018197,-23.8861795305405));
#23344=CARTESIAN_POINT('Ctrl Pts',(0.456536185774643,1.42963027762125,-23.8826029416154));
#23345=CARTESIAN_POINT('Ctrl Pts',(0.284344918213945,1.47649031407643,-23.8727597710839));
#23346=CARTESIAN_POINT('Ctrl Pts',(0.171350805511131,1.49394174300891,-23.8664850805791));
#23347=CARTESIAN_POINT('Ctrl Pts',(-0.0149067568169257,1.50094304571182,
-23.8567019973112));
#23348=CARTESIAN_POINT('Ctrl Pts',(-0.0872953159708956,1.49841681252354,
-23.8530022513087));
#23349=CARTESIAN_POINT('Ctrl Pts',(-0.274653153292379,1.47839610883237,
-23.8433751700276));
#23350=CARTESIAN_POINT('Ctrl Pts',(-0.388935673680077,1.4527147936456,-23.8374423246153));
#23351=CARTESIAN_POINT('Ctrl Pts',(-0.560227605017933,1.39229294224809,
-23.8276836033757));
#23352=CARTESIAN_POINT('Ctrl Pts',(-0.620113874544232,1.36664666328502,
-23.8241082892213));
#23353=CARTESIAN_POINT('Ctrl Pts',(-0.779273560583134,1.28592927114846,
-23.814264837881));
#23354=CARTESIAN_POINT('Ctrl Pts',(-0.874816906047994,1.22308003203388,
-23.8079884291192));
#23355=CARTESIAN_POINT('Ctrl Pts',(-1.01765919442854,1.10336579439268,-23.7982060714263));
#23356=CARTESIAN_POINT('Ctrl Pts',(-1.06963151729626,1.05297467866217,-23.7945084502914));
#23357=CARTESIAN_POINT('Ctrl Pts',(-1.19521011167544,0.912456583884857,
-23.7848800324962));
#23358=CARTESIAN_POINT('Ctrl Pts',(-1.26279982894885,0.81670182455948,-23.7789439151475));
#23359=CARTESIAN_POINT('Ctrl Pts',(-1.34935216351238,0.656945061118655,
-23.7691821278869));
#23360=CARTESIAN_POINT('Ctrl Pts',(-1.37656451834724,0.597768821033822,
-23.7656076108186));
#23361=CARTESIAN_POINT('Ctrl Pts',(-1.44058442680957,0.430883963769553,
-23.7557483227243));
#23362=CARTESIAN_POINT('Ctrl Pts',(-1.46934288907299,0.319885892868802,
-23.7494556404723));
#23363=CARTESIAN_POINT('Ctrl Pts',(-1.49499671235264,0.134531929525419,
-23.7396342765976));
#23364=CARTESIAN_POINT('Ctrl Pts',(-1.49970494926013,0.0618465296069818,
-23.7359139852706));
#23365=CARTESIAN_POINT('Ctrl Pts',(-1.49833434475102,-0.12642650271697,
-23.7262924158087));
#23366=CARTESIAN_POINT('Ctrl Pts',(-1.48422494267998,-0.242142611424862,
-23.720383982627));
#23367=CARTESIAN_POINT('Ctrl Pts',(-1.44128641455023,-0.418464996353218,
-23.7106322664842));
#23368=CARTESIAN_POINT('Ctrl Pts',(-1.42162126502408,-0.480979297208294,
-23.7070351775453));
#23369=CARTESIAN_POINT('Ctrl Pts',(-1.35759602968765,-0.646103273059249,
-23.6972677758374));
#23370=CARTESIAN_POINT('Ctrl Pts',(-1.30553330549334,-0.745938503150817,
-23.6910898598436));
#23371=CARTESIAN_POINT('Ctrl Pts',(-1.20289977957849,-0.897698210470899,
-23.6814734943211));
#23372=CARTESIAN_POINT('Ctrl Pts',(-1.15906515562584,-0.953520068604759,
-23.6778476851766));
#23373=CARTESIAN_POINT('Ctrl Pts',(-1.03225726041117,-1.09356592048758,
-23.6682017104795));
#23374=CARTESIAN_POINT('Ctrl Pts',(-0.942582500787517,-1.17197371523185,
-23.6621823589794));
#23375=CARTESIAN_POINT('Ctrl Pts',(-0.792172583544227,-1.27455337196535,
-23.6524064769686));
#23376=CARTESIAN_POINT('Ctrl Pts',(-0.737419037677256,-1.30697126142047,
-23.6489159470707));
#23377=CARTESIAN_POINT('Ctrl Pts',(-0.596280754156468,-1.37890722070677,
-23.640173961861));
#23378=CARTESIAN_POINT('Ctrl Pts',(-0.507594195380326,-1.41402878226614,
-23.6349050185627));
#23379=CARTESIAN_POINT('Ctrl Pts',(-0.316036897635311,-1.46937081547821,
-23.6242553807404));
#23380=CARTESIAN_POINT('Ctrl Pts',(-0.212669147446816,-1.48775200308733,
-23.6189163456654));
#23381=CARTESIAN_POINT('Ctrl Pts',(-0.0724009869030183,-1.49795898083252,
-23.6117213803296));
#23382=CARTESIAN_POINT('Ctrl Pts',(-0.0362014860425619,-1.49928841111174,
-23.6098685598738));
#23383=CARTESIAN_POINT('Ctrl Pts',(-1.44394147025245E-6,-1.4993119708072,
-23.6080042218746));
#23384=CARTESIAN_POINT('Ctrl Pts',(-2.21494460401153E-5,-1.49999999983647,
-23.6076079457077));
#23385=CARTESIAN_POINT('Ctrl Pts',(0.0610512616330307,-1.50000090166462,
-23.6044870183155));
#23386=CARTESIAN_POINT('Ctrl Pts',(0.122065160139671,-1.49627182965613,
-23.6013464945155));
#23387=CARTESIAN_POINT('Ctrl Pts',(0.255962644401841,-1.4798427421027,-23.5941670216917));
#23388=CARTESIAN_POINT('Ctrl Pts',(0.328479811699856,-1.46545266079536,
-23.590095995072));
#23389=CARTESIAN_POINT('Ctrl Pts',(0.483909921285898,-1.42248916477728,
-23.5811996134758));
#23390=CARTESIAN_POINT('Ctrl Pts',(0.565987731379545,-1.3918705780163,-23.5763953841136));
#23391=CARTESIAN_POINT('Ctrl Pts',(0.778985033664735,-1.29043694267683,
-23.5637480203523));
#23392=CARTESIAN_POINT('Ctrl Pts',(0.902815515892788,-1.20705073239231,
-23.5562615648057));
#23393=CARTESIAN_POINT('Ctrl Pts',(1.0491205572373,-1.07323120591599,-23.5461215215063));
#23394=CARTESIAN_POINT('Ctrl Pts',(1.08416347801703,-1.03781900299683,-23.5435591375015));
#23395=CARTESIAN_POINT('Ctrl Pts',(1.17589390811468,-0.935396301720369,
-23.536304716054));
#23396=CARTESIAN_POINT('Ctrl Pts',(1.22855978406094,-0.865060983721391,
-23.5314596871629));
#23397=CARTESIAN_POINT('Ctrl Pts',(1.32009699721817,-0.7174533077395,-23.5218784328483));
#23398=CARTESIAN_POINT('Ctrl Pts',(1.35905270075097,-0.640603367541495,
-23.5171640521621));
#23399=CARTESIAN_POINT('Ctrl Pts',(1.43746671825191,-0.446089540182238,
-23.5059457278048));
#23400=CARTESIAN_POINT('Ctrl Pts',(1.46935172592144,-0.326059318947462,
-23.4996324550146));
#23401=CARTESIAN_POINT('Ctrl Pts',(1.49428732622014,-0.143933261681204,
-23.4902635412337));
#23402=CARTESIAN_POINT('Ctrl Pts',(1.49885342576748,-0.0839599013022765,
-23.4872013986174));
#23403=CARTESIAN_POINT('Ctrl Pts',(1.50081555415856,0.0392886786925357,
-23.4807580546551));
#23404=CARTESIAN_POINT('Ctrl Pts',(1.49782969294123,0.102446272228486,-23.4773443297187));
#23405=CARTESIAN_POINT('Ctrl Pts',(1.4799645131146,0.263653130021101,-23.4684439696149));
#23406=CARTESIAN_POINT('Ctrl Pts',(1.45933379792741,0.3607690875887,-23.4629454401956));
#23407=CARTESIAN_POINT('Ctrl Pts',(1.40014971170343,0.546624578076728,-23.4523907855226));
#23408=CARTESIAN_POINT('Ctrl Pts',(1.3623010153063,0.635103174225821,-23.447349924324));
#23409=CARTESIAN_POINT('Ctrl Pts',(1.27231522371821,0.799754549063724,-23.4376952019255));
#23410=CARTESIAN_POINT('Ctrl Pts',(1.22110731836698,0.875950726096881,-23.4330887732277));
#23411=CARTESIAN_POINT('Ctrl Pts',(1.12501199052552,0.99399205870297,-23.4252319952568));
#23412=CARTESIAN_POINT('Ctrl Pts',(1.08394732001753,1.03861910145001,-23.4220350972597));
#23413=CARTESIAN_POINT('Ctrl Pts',(0.972808301740653,1.1456086397659,-23.4136572393688));
#23414=CARTESIAN_POINT('Ctrl Pts',(0.899384500212469,1.20411084509114,-23.4084404180098));
#23415=CARTESIAN_POINT('Ctrl Pts',(0.744344138092426,1.30550278825905,-23.3983035776558));
#23416=CARTESIAN_POINT('Ctrl Pts',(0.663271081098984,1.34850270185102,-23.3934013753622));
#23417=CARTESIAN_POINT('Ctrl Pts',(0.495787299847338,1.41855102515141,-23.3839263068296));
#23418=CARTESIAN_POINT('Ctrl Pts',(0.409843129215484,1.44572517188591,-23.3793665661827));
#23419=CARTESIAN_POINT('Ctrl Pts',(0.244796967294499,1.48199849690076,-23.3707448905942));
#23420=CARTESIAN_POINT('Ctrl Pts',(0.16640320555457,1.49283445240194,-23.3666912231762));
#23421=CARTESIAN_POINT('Ctrl Pts',(0.0337154774817,1.50058903644668,-23.359547166957));
#23422=CARTESIAN_POINT('Ctrl Pts',(-0.0202118811268179,1.50083152916805,
-23.356586196228));
#23423=CARTESIAN_POINT('Ctrl Pts',(-0.141338295927296,1.49484599034754,
-23.3498998826809));
#23424=CARTESIAN_POINT('Ctrl Pts',(-0.208344787705541,1.48698821739586,
-23.346178279403));
#23425=CARTESIAN_POINT('Ctrl Pts',(-0.368108567587156,1.4572384051594,-23.3373357410272));
#23426=CARTESIAN_POINT('Ctrl Pts',(-0.459757384516831,1.43096938147552,
-23.3322987413637));
#23427=CARTESIAN_POINT('Ctrl Pts',(-0.64532285006907,1.35809505391628,-23.3219848572406));
#23428=CARTESIAN_POINT('Ctrl Pts',(-0.738101034400311,1.30998850421461,
-23.3167599218195));
#23429=CARTESIAN_POINT('Ctrl Pts',(-0.875729358686173,1.21933088560281,
-23.3082536226009));
#23430=CARTESIAN_POINT('Ctrl Pts',(-0.924246277437874,1.18297835351376,
-23.3050582831458));
#23431=CARTESIAN_POINT('Ctrl Pts',(-1.02443016465529,1.09797867852197,-23.2979235383796));
#23432=CARTESIAN_POINT('Ctrl Pts',(-1.07511362030052,1.04840106642832,-23.2939982324414));
#23433=CARTESIAN_POINT('Ctrl Pts',(-1.19166537252994,0.917017377479984,
-23.2843259939895));
#23434=CARTESIAN_POINT('Ctrl Pts',(-1.25282046894653,0.831523616904168,
-23.2786523187085));
#23435=CARTESIAN_POINT('Ctrl Pts',(-1.34688514110225,0.665772338535599,
-23.2686518583943));
#23436=CARTESIAN_POINT('Ctrl Pts',(-1.38273478368918,0.587705535401598,
-23.2642794417706));
#23437=CARTESIAN_POINT('Ctrl Pts',(-1.44209863967229,0.422409896427763,
-23.255329574732));
#23438=CARTESIAN_POINT('Ctrl Pts',(-1.46481145689039,0.335268966929233,
-23.2507632454323));
#23439=CARTESIAN_POINT('Ctrl Pts',(-1.48800856425733,0.196095877764329,
-23.2432034960859));
#23440=CARTESIAN_POINT('Ctrl Pts',(-1.49383577848236,0.145180448122853,
-23.2403976575781));
#23441=CARTESIAN_POINT('Ctrl Pts',(-1.50469129040932,-0.0275780324609217,
-23.2308668633208));
#23442=CARTESIAN_POINT('Ctrl Pts',(-1.49747999659813,-0.149715711461895,
-23.2241534790374));
#23443=CARTESIAN_POINT('Ctrl Pts',(-1.45503235568658,-0.382007620591668,
-23.2116320695379));
#23444=CARTESIAN_POINT('Ctrl Pts',(-1.42173049413197,-0.491660849941786,
-23.2058275953147));
#23445=CARTESIAN_POINT('Ctrl Pts',(-1.37630824614812,-0.596469288048168,
-23.2));
#23446=CARTESIAN_POINT('Origin',(0.,0.,-32.2));
#23447=CARTESIAN_POINT('Ctrl Pts',(0.494775932846,-1.018046262115,-23.35929593715));
#23448=CARTESIAN_POINT('Ctrl Pts',(0.2453095735162,-1.139288248107,-23.37879593715));
#23449=CARTESIAN_POINT('Ctrl Pts',(-0.3453387530757,-1.189255922589,-23.41779593715));
#23450=CARTESIAN_POINT('Ctrl Pts',(-1.054036524768,-0.6504710245889,-23.47629593715));
#23451=CARTESIAN_POINT('Ctrl Pts',(-1.218012764277,0.224435903584,-23.53479593715));
#23452=CARTESIAN_POINT('Ctrl Pts',(-0.752944232956,0.9833796663719,-23.59329593715));
#23453=CARTESIAN_POINT('Ctrl Pts',(0.1010535154996,1.234401920446,-23.65179593715));
#23454=CARTESIAN_POINT('Ctrl Pts',(0.9028497982508,0.8478325192742,-23.71029593715));
#23455=CARTESIAN_POINT('Ctrl Pts',(1.238310821415,0.02334440857184,-23.76879593715));
#23456=CARTESIAN_POINT('Ctrl Pts',(0.9341635229797,-0.8132016708522,-23.82729593715));
#23457=CARTESIAN_POINT('Ctrl Pts',(0.147505502639,-1.229715653496,-23.88579593715));
#23458=CARTESIAN_POINT('Ctrl Pts',(-0.7153415661346,-1.011061280911,-23.94429593715));
#23459=CARTESIAN_POINT('Ctrl Pts',(-1.208702937575,-0.2701771164033,-24.00279593715));
#23460=CARTESIAN_POINT('Ctrl Pts',(-1.077749355224,0.6102579733435,-24.06129593715));
#23461=CARTESIAN_POINT('Ctrl Pts',(-0.390120496487,1.175484778628,-24.11979593715));
#23462=CARTESIAN_POINT('Ctrl Pts',(0.4990120177814,1.133554353637,-24.17829593715));
#23463=CARTESIAN_POINT('Ctrl Pts',(1.130396613902,0.5061244529163,-24.23679593715));
#23464=CARTESIAN_POINT('Ctrl Pts',(1.177912758794,-0.3827270557762,-24.29529593715));
#23465=CARTESIAN_POINT('Ctrl Pts',(0.6170175817815,-1.073893742571,-24.35379593715));
#23466=CARTESIAN_POINT('Ctrl Pts',(-0.2625773289571,-1.210376640909,-24.41229593715));
#23467=CARTESIAN_POINT('Ctrl Pts',(-1.006546728684,-0.7216800880868,-24.47079593715));
#23468=CARTESIAN_POINT('Ctrl Pts',(-1.230618180878,0.1397761052806,-24.52929593715));
#23469=CARTESIAN_POINT('Ctrl Pts',(-0.8190550931204,0.9290356397707,-24.58779593715));
#23470=CARTESIAN_POINT('Ctrl Pts',(0.01556342629763,1.238432981537,-24.64629593715));
#23471=CARTESIAN_POINT('Ctrl Pts',(0.8421431840371,0.9081593028442,-24.70479593715));
#23472=CARTESIAN_POINT('Ctrl Pts',(1.233742114882,0.1088064295365,-24.76329593715));
#23473=CARTESIAN_POINT('Ctrl Pts',(0.9880929997609,-0.74674686184,-24.82179593715));
#23474=CARTESIAN_POINT('Ctrl Pts',(0.2320773789096,-1.216592712924,-24.88029593715));
#23475=CARTESIAN_POINT('Ctrl Pts',(-0.6438092328589,-1.058049897633,-24.93879593715));
#23476=CARTESIAN_POINT('Ctrl Pts',(-1.187160745576,-0.3530013460875,-24.99729593715));
#23477=CARTESIAN_POINT('Ctrl Pts',(-1.117313139878,0.5343574797989,-25.05579593715));
#23478=CARTESIAN_POINT('Ctrl Pts',(-0.4703961859321,1.145789237877,-25.11429593715));
#23479=CARTESIAN_POINT('Ctrl Pts',(0.4196421724445,1.165113278138,-25.17279593715));
#23480=CARTESIAN_POINT('Ctrl Pts',(0.868116444205,0.7775142046514,-25.21179593715));
#23481=CARTESIAN_POINT('Ctrl Pts',(0.9986747171026,0.5327947305945,-25.23129593715));
#23482=CARTESIAN_POINT('Ctrl Pts',(0.5535193767689,-1.138916214631,-23.43688532136));
#23483=CARTESIAN_POINT('Ctrl Pts',(0.2744345333596,-1.27455294243,-23.45638532136));
#23484=CARTESIAN_POINT('Ctrl Pts',(-0.3863399140639,-1.330453147354,-23.49538532136));
#23485=CARTESIAN_POINT('Ctrl Pts',(-1.179179506419,-0.72769973686,-23.55388532136));
#23486=CARTESIAN_POINT('Ctrl Pts',(-1.362624213149,0.2510825875499,-23.61238532136));
#23487=CARTESIAN_POINT('Ctrl Pts',(-0.8423393194779,1.100133745242,-23.67088532136));
#23488=CARTESIAN_POINT('Ctrl Pts',(0.1130513333539,1.380959210682,-23.72938532136));
#23489=CARTESIAN_POINT('Ctrl Pts',(1.010042777888,0.9484934422207,-23.78788532136));
#23490=CARTESIAN_POINT('Ctrl Pts',(1.385332205172,0.02611602874334,-23.84638532136));
#23491=CARTESIAN_POINT('Ctrl Pts',(1.045074298715,-0.9097509643373,-23.90488532136));
#23492=CARTESIAN_POINT('Ctrl Pts',(0.1650184426333,-1.375716555595,-23.96338532136));
#23493=CARTESIAN_POINT('Ctrl Pts',(-0.8002721870203,-1.131101924998,-24.02188532136));
#23494=CARTESIAN_POINT('Ctrl Pts',(-1.352209055232,-0.3022545341455,-24.08038532136));
#23495=CARTESIAN_POINT('Ctrl Pts',(-1.205707698806,0.682712295908,-24.13888532136));
#23496=CARTESIAN_POINT('Ctrl Pts',(-0.4364384759746,1.315046991726,-24.19738532136));
#23497=CARTESIAN_POINT('Ctrl Pts',(0.5582584009165,1.268138277765,-24.25588532136));
#23498=CARTESIAN_POINT('Ctrl Pts',(1.264605627904,0.5662152767502,-24.31438532136));
#23499=CARTESIAN_POINT('Ctrl Pts',(1.317763239585,-0.4281672315128,-24.37288532136));
#23500=CARTESIAN_POINT('Ctrl Pts',(0.6902744548601,-1.201394319414,-24.43138532136));
#23501=CARTESIAN_POINT('Ctrl Pts',(-0.2937524439436,-1.354081472956,-24.48988532136));
#23502=CARTESIAN_POINT('Ctrl Pts',(-1.12605137187,-0.8073632649967,-24.54838532136));
#23503=CARTESIAN_POINT('Ctrl Pts',(-1.376726237677,0.1563713542756,-24.60688532136));
#23504=CARTESIAN_POINT('Ctrl Pts',(-0.9162993480212,1.039337595432,-24.66538532136));
#23505=CARTESIAN_POINT('Ctrl Pts',(0.01741123092852,1.385468869044,-24.72388532136));
#23506=CARTESIAN_POINT('Ctrl Pts',(0.9421286271891,1.015982665983,-24.78238532136));
#23507=CARTESIAN_POINT('Ctrl Pts',(1.380221068141,0.1217247304635,-24.84088532136));
#23508=CARTESIAN_POINT('Ctrl Pts',(1.105406680295,-0.8354061508049,-24.89938532136));
#23509=CARTESIAN_POINT('Ctrl Pts',(0.2596313151233,-1.361035562837,-24.95788532136));
#23510=CARTESIAN_POINT('Ctrl Pts',(-0.7202470081362,-1.183669376478,-25.01638532136));
#23511=CARTESIAN_POINT('Ctrl Pts',(-1.32810921549,-0.3949122665708,-25.07488532136));
#23512=CARTESIAN_POINT('Ctrl Pts',(-1.249968787454,0.5978003365862,-25.13338532136));
#23513=CARTESIAN_POINT('Ctrl Pts',(-0.5262450866879,1.2818257776,-25.19188532136));
#23514=CARTESIAN_POINT('Ctrl Pts',(0.4694651827977,1.303444110288,-25.25038532136));
#23515=CARTESIAN_POINT('Ctrl Pts',(0.9711856241576,0.8698264192279,-25.28938532136));
#23516=CARTESIAN_POINT('Ctrl Pts',(1.117244737079,0.5960520462829,-25.30888532136));
#23517=CARTESIAN_POINT('Ctrl Pts',(0.6122628206918,-1.259786167148,-23.51447470556));
#23518=CARTESIAN_POINT('Ctrl Pts',(0.303559493203,-1.409817636753,-23.53397470556));
#23519=CARTESIAN_POINT('Ctrl Pts',(-0.4273410750521,-1.471650372119,-23.57297470556));
#23520=CARTESIAN_POINT('Ctrl Pts',(-1.304322488069,-0.804928449131,-23.63147470556));
#23521=CARTESIAN_POINT('Ctrl Pts',(-1.507235662021,0.2777292715157,-23.68997470556));
#23522=CARTESIAN_POINT('Ctrl Pts',(-0.9317344059998,1.216887824112,-23.74847470556));
#23523=CARTESIAN_POINT('Ctrl Pts',(0.1250491512082,1.527516500918,-23.80697470556));
#23524=CARTESIAN_POINT('Ctrl Pts',(1.117235757524,1.049154365167,-23.86547470556));
#23525=CARTESIAN_POINT('Ctrl Pts',(1.53235358893,0.02888764891485,-23.92397470556));
#23526=CARTESIAN_POINT('Ctrl Pts',(1.15598507445,-1.006300257822,-23.98247470556));
#23527=CARTESIAN_POINT('Ctrl Pts',(0.1825313826277,-1.521717457694,-24.04097470556));
#23528=CARTESIAN_POINT('Ctrl Pts',(-0.8852028079061,-1.251142569086,-24.09947470556));
#23529=CARTESIAN_POINT('Ctrl Pts',(-1.495715172889,-0.3343319518877,-24.15797470556));
#23530=CARTESIAN_POINT('Ctrl Pts',(-1.333666042389,0.7551666184726,-24.21647470556));
#23531=CARTESIAN_POINT('Ctrl Pts',(-0.4827564554623,1.454609204823,-24.27497470556));
#23532=CARTESIAN_POINT('Ctrl Pts',(0.6175047840515,1.402722201892,-24.33347470556));
#23533=CARTESIAN_POINT('Ctrl Pts',(1.398814641906,0.6263061005841,-24.39197470556));
#23534=CARTESIAN_POINT('Ctrl Pts',(1.457613720376,-0.4736074072494,-24.45047470556));
#23535=CARTESIAN_POINT('Ctrl Pts',(0.7635313279386,-1.328894896257,-24.50897470556));
#23536=CARTESIAN_POINT('Ctrl Pts',(-0.3249275589301,-1.497786305004,-24.56747470556));
#23537=CARTESIAN_POINT('Ctrl Pts',(-1.245556015057,-0.8930464419066,-24.62597470556));
#23538=CARTESIAN_POINT('Ctrl Pts',(-1.522834294475,0.1729666032706,-24.68447470556));
#23539=CARTESIAN_POINT('Ctrl Pts',(-1.013543602922,1.149639551094,-24.74297470556));
#23540=CARTESIAN_POINT('Ctrl Pts',(0.01925903555941,1.532504756551,-24.80147470556));
#23541=CARTESIAN_POINT('Ctrl Pts',(1.042114070341,1.123806029122,-24.85997470556));
#23542=CARTESIAN_POINT('Ctrl Pts',(1.5267000214,0.1346430313905,-24.91847470556));
#23543=CARTESIAN_POINT('Ctrl Pts',(1.22272036083,-0.9240654397699,-24.97697470556));
#23544=CARTESIAN_POINT('Ctrl Pts',(0.2871852513371,-1.50547841275,-25.03547470556));
#23545=CARTESIAN_POINT('Ctrl Pts',(-0.7966847834135,-1.309288855323,-25.09397470556));
#23546=CARTESIAN_POINT('Ctrl Pts',(-1.469057685405,-0.4368231870542,-25.15247470556));
#23547=CARTESIAN_POINT('Ctrl Pts',(-1.38262443503,0.6612431933735,-25.21097470556));
#23548=CARTESIAN_POINT('Ctrl Pts',(-0.5820939874436,1.417862317323,-25.26947470556));
#23549=CARTESIAN_POINT('Ctrl Pts',(0.5192881931508,1.441774942437,-25.32797470556));
#23550=CARTESIAN_POINT('Ctrl Pts',(1.07425480411,0.9621386338044,-25.36697470556));
#23551=CARTESIAN_POINT('Ctrl Pts',(1.235814757055,0.6593093619714,-25.38647470556));
#23552=CARTESIAN_POINT('Ctrl Pts',(0.6710062646147,-1.380656119664,-23.59206408977));
#23553=CARTESIAN_POINT('Ctrl Pts',(0.3326844530463,-1.545082331076,-23.61156408977));
#23554=CARTESIAN_POINT('Ctrl Pts',(-0.4683422360403,-1.612847596885,-23.65056408977));
#23555=CARTESIAN_POINT('Ctrl Pts',(-1.42946546972,-0.8821571614021,-23.70906408977));
#23556=CARTESIAN_POINT('Ctrl Pts',(-1.651847110892,0.3043759554816,-23.76756408977));
#23557=CARTESIAN_POINT('Ctrl Pts',(-1.021129492522,1.333641902982,-23.82606408977));
#23558=CARTESIAN_POINT('Ctrl Pts',(0.1370469690624,1.674073791154,-23.88456408977));
#23559=CARTESIAN_POINT('Ctrl Pts',(1.224428737161,1.149815288114,-23.94306408977));
#23560=CARTESIAN_POINT('Ctrl Pts',(1.679374972687,0.03165926908636,-24.00156408977));
#23561=CARTESIAN_POINT('Ctrl Pts',(1.266895850185,-1.102849551308,-24.06006408977));
#23562=CARTESIAN_POINT('Ctrl Pts',(0.2000443226221,-1.667718359793,-24.11856408977));
#23563=CARTESIAN_POINT('Ctrl Pts',(-0.9701334287918,-1.371183213173,-24.17706408977));
#23564=CARTESIAN_POINT('Ctrl Pts',(-1.639221290546,-0.3664093696299,-24.23556408977));
#23565=CARTESIAN_POINT('Ctrl Pts',(-1.461624385972,0.8276209410372,-24.29406408977));
#23566=CARTESIAN_POINT('Ctrl Pts',(-0.52907443495,1.594171417921,-24.35256408977));
#23567=CARTESIAN_POINT('Ctrl Pts',(0.6767511671866,1.53730612602,-24.41106408977));
#23568=CARTESIAN_POINT('Ctrl Pts',(1.533023655909,0.686396924418,-24.46956408977));
#23569=CARTESIAN_POINT('Ctrl Pts',(1.597464201167,-0.519047582986,-24.52806408977));
#23570=CARTESIAN_POINT('Ctrl Pts',(0.8367882010172,-1.456395473099,-24.58656408977));
#23571=CARTESIAN_POINT('Ctrl Pts',(-0.3561026739166,-1.641491137051,-24.64506408977));
#23572=CARTESIAN_POINT('Ctrl Pts',(-1.365060658244,-0.9787296188165,-24.70356408977));
#23573=CARTESIAN_POINT('Ctrl Pts',(-1.668942351274,0.1895618522656,-24.76206408977));
#23574=CARTESIAN_POINT('Ctrl Pts',(-1.110787857823,1.259941506756,-24.82056408977));
#23575=CARTESIAN_POINT('Ctrl Pts',(0.02110684019029,1.679540644058,-24.87906408977));
#23576=CARTESIAN_POINT('Ctrl Pts',(1.142099513493,1.231629392261,-24.93756408977));
#23577=CARTESIAN_POINT('Ctrl Pts',(1.673178974659,0.1475613323174,-24.99606408977));
#23578=CARTESIAN_POINT('Ctrl Pts',(1.340034041364,-1.012724728735,-25.05456408977));
#23579=CARTESIAN_POINT('Ctrl Pts',(0.3147391875509,-1.649921262663,-25.11306408977));
#23580=CARTESIAN_POINT('Ctrl Pts',(-0.8731225586908,-1.434908334168,-25.17156408977));
#23581=CARTESIAN_POINT('Ctrl Pts',(-1.610006155319,-0.4787341075376,-25.23006408977));
#23582=CARTESIAN_POINT('Ctrl Pts',(-1.515280082606,0.7246860501608,-25.28856408977));
#23583=CARTESIAN_POINT('Ctrl Pts',(-0.6379428881994,1.553898857047,-25.34706408977));
#23584=CARTESIAN_POINT('Ctrl Pts',(0.569111203504,1.580105774587,-25.40556408977));
#23585=CARTESIAN_POINT('Ctrl Pts',(1.177323984063,1.054450848381,-25.44456408977));
#23586=CARTESIAN_POINT('Ctrl Pts',(1.354384777031,0.7225666776598,-25.46406408977));
#23587=CARTESIAN_POINT('',(0.88141761294346,1.21316727086581,-25.4075569156963));
#23588=CARTESIAN_POINT('Ctrl Pts',(0.881272060753893,1.21292427294373,-24.9076008241125));
#23589=CARTESIAN_POINT('Ctrl Pts',(0.996854232029655,1.12941607459641,-24.9151108232887));
#23590=CARTESIAN_POINT('Ctrl Pts',(1.09903748426639,1.03061271571212,-24.922888098466));
#23591=CARTESIAN_POINT('Ctrl Pts',(1.26828247410366,0.81113931730235,-24.9378733243509));
#23592=CARTESIAN_POINT('Ctrl Pts',(1.33595204838605,0.692845852390926,-24.9448956623844));
#23593=CARTESIAN_POINT('Ctrl Pts',(1.42935208810126,0.46448502774489,-24.9576888333645));
#23594=CARTESIAN_POINT('Ctrl Pts',(1.46035128052924,0.356433930622584,-24.9634772614354));
#23595=CARTESIAN_POINT('Ctrl Pts',(1.49775994046669,0.13564250301949,-24.975383500877));
#23596=CARTESIAN_POINT('Ctrl Pts',(1.50382443165145,0.0241606386654887,
-24.9815225190637));
#23597=CARTESIAN_POINT('Ctrl Pts',(1.48757937945927,-0.248131031019487,
-24.9963697308979));
#23598=CARTESIAN_POINT('Ctrl Pts',(1.45140820792574,-0.40686417356901,-25.0046989308054));
#23599=CARTESIAN_POINT('Ctrl Pts',(1.34071624949762,-0.684366848185125,
-25.0201942046533));
#23600=CARTESIAN_POINT('Ctrl Pts',(1.27196490382923,-0.806121698603482,
-25.0274086698495));
#23601=CARTESIAN_POINT('Ctrl Pts',(1.12526332452217,-0.996878599573301,
-25.0404730867428));
#23602=CARTESIAN_POINT('Ctrl Pts',(1.055053532006,-1.07084246642367,-25.0460952204423));
#23603=CARTESIAN_POINT('Ctrl Pts',(0.900866720644833,-1.20260014134437,
-25.0569359673065));
#23604=CARTESIAN_POINT('Ctrl Pts',(0.818038542621622,-1.26002586650043,
-25.062163772409));
#23605=CARTESIAN_POINT('Ctrl Pts',(0.627936459696357,-1.36593650206767,
-25.0734565570246));
#23606=CARTESIAN_POINT('Ctrl Pts',(0.518806191168035,-1.41129028572528,
-25.0795222275456));
#23607=CARTESIAN_POINT('Ctrl Pts',(0.29457123980294,-1.47502535777107,-25.091885171377));
#23608=CARTESIAN_POINT('Ctrl Pts',(0.180846817453055,-1.49338989670108,
-25.0982048412207));
#23609=CARTESIAN_POINT('Ctrl Pts',(-0.0801360635283695,-1.50447944522687,
-25.1124180147734));
#23610=CARTESIAN_POINT('Ctrl Pts',(-0.22643540767658,-1.48879367987403,
-25.1200025038582));
#23611=CARTESIAN_POINT('Ctrl Pts',(-0.475813301844074,-1.42568036311793,
-25.1333434648599));
#23612=CARTESIAN_POINT('Ctrl Pts',(-0.581342893248654,-1.38632056710971,
-25.1391417409856));
#23613=CARTESIAN_POINT('Ctrl Pts',(-0.780638853926507,-1.28537566237664,
-25.1510164952203));
#23614=CARTESIAN_POINT('Ctrl Pts',(-0.87329259886436,-1.22445335145697,
-25.1571101120661));
#23615=CARTESIAN_POINT('Ctrl Pts',(-1.05143659264298,-1.07599275375337,
-25.1697221953949));
#23616=CARTESIAN_POINT('Ctrl Pts',(-1.13447948010956,-0.98723527130443,
-25.1760565796546));
#23617=CARTESIAN_POINT('Ctrl Pts',(-1.31542362877098,-0.74146902433613,
-25.1919170784518));
#23618=CARTESIAN_POINT('Ctrl Pts',(-1.39834713694402,-0.572369695431689,
-25.2014459946615));
#23619=CARTESIAN_POINT('Ctrl Pts',(-1.47766193566027,-0.281894798315009,
-25.2178464657796));
#23620=CARTESIAN_POINT('Ctrl Pts',(-1.49474758269074,-0.167816718099114,
-25.224163502727));
#23621=CARTESIAN_POINT('Ctrl Pts',(-1.50224798014019,0.0671521060380822,
-25.2366170198868));
#23622=CARTESIAN_POINT('Ctrl Pts',(-1.49184489770568,0.186787458005913,
-25.2427734719892));
#23623=CARTESIAN_POINT('Ctrl Pts',(-1.44764485166995,0.401517274028821,
-25.2541548609197));
#23624=CARTESIAN_POINT('Ctrl Pts',(-1.41786426926399,0.497540003891422,
-25.2593772772489));
#23625=CARTESIAN_POINT('Ctrl Pts',(-1.34056704157422,0.679550937711682,
-25.2699691425619));
#23626=CARTESIAN_POINT('Ctrl Pts',(-1.29385520043036,0.764820066777107,
-25.2753309368534));
#23627=CARTESIAN_POINT('Ctrl Pts',(-1.15764425661784,0.963893360333778,
-25.2884292940504));
#23628=CARTESIAN_POINT('Ctrl Pts',(-1.0589086197412,1.07051008241031,-25.2959099928094));
#23629=CARTESIAN_POINT('Ctrl Pts',(-0.823750133175226,1.2623201806948,-25.3116467956406));
#23630=CARTESIAN_POINT('Ctrl Pts',(-0.68372051272252,1.34425016727509,-25.3199680385646));
#23631=CARTESIAN_POINT('Ctrl Pts',(-0.423365338694491,1.44370500948602,
-25.3351649382959));
#23632=CARTESIAN_POINT('Ctrl Pts',(-0.308952727975757,1.47222251714957,
-25.3416186189514));
#23633=CARTESIAN_POINT('Ctrl Pts',(-0.071322839538722,1.50214058415113,
-25.3542951995422));
#23634=CARTESIAN_POINT('Ctrl Pts',(0.0507139592723535,1.50274269520359,
-25.3605452492806));
#23635=CARTESIAN_POINT('Ctrl Pts',(0.295625083841534,1.47490327186699,-25.3733440948517));
#23636=CARTESIAN_POINT('Ctrl Pts',(0.418716827588455,1.44539674806488,-25.3799246413091));
#23637=CARTESIAN_POINT('Ctrl Pts',(0.659291920030595,1.35366265978716,-25.3939167140426));
#23638=CARTESIAN_POINT('Ctrl Pts',(0.774758582836638,1.29074282062916,-25.4010793596211));
#23639=CARTESIAN_POINT('Ctrl Pts',(0.881231260302741,1.2129539171392,-25.4080241608977));
#23640=CARTESIAN_POINT('',(0.6859379234404,0.9441125563889,-25.21554752692));
#23641=CARTESIAN_POINT('Ctrl Pts',(0.1981104409423,1.114438723627,-25.15929593715));
#23642=CARTESIAN_POINT('Ctrl Pts',(0.47119721649,1.065892903769,-25.17879593715));
#23643=CARTESIAN_POINT('Ctrl Pts',(0.9784120125535,0.7591432259322,-25.21779593715));
#23644=CARTESIAN_POINT('Ctrl Pts',(1.235070736526,-0.09330501139523,-25.27629593715));
#23645=CARTESIAN_POINT('Ctrl Pts',(0.8534729114545,-0.8975024000936,-25.33479593715));
#23646=CARTESIAN_POINT('Ctrl Pts',(0.03112861498029,-1.238140377948,-25.39329593715));
#23647=CARTESIAN_POINT('Ctrl Pts',(-0.80731725562,-0.9392543654266,-25.45179593715));
#23648=CARTESIAN_POINT('Ctrl Pts',(-1.228764281396,-0.1552291200295,-25.51029593715));
#23649=CARTESIAN_POINT('Ctrl Pts',(-1.015535997925,0.7089748153235,-25.56879593715));
#23650=CARTESIAN_POINT('Ctrl Pts',(-0.2777662163492,1.206981513611,-25.62729593715));
#23651=CARTESIAN_POINT('Ctrl Pts',(0.6034742672396,1.081562421011,-25.68579593715));
#23652=CARTESIAN_POINT('Ctrl Pts',(1.173010393869,0.3974985356856,-25.74429593715));
#23653=CARTESIAN_POINT('Ctrl Pts',(1.136667342178,-0.4918798824477,-25.80279593715));
#23654=CARTESIAN_POINT('Ctrl Pts',(0.5132169072275,-1.127194248056,-25.86129593715));
#23655=CARTESIAN_POINT('Ctrl Pts',(-0.3753185056597,-1.180294236991,-25.91979593715));
#23656=CARTESIAN_POINT('Ctrl Pts',(-1.069995734522,-0.6237528313713,-25.97829593715));
#23657=CARTESIAN_POINT('Ctrl Pts',(-1.212002560279,0.2549671752147,-26.03679593715));
#23658=CARTESIAN_POINT('Ctrl Pts',(-0.7279901207168,1.001992440436,-26.09529593715));
#23659=CARTESIAN_POINT('Ctrl Pts',(0.1320411949229,1.231472122869,-26.15379593715));
#23660=CARTESIAN_POINT('Ctrl Pts',(0.9238710607093,0.8248761905421,-26.21229593715));
#23661=CARTESIAN_POINT('Ctrl Pts',(1.238506321788,-0.007781867099203,-26.27079593715));
#23662=CARTESIAN_POINT('Ctrl Pts',(0.9134326886102,-0.8364204625026,-26.32929593715));
#23663=CARTESIAN_POINT('Ctrl Pts',(0.1165560417524,-1.233034125506,-26.38779593715));
#23664=CARTESIAN_POINT('Ctrl Pts',(-0.7405237188655,-0.992765376005,-26.44629593715));
#23665=CARTESIAN_POINT('Ctrl Pts',(-1.215110792527,-0.2397169657051,-26.50479593715));
#23666=CARTESIAN_POINT('Ctrl Pts',(-1.062073152252,0.6371491696676,-26.56329593715));
#23667=CARTESIAN_POINT('Ctrl Pts',(-0.3604572362442,1.184917394878,-26.62179593715));
#23668=CARTESIAN_POINT('Ctrl Pts',(0.5273407111552,1.120655840702,-26.68029593715));
#23669=CARTESIAN_POINT('Ctrl Pts',(1.142758736536,0.4775587757172,-26.73879593715));
#23670=CARTESIAN_POINT('Ctrl Pts',(1.167922203495,-0.412211490328,-26.79729593715));
#23671=CARTESIAN_POINT('Ctrl Pts',(0.5898378721215,-1.089044468041,-26.85579593715));
#23672=CARTESIAN_POINT('Ctrl Pts',(-0.2929195077513,-1.20345490624,-26.91429593715));
#23673=CARTESIAN_POINT('Ctrl Pts',(-1.024334051204,-0.6959369621828,-26.97279593715));
#23674=CARTESIAN_POINT('Ctrl Pts',(-1.1593323394,-0.1187561617546,-27.01179593715));
#23675=CARTESIAN_POINT('Ctrl Pts',(-1.121113703131,0.1559662789859,-27.03129593715));
#23676=CARTESIAN_POINT('Ctrl Pts',(0.2216315720351,1.246753099329,-25.23688532136));
#23677=CARTESIAN_POINT('Ctrl Pts',(0.527141221495,1.192443562085,-25.25638532136));
#23678=CARTESIAN_POINT('Ctrl Pts',(1.094576294964,0.8492743025702,-25.29538532136));
#23679=CARTESIAN_POINT('Ctrl Pts',(1.381707433535,-0.1043828697565,-25.35388532136));
#23680=CARTESIAN_POINT('Ctrl Pts',(0.9548035033152,-1.004060497225,-25.41238532136));
#23681=CARTESIAN_POINT('Ctrl Pts',(0.03482443348539,-1.385141525401,-25.47088532136));
#23682=CARTESIAN_POINT('Ctrl Pts',(-0.9031679079763,-1.050769563483,-25.52938532136));
#23683=CARTESIAN_POINT('Ctrl Pts',(-1.37465222959,-0.1736590647829,-25.58788532136));
#23684=CARTESIAN_POINT('Ctrl Pts',(-1.136107913383,0.793149528647,-25.64638532136));
#23685=CARTESIAN_POINT('Ctrl Pts',(-0.3107446679484,1.350283251132,-25.70488532136));
#23686=CARTESIAN_POINT('Ctrl Pts',(0.6751231782377,1.209973479856,-25.76338532136));
#23687=CARTESIAN_POINT('Ctrl Pts',(1.312278829779,0.4446924903434,-25.82188532136));
#23688=CARTESIAN_POINT('Ctrl Pts',(1.27162086324,-0.5502794859312,-25.88038532136));
#23689=CARTESIAN_POINT('Ctrl Pts',(0.5741497994896,-1.261023053592,-25.93888532136));
#23690=CARTESIAN_POINT('Ctrl Pts',(-0.4198790837452,-1.320427464418,-25.99738532136));
#23691=CARTESIAN_POINT('Ctrl Pts',(-1.197033511132,-0.6978093629019,-26.05588532136));
#23692=CARTESIAN_POINT('Ctrl Pts',(-1.355900433453,0.2852387566824,-26.11438532136));
#23693=CARTESIAN_POINT('Ctrl Pts',(-0.8144224711886,1.120956364969,-26.17288532136));
#23694=CARTESIAN_POINT('Ctrl Pts',(0.1477180983746,1.377681565952,-26.23138532136));
#23695=CARTESIAN_POINT('Ctrl Pts',(1.033559839496,0.9228115690148,-26.28988532136));
#23696=CARTESIAN_POINT('Ctrl Pts',(1.38555091679,-0.008705787692768,-26.34838532136));
#23697=CARTESIAN_POINT('Ctrl Pts',(1.021882146958,-0.9357264619928,-26.40688532136));
#23698=CARTESIAN_POINT('Ctrl Pts',(0.1303944337356,-1.37942902105,-26.46538532136));
#23699=CARTESIAN_POINT('Ctrl Pts',(-0.8284441504486,-1.11063379547,-26.52388532136));
#23700=CARTESIAN_POINT('Ctrl Pts',(-1.359377697933,-0.2681779299465,-26.58238532136));
#23701=CARTESIAN_POINT('Ctrl Pts',(-1.188170301526,0.712796213176,-26.64088532136));
#23702=CARTESIAN_POINT('Ctrl Pts',(-0.403253374937,1.32559951767,-26.69938532136));
#23703=CARTESIAN_POINT('Ctrl Pts',(0.5899504854742,1.253708358346,-26.75788532136));
#23704=CARTESIAN_POINT('Ctrl Pts',(1.278435472814,0.5342580719014,-26.81638532136));
#23705=CARTESIAN_POINT('Ctrl Pts',(1.306586531957,-0.461152275356,-26.87488532136));
#23706=CARTESIAN_POINT('Ctrl Pts',(0.6598677698274,-1.218343850632,-26.93338532136));
#23707=CARTESIAN_POINT('Ctrl Pts',(-0.3276970697449,-1.346337938953,-26.99188532136));
#23708=CARTESIAN_POINT('Ctrl Pts',(-1.145950536365,-0.7785637255274,-27.05038532136));
#23709=CARTESIAN_POINT('Ctrl Pts',(-1.296976815913,-0.1328557681934,-27.08938532136));
#23710=CARTESIAN_POINT('Ctrl Pts',(-1.254220581577,0.1744837446815,-27.10888532136));
#23711=CARTESIAN_POINT('Ctrl Pts',(0.2451527031279,1.379067475031,-25.31447470556));
#23712=CARTESIAN_POINT('Ctrl Pts',(0.5830852265001,1.318994220401,-25.33397470556));
#23713=CARTESIAN_POINT('Ctrl Pts',(1.210740577374,0.9394053792083,-25.37297470556));
#23714=CARTESIAN_POINT('Ctrl Pts',(1.528344130543,-0.1154607281177,-25.43147470556));
#23715=CARTESIAN_POINT('Ctrl Pts',(1.056134095176,-1.110618594357,-25.48997470556));
#23716=CARTESIAN_POINT('Ctrl Pts',(0.03852025199049,-1.532142672854,-25.54847470556));
#23717=CARTESIAN_POINT('Ctrl Pts',(-0.9990185603326,-1.162284761539,-25.60697470556));
#23718=CARTESIAN_POINT('Ctrl Pts',(-1.520540177784,-0.1920890095362,-25.66547470556));
#23719=CARTESIAN_POINT('Ctrl Pts',(-1.256679828841,0.8773242419706,-25.72397470556));
#23720=CARTESIAN_POINT('Ctrl Pts',(-0.3437231195475,1.493584988654,-25.78247470556));
#23721=CARTESIAN_POINT('Ctrl Pts',(0.7467720892358,1.3383845387,-25.84097470556));
#23722=CARTESIAN_POINT('Ctrl Pts',(1.451547265688,0.4918864450011,-25.89947470556));
#23723=CARTESIAN_POINT('Ctrl Pts',(1.406574384301,-0.6086790894146,-25.95797470556));
#23724=CARTESIAN_POINT('Ctrl Pts',(0.6350826917518,-1.394851859129,-26.01647470556));
#23725=CARTESIAN_POINT('Ctrl Pts',(-0.4644396618308,-1.460560691846,-26.07497470556));
#23726=CARTESIAN_POINT('Ctrl Pts',(-1.324071287741,-0.7718658944325,-26.13347470556));
#23727=CARTESIAN_POINT('Ctrl Pts',(-1.499798306627,0.3155103381501,-26.19197470556));
#23728=CARTESIAN_POINT('Ctrl Pts',(-0.9008548216604,1.239920289503,-26.25047470556));
#23729=CARTESIAN_POINT('Ctrl Pts',(0.1633950018263,1.523891009035,-26.30897470556));
#23730=CARTESIAN_POINT('Ctrl Pts',(1.143248618282,1.020746947487,-26.36747470556));
#23731=CARTESIAN_POINT('Ctrl Pts',(1.532595511792,-0.009629708286341,-26.42597470556));
#23732=CARTESIAN_POINT('Ctrl Pts',(1.130331605306,-1.035032461483,-26.48447470556));
#23733=CARTESIAN_POINT('Ctrl Pts',(0.1442328257187,-1.525823916594,-26.54297470556));
#23734=CARTESIAN_POINT('Ctrl Pts',(-0.9163645820317,-1.228502214935,-26.60147470556));
#23735=CARTESIAN_POINT('Ctrl Pts',(-1.503644603339,-0.296638894188,-26.65997470556));
#23736=CARTESIAN_POINT('Ctrl Pts',(-1.3142674508,0.7884432566844,-26.71847470556));
#23737=CARTESIAN_POINT('Ctrl Pts',(-0.4460495136298,1.466281640462,-26.77697470556));
#23738=CARTESIAN_POINT('Ctrl Pts',(0.6525602597933,1.386760875991,-26.83547470556));
#23739=CARTESIAN_POINT('Ctrl Pts',(1.414112209091,0.5909573680856,-26.89397470556));
#23740=CARTESIAN_POINT('Ctrl Pts',(1.445250860419,-0.510093060384,-26.95247470556));
#23741=CARTESIAN_POINT('Ctrl Pts',(0.7298976675333,-1.347643233224,-27.01097470556));
#23742=CARTESIAN_POINT('Ctrl Pts',(-0.3624746317386,-1.489220971666,-27.06947470556));
#23743=CARTESIAN_POINT('Ctrl Pts',(-1.267567021527,-0.8611904888719,-27.12797470556));
#23744=CARTESIAN_POINT('Ctrl Pts',(-1.434621292425,-0.1469553746322,-27.16697470556));
#23745=CARTESIAN_POINT('Ctrl Pts',(-1.387327460022,0.193001210377,-27.18647470556));
#23746=CARTESIAN_POINT('Ctrl Pts',(0.2686738342207,1.511381850733,-25.39206408977));
#23747=CARTESIAN_POINT('Ctrl Pts',(0.6390292315051,1.445544878716,-25.41156408977));
#23748=CARTESIAN_POINT('Ctrl Pts',(1.326904859784,1.029536455846,-25.45056408977));
#23749=CARTESIAN_POINT('Ctrl Pts',(1.674980827552,-0.126538586479,-25.50906408977));
#23750=CARTESIAN_POINT('Ctrl Pts',(1.157464687037,-1.217176691488,-25.56756408977));
#23751=CARTESIAN_POINT('Ctrl Pts',(0.0422160704956,-1.679143820308,-25.62606408977));
#23752=CARTESIAN_POINT('Ctrl Pts',(-1.094869212689,-1.273799959595,-25.68456408977));
#23753=CARTESIAN_POINT('Ctrl Pts',(-1.666428125978,-0.2105189542896,-25.74306408977));
#23754=CARTESIAN_POINT('Ctrl Pts',(-1.377251744299,0.9614989552941,-25.80156408977));
#23755=CARTESIAN_POINT('Ctrl Pts',(-0.3767015711467,1.636886726176,-25.86006408977));
#23756=CARTESIAN_POINT('Ctrl Pts',(0.818421000234,1.466795597545,-25.91856408977));
#23757=CARTESIAN_POINT('Ctrl Pts',(1.590815701598,0.5390803996589,-25.97706408977));
#23758=CARTESIAN_POINT('Ctrl Pts',(1.541527905363,-0.6670786928981,-26.03556408977));
#23759=CARTESIAN_POINT('Ctrl Pts',(0.6960155840139,-1.528680664665,-26.09406408977));
#23760=CARTESIAN_POINT('Ctrl Pts',(-0.5090002399164,-1.600693919274,-26.15256408977));
#23761=CARTESIAN_POINT('Ctrl Pts',(-1.451109064351,-0.8459224259631,-26.21106408977));
#23762=CARTESIAN_POINT('Ctrl Pts',(-1.643696179801,0.3457819196178,-26.26956408977));
#23763=CARTESIAN_POINT('Ctrl Pts',(-0.9872871721321,1.358884214036,-26.32806408977));
#23764=CARTESIAN_POINT('Ctrl Pts',(0.179071905278,1.670100452118,-26.38656408977));
#23765=CARTESIAN_POINT('Ctrl Pts',(1.252937397068,1.11868232596,-26.44506408977));
#23766=CARTESIAN_POINT('Ctrl Pts',(1.679640106794,-0.01055362887991,-26.50356408977));
#23767=CARTESIAN_POINT('Ctrl Pts',(1.238781063654,-1.134338460973,-26.56206408977));
#23768=CARTESIAN_POINT('Ctrl Pts',(0.1580712177019,-1.672218812138,-26.62056408977));
#23769=CARTESIAN_POINT('Ctrl Pts',(-1.004285013615,-1.3463706344,-26.67906408977));
#23770=CARTESIAN_POINT('Ctrl Pts',(-1.647911508744,-0.3250998584294,-26.73756408977));
#23771=CARTESIAN_POINT('Ctrl Pts',(-1.440364600074,0.8640903001927,-26.79606408977));
#23772=CARTESIAN_POINT('Ctrl Pts',(-0.4888456523225,1.606963763254,-26.85456408977));
#23773=CARTESIAN_POINT('Ctrl Pts',(0.7151700341124,1.519813393635,-26.91306408977));
#23774=CARTESIAN_POINT('Ctrl Pts',(1.549788945368,0.6476566642697,-26.97156408977));
#23775=CARTESIAN_POINT('Ctrl Pts',(1.583915188882,-0.559033845412,-27.03006408977));
#23776=CARTESIAN_POINT('Ctrl Pts',(0.7999275652393,-1.476942615815,-27.08856408977));
#23777=CARTESIAN_POINT('Ctrl Pts',(-0.3972521937322,-1.632104004379,-27.14706408977));
#23778=CARTESIAN_POINT('Ctrl Pts',(-1.389183506688,-0.9438172522165,-27.20556408977));
#23779=CARTESIAN_POINT('Ctrl Pts',(-1.572265768938,-0.161054981071,-27.24456408977));
#23780=CARTESIAN_POINT('Ctrl Pts',(-1.520434338468,0.2115186760726,-27.26406408977));
#23781=CARTESIAN_POINT('',(-1.42616365985445,-0.463388660650263,-26.7080680843046));
#23782=CARTESIAN_POINT('Ctrl Pts',(0.881253915032725,1.21298308849533,-25.4080029023648));
#23783=CARTESIAN_POINT('Ctrl Pts',(0.948747205053193,1.16388095517069,-25.4123014309742));
#23784=CARTESIAN_POINT('Ctrl Pts',(1.01215734643154,1.10916455955355,-25.4165388040928));
#23785=CARTESIAN_POINT('Ctrl Pts',(1.11653475356739,1.0027866261975,-25.4242292869111));
#23786=CARTESIAN_POINT('Ctrl Pts',(1.15943877346581,0.952944924722898,-25.4276606152218));
#23787=CARTESIAN_POINT('Ctrl Pts',(1.25513297297284,0.825512929642758,-25.4362277693364));
#23788=CARTESIAN_POINT('Ctrl Pts',(1.30428073799585,0.745337850901385,-25.4414340950019));
#23789=CARTESIAN_POINT('Ctrl Pts',(1.37248032915429,0.60659522353523,-25.4499560923802));
#23790=CARTESIAN_POINT('Ctrl Pts',(1.39606039550318,0.55021426433255,-25.4532986464789));
#23791=CARTESIAN_POINT('Ctrl Pts',(1.45534760596076,0.379668230731732,-25.4629595930959));
#23792=CARTESIAN_POINT('Ctrl Pts',(1.48087684845796,0.262130059911762,-25.4690181210202));
#23793=CARTESIAN_POINT('Ctrl Pts',(1.49896284899431,0.0744882692565386,
-25.4786488460513));
#23794=CARTESIAN_POINT('Ctrl Pts',(1.50087122287115,0.0051734444455085,
-25.482199931001));
#23795=CARTESIAN_POINT('Ctrl Pts',(1.49311577995529,-0.179378628968762,
-25.4919233531514));
#23796=CARTESIAN_POINT('Ctrl Pts',(1.47475924984555,-0.293780963306843,
-25.4983060220473));
#23797=CARTESIAN_POINT('Ctrl Pts',(1.42687768842866,-0.464801659022707,
-25.5080926753898));
#23798=CARTESIAN_POINT('Ctrl Pts',(1.40618202469664,-0.524156758629176,
-25.5115332595472));
#23799=CARTESIAN_POINT('Ctrl Pts',(1.33629576206914,-0.690000309590655,
-25.5211707534326));
#23800=CARTESIAN_POINT('Ctrl Pts',(1.27800150301672,-0.792455210852014,
-25.5271252390471));
#23801=CARTESIAN_POINT('Ctrl Pts',(1.16686294825516,-0.944010881473911,
-25.5367339393702));
#23802=CARTESIAN_POINT('Ctrl Pts',(1.12086233336162,-0.998286355735829,
-25.5403767034103));
#23803=CARTESIAN_POINT('Ctrl Pts',(0.989045661700086,-1.1330542198356,-25.5502995687537));
#23804=CARTESIAN_POINT('Ctrl Pts',(0.8971946703891,-1.20693269674559,-25.5567947553411));
#23805=CARTESIAN_POINT('Ctrl Pts',(0.74554678902829,-1.30234068942969,-25.5666683706389));
#23806=CARTESIAN_POINT('Ctrl Pts',(0.690722599936893,-1.3322540013091,-25.5700860467031));
#23807=CARTESIAN_POINT('Ctrl Pts',(0.527400614845279,-1.40845860401314,
-25.5797352638084));
#23808=CARTESIAN_POINT('Ctrl Pts',(0.414767928635027,-1.4454651523955,-25.5857194496648));
#23809=CARTESIAN_POINT('Ctrl Pts',(0.230442521142555,-1.48308713066819,
-25.5953359895283));
#23810=CARTESIAN_POINT('Ctrl Pts',(0.160389091951486,-1.49235155293721,
-25.5989543610995));
#23811=CARTESIAN_POINT('Ctrl Pts',(-0.0269482729927231,-1.50373449218106,
-25.608833930586));
#23812=CARTESIAN_POINT('Ctrl Pts',(-0.14427467802895,-1.49691490378518,
-25.615309980205));
#23813=CARTESIAN_POINT('Ctrl Pts',(-0.320435663803831,-1.46603573232472,
-25.6251661227975));
#23814=CARTESIAN_POINT('Ctrl Pts',(-0.381190857378073,-1.45144758868543,
-25.6285854264352));
#23815=CARTESIAN_POINT('Ctrl Pts',(-0.553375930513323,-1.39844997155958,
-25.63823118699));
#23816=CARTESIAN_POINT('Ctrl Pts',(-0.66165399426776,-1.35040561431633,
-25.6442110145844));
#23817=CARTESIAN_POINT('Ctrl Pts',(-0.823592491370934,-1.25473294660535,
-25.6538258085075));
#23818=CARTESIAN_POINT('Ctrl Pts',(-0.881820799163859,-1.21459372231324,
-25.6574471288747));
#23819=CARTESIAN_POINT('Ctrl Pts',(-1.02845778633262,-1.09736796129135,
-25.6673292599762));
#23820=CARTESIAN_POINT('Ctrl Pts',(-1.11090953277994,-1.0136311487283,-25.673804666259));
#23821=CARTESIAN_POINT('Ctrl Pts',(-1.22088174814917,-0.872577001693917,
-25.6836613750646));
#23822=CARTESIAN_POINT('Ctrl Pts',(-1.25617540400088,-0.82099524423784,
-25.6870817080832));
#23823=CARTESIAN_POINT('Ctrl Pts',(-1.34836098934793,-0.666191286462965,
-25.6967284301321));
#23824=CARTESIAN_POINT('Ctrl Pts',(-1.39645522725724,-0.55793791492804,
-25.7027082129281));
#23825=CARTESIAN_POINT('Ctrl Pts',(-1.45241333146443,-0.378360349758196,
-25.7123233593778));
#23826=CARTESIAN_POINT('Ctrl Pts',(-1.46868657398459,-0.309527086480265,
-25.7159451114343));
#23827=CARTESIAN_POINT('Ctrl Pts',(-1.49883862410827,-0.124207863002646,
-25.7258284243131));
#23828=CARTESIAN_POINT('Ctrl Pts',(-1.50383664266925,-0.00678408440194565,
-25.7323046241237));
#23829=CARTESIAN_POINT('Ctrl Pts',(-1.49080266440243,0.171607254565109,
-25.7421618584004));
#23830=CARTESIAN_POINT('Ctrl Pts',(-1.48238670367419,0.233534213274606,
-25.7455819557246));
#23831=CARTESIAN_POINT('Ctrl Pts',(-1.44693248446084,0.410224322075841,
-25.7552307520551));
#23832=CARTESIAN_POINT('Ctrl Pts',(-1.40998370308478,0.522816620307887,
-25.761212572804));
#23833=CARTESIAN_POINT('Ctrl Pts',(-1.33102660310492,0.693560536556842,
-25.7708288393751));
#23834=CARTESIAN_POINT('Ctrl Pts',(-1.29693788925547,0.755510746312485,
-25.7744495618416));
#23835=CARTESIAN_POINT('Ctrl Pts',(-1.19505639779183,0.913108878650343,
-25.7843280172044));
#23836=CARTESIAN_POINT('Ctrl Pts',(-1.12005931210667,1.00350446405672,-25.7908000358875));
#23837=CARTESIAN_POINT('Ctrl Pts',(-0.990794696798901,1.12706282088653,
-25.8006546684764));
#23838=CARTESIAN_POINT('Ctrl Pts',(-0.943003564918622,1.16737140311131,
-25.8040761477679));
#23839=CARTESIAN_POINT('Ctrl Pts',(-0.798069480629218,1.27476199427798,
-25.8137343929126));
#23840=CARTESIAN_POINT('Ctrl Pts',(-0.695012437837789,1.33356033067832,
-25.8197233994126));
#23841=CARTESIAN_POINT('Ctrl Pts',(-0.521828941050238,1.40724748710769,
-25.8293445130506));
#23842=CARTESIAN_POINT('Ctrl Pts',(-0.455042945148829,1.43030527422233,
-25.8329625909461));
#23843=CARTESIAN_POINT('Ctrl Pts',(-0.274113561120321,1.4787555873326,-25.8428226748611));
#23844=CARTESIAN_POINT('Ctrl Pts',(-0.158163903410276,1.49548288672185,
-25.849277389497));
#23845=CARTESIAN_POINT('Ctrl Pts',(0.0203900776809842,1.50051380193253,
-25.8591217185526));
#23846=CARTESIAN_POINT('Ctrl Pts',(0.0829797582305993,1.49837878424183,
-25.8625493155582));
#23847=CARTESIAN_POINT('Ctrl Pts',(0.263360222333621,1.48079426165296,-25.8722540845708));
#23848=CARTESIAN_POINT('Ctrl Pts',(0.379963033263763,1.45506869010588,-25.8782790333735));
#23849=CARTESIAN_POINT('Ctrl Pts',(0.558197182661076,1.39320862390086,-25.8879241287906));
#23850=CARTESIAN_POINT('Ctrl Pts',(0.622912838124379,1.36556959813383,-25.8915286432843));
#23851=CARTESIAN_POINT('Ctrl Pts',(0.787967940386338,1.2808638273995,-25.9012971323364));
#23852=CARTESIAN_POINT('Ctrl Pts',(0.883987225285216,1.21643379367,-25.9076661037997));
#23853=CARTESIAN_POINT('Ctrl Pts',(1.01934069704798,1.10134720045136,-25.9174593264319));
#23854=CARTESIAN_POINT('Ctrl Pts',(1.06479174553287,1.0575007596973,-25.9209173539813));
#23855=CARTESIAN_POINT('Ctrl Pts',(1.18981730196394,0.92051202873792,-25.93085343019));
#23856=CARTESIAN_POINT('Ctrl Pts',(1.26098625819716,0.819986923949259,-25.9370566163374));
#23857=CARTESIAN_POINT('Ctrl Pts',(1.35178546403656,0.652007903132813,-25.9468224726596));
#23858=CARTESIAN_POINT('Ctrl Pts',(1.38037429657283,0.589229391201502,-25.9503606218836));
#23859=CARTESIAN_POINT('Ctrl Pts',(1.44226544638672,0.423877658750142,-25.9596679311729));
#23860=CARTESIAN_POINT('Ctrl Pts',(1.46887074150055,0.31923451481424,-25.9656048447258));
#23861=CARTESIAN_POINT('Ctrl Pts',(1.49346482083203,0.148077541387214,-25.9751425515935));
#23862=CARTESIAN_POINT('Ctrl Pts',(1.49855032812148,0.0823615348455862,
-25.9787596154772));
#23863=CARTESIAN_POINT('Ctrl Pts',(1.5002906590474,-0.0765947816070528,
-25.9872958586034));
#23864=CARTESIAN_POINT('Ctrl Pts',(1.49250160467889,-0.169662813193452,
-25.9920890856491));
#23865=CARTESIAN_POINT('Ctrl Pts',(1.46141131564603,-0.345171139561176,
-26.0012048594846));
#23866=CARTESIAN_POINT('Ctrl Pts',(1.43939852652682,-0.427965168144118,
-26.0055441490584));
#23867=CARTESIAN_POINT('Ctrl Pts',(1.38535767557335,-0.578259379816273,
-26.013876996291));
#23868=CARTESIAN_POINT('Ctrl Pts',(1.35510480727151,-0.645989385614745,
-26.0178480574243));
#23869=CARTESIAN_POINT('Ctrl Pts',(1.27527714079766,-0.794052989329665,
-26.0270564027238));
#23870=CARTESIAN_POINT('Ctrl Pts',(1.22288066943919,-0.87260868724116,-26.0322983947709));
#23871=CARTESIAN_POINT('Ctrl Pts',(1.11488576133415,-1.00554150868028,-26.041616500911));
#23872=CARTESIAN_POINT('Ctrl Pts',(1.06174173650512,-1.06142358200637,-26.0456839391086));
#23873=CARTESIAN_POINT('Ctrl Pts',(0.926636430335163,-1.18318209801484,
-26.055091177317));
#23874=CARTESIAN_POINT('Ctrl Pts',(0.841477682492276,-1.24518505133867,
-26.0603775999692));
#23875=CARTESIAN_POINT('Ctrl Pts',(0.685498525869903,-1.33557195750662,
-26.0696977140141));
#23876=CARTESIAN_POINT('Ctrl Pts',(0.617457126019338,-1.36842541977454,
-26.0736763842373));
#23877=CARTESIAN_POINT('Ctrl Pts',(0.46872051102547,-1.42668206718181,-26.082354879253));
#23878=CARTESIAN_POINT('Ctrl Pts',(0.387881235611041,-1.45073002316929,
-26.0870274468075));
#23879=CARTESIAN_POINT('Ctrl Pts',(0.228505663239964,-1.48393811934091,
-26.0959767891238));
#23880=CARTESIAN_POINT('Ctrl Pts',(0.150177863546774,-1.49392774096055,
-26.1002435028173));
#23881=CARTESIAN_POINT('Ctrl Pts',(-0.00235132932211669,-1.50107685274736,
-26.10824952913));
#23882=CARTESIAN_POINT('Ctrl Pts',(-0.0761386409443736,-1.49908767270109,
-26.1120153566548));
#23883=CARTESIAN_POINT('Ctrl Pts',(-0.261362591202425,-1.48052766734123,
-26.1215250525544));
#23884=CARTESIAN_POINT('Ctrl Pts',(-0.372253221316257,-1.45678768684412,
-26.1272793118747));
#23885=CARTESIAN_POINT('Ctrl Pts',(-0.540398465334221,-1.40008593812626,
-26.1368085074094));
#23886=CARTESIAN_POINT('Ctrl Pts',(-0.600177814013998,-1.37549549714502,
-26.140354478175));
#23887=CARTESIAN_POINT('Ctrl Pts',(-0.761433663825177,-1.29670566194455,
-26.1502529407966));
#23888=CARTESIAN_POINT('Ctrl Pts',(-0.85911880730259,-1.23430151390798,
-26.1566166953978));
#23889=CARTESIAN_POINT('Ctrl Pts',(-1.00482069987022,-1.11509090750047,
-26.1664954267595));
#23890=CARTESIAN_POINT('Ctrl Pts',(-1.05761684173333,-1.06506374863199,
-26.1702095722915));
#23891=CARTESIAN_POINT('Ctrl Pts',(-1.1844001976096,-0.926340335232992,
-26.1798111477295));
#23892=CARTESIAN_POINT('Ctrl Pts',(-1.25261441634892,-0.83211920082608,
-26.1857052765572));
#23893=CARTESIAN_POINT('Ctrl Pts',(-1.34074826464044,-0.674326760409325,
-26.1954147409246));
#23894=CARTESIAN_POINT('Ctrl Pts',(-1.36868794552701,-0.615585478595458,
-26.1989842830473));
#23895=CARTESIAN_POINT('Ctrl Pts',(-1.43485703413466,-0.449600827717206,
-26.2088401621456));
#23896=CARTESIAN_POINT('Ctrl Pts',(-1.46506530207602,-0.338953293629063,
-26.2151353002451));
#23897=CARTESIAN_POINT('Ctrl Pts',(-1.49307424044238,-0.15424442962602,
-26.2249405220094));
#23898=CARTESIAN_POINT('Ctrl Pts',(-1.49872145505749,-0.0819601957990811,
-26.2286437288062));
#23899=CARTESIAN_POINT('Ctrl Pts',(-1.4999128142802,0.10635364717765,-26.2382653050375));
#23900=CARTESIAN_POINT('Ctrl Pts',(-1.48729611729633,0.222621170813189,
-26.2441894727905));
#23901=CARTESIAN_POINT('Ctrl Pts',(-1.44664089724751,0.399454503995218,
-26.2539378222371));
#23902=CARTESIAN_POINT('Ctrl Pts',(-1.42792282839189,0.461843884428479,
-26.257512527193));
#23903=CARTESIAN_POINT('Ctrl Pts',(-1.36567226646368,0.629155145193409,
-26.267359150332));
#23904=CARTESIAN_POINT('Ctrl Pts',(-1.3139744789766,0.731242932312221,-26.2736393537179));
#23905=CARTESIAN_POINT('Ctrl Pts',(-1.2110594246586,0.886786659230229,-26.2834285909181));
#23906=CARTESIAN_POINT('Ctrl Pts',(-1.16680806056728,0.944158793526481,
-26.2871294400225));
#23907=CARTESIAN_POINT('Ctrl Pts',(-1.04136689066287,1.08472802366668,-26.2967553749447));
#23908=CARTESIAN_POINT('Ctrl Pts',(-0.953934620650422,1.16260491289205,
-26.3026860592708));
#23909=CARTESIAN_POINT('Ctrl Pts',(-0.805047877218473,1.26658368501614,
-26.312442864928));
#23910=CARTESIAN_POINT('Ctrl Pts',(-0.749301072162544,1.30031295894254,
-26.3160187086009));
#23911=CARTESIAN_POINT('Ctrl Pts',(-0.590941438505108,1.38263225313536,
-26.3258632125988));
#23912=CARTESIAN_POINT('Ctrl Pts',(-0.484180955146683,1.4236573787086,-26.3321400480036));
#23913=CARTESIAN_POINT('Ctrl Pts',(-0.303595410153914,1.46999439523184,
-26.3419255580418));
#23914=CARTESIAN_POINT('Ctrl Pts',(-0.232307353434979,1.4828716436308,-26.3456257619413));
#23915=CARTESIAN_POINT('Ctrl Pts',(-0.0449665451035471,1.50301868666175,
-26.3552526860981));
#23916=CARTESIAN_POINT('Ctrl Pts',(0.0721499053482647,1.50214624239001,
-26.3611849503045));
#23917=CARTESIAN_POINT('Ctrl Pts',(0.252356788815005,1.47940947106688,-26.3709436521134));
#23918=CARTESIAN_POINT('Ctrl Pts',(0.316329984727802,1.46703825681549,-26.3745196087977));
#23919=CARTESIAN_POINT('Ctrl Pts',(0.489002070828588,1.4218861436686,-26.3843641477804));
#23920=CARTESIAN_POINT('Ctrl Pts',(0.595703752241775,1.38071290442607,-26.390640884777));
#23921=CARTESIAN_POINT('Ctrl Pts',(0.760732886542325,1.29396300726967,-26.4004266802352));
#23922=CARTESIAN_POINT('Ctrl Pts',(0.822251899522651,1.25569822892507,-26.4041272317976));
#23923=CARTESIAN_POINT('Ctrl Pts',(0.974721464626966,1.14499111466233,-26.4137542763936));
#23924=CARTESIAN_POINT('Ctrl Pts',(1.06100126006438,1.06579775744788,-26.4196863404273));
#23925=CARTESIAN_POINT('Ctrl Pts',(1.17942115031437,0.928064769776612,-26.4294454073568));
#23926=CARTESIAN_POINT('Ctrl Pts',(1.21858093601503,0.875972882995377,-26.4330219823601));
#23927=CARTESIAN_POINT('Ctrl Pts',(1.31635792021209,0.7266895236537,-26.4428651778376));
#23928=CARTESIAN_POINT('Ctrl Pts',(1.3678726784997,0.624617905788714,-26.4491399085815));
#23929=CARTESIAN_POINT('Ctrl Pts',(1.43208829773097,0.449639147595743,-26.4589230349693));
#23930=CARTESIAN_POINT('Ctrl Pts',(1.4520550072253,0.380012749941871,-26.4626227873655));
#23931=CARTESIAN_POINT('Ctrl Pts',(1.49091078706645,0.195638319667655,-26.4722498568713));
#23932=CARTESIAN_POINT('Ctrl Pts',(1.50180158407935,0.0790135856532134,
-26.4781826846612));
#23933=CARTESIAN_POINT('Ctrl Pts',(1.49726914081623,-0.102565685129436,
-26.4879413830688));
#23934=CARTESIAN_POINT('Ctrl Pts',(1.49138397176759,-0.167445996749231,
-26.491516694186));
#23935=CARTESIAN_POINT('Ctrl Pts',(1.46380024372253,-0.343759005058039,
-26.5013601509739));
#23936=CARTESIAN_POINT('Ctrl Pts',(1.43355155078388,-0.454047762524838,
-26.5076365685205));
#23937=CARTESIAN_POINT('Ctrl Pts',(1.36383715846955,-0.626892751013256,
-26.517418935626));
#23938=CARTESIAN_POINT('Ctrl Pts',(1.33197267114545,-0.691893101510102,
-26.521116558156));
#23939=CARTESIAN_POINT('Ctrl Pts',(1.23713794533795,-0.854747866201789,
-26.5307449733761));
#23940=CARTESIAN_POINT('Ctrl Pts',(1.16695617220513,-0.948619287037085,
-26.5366810868746));
#23941=CARTESIAN_POINT('Ctrl Pts',(1.04176467010574,-1.08030294138717,-26.5464428691456));
#23942=CARTESIAN_POINT('Ctrl Pts',(0.993893811690886,-1.12446988675267,
-26.5500173855498));
#23943=CARTESIAN_POINT('Ctrl Pts',(0.854960109142449,-1.2369267158239,-26.5598766748324));
#23944=CARTESIAN_POINT('Ctrl Pts',(0.758281496474013,-1.2985779491472,-26.5661693590029));
#23945=CARTESIAN_POINT('Ctrl Pts',(0.589926831790066,-1.3802537244995,-26.5759907249344));
#23946=CARTESIAN_POINT('Ctrl Pts',(0.522253827245407,-1.40719254860585,
-26.5797110165672));
#23947=CARTESIAN_POINT('Ctrl Pts',(0.342772001528536,-1.46406858457962,
-26.5893325854756));
#23948=CARTESIAN_POINT('Ctrl Pts',(0.228359414155081,-1.48640798527583,
-26.5952410178224));
#23949=CARTESIAN_POINT('Ctrl Pts',(0.0473981458182217,-1.50005763135903,
-26.6049927328855));
#23950=CARTESIAN_POINT('Ctrl Pts',(-0.0181333502888847,-1.50067294465087,
-26.6085898216814));
#23951=CARTESIAN_POINT('Ctrl Pts',(-0.19496047411489,-1.49080744377269,
-26.6183572236448));
#23952=CARTESIAN_POINT('Ctrl Pts',(-0.305997694094707,-1.47214363262793,
-26.6245351400502));
#23953=CARTESIAN_POINT('Ctrl Pts',(-0.482045264444345,-1.42142967465588,
-26.6341515060131));
#23954=CARTESIAN_POINT('Ctrl Pts',(-0.548680651270178,-1.39699037194736,
-26.6377773152219));
#23955=CARTESIAN_POINT('Ctrl Pts',(-0.721057963265396,-1.31966544505203,
-26.647423289794));
#23956=CARTESIAN_POINT('Ctrl Pts',(-0.823339228634004,-1.25860902335675,
-26.6534426411113));
#23957=CARTESIAN_POINT('Ctrl Pts',(-0.967377496896887,-1.14725955151277,
-26.6632185228844));
#23958=CARTESIAN_POINT('Ctrl Pts',(-1.01512851775822,-1.10520351414327,
-26.6667090527507));
#23959=CARTESIAN_POINT('Ctrl Pts',(-1.12706752532266,-0.993292725067995,
-26.675443992847));
#23960=CARTESIAN_POINT('Ctrl Pts',(-1.18780019231101,-0.919909652198967,
-26.680705639719));
#23961=CARTESIAN_POINT('Ctrl Pts',(-1.29936775096139,-0.755307651316867,
-26.6913274460603));
#23962=CARTESIAN_POINT('Ctrl Pts',(-1.34865829060901,-0.663077553166124,
-26.6966469113585));
#23963=CARTESIAN_POINT('Ctrl Pts',(-1.40190296279248,-0.532756487150161,
-26.7038489235449));
#23964=CARTESIAN_POINT('Ctrl Pts',(-1.41456019814549,-0.498231485192453,
-26.7057295679761));
#23965=CARTESIAN_POINT('Ctrl Pts',(-1.42593782207381,-0.463290149673335,
-26.7076220835797));
#23966=CARTESIAN_POINT('',(-1.42616365839152,-0.463388665150944,-27.2075569156963));
#23967=CARTESIAN_POINT('Ctrl Pts',(-1.42590316226897,-0.46327735868407,
-26.7076008391022));
#23968=CARTESIAN_POINT('Ctrl Pts',(-1.48022542784997,-0.297586107654068,
-26.7167843685386));
#23969=CARTESIAN_POINT('Ctrl Pts',(-1.50486925637141,-0.125249205425268,
-26.7263745778538));
#23970=CARTESIAN_POINT('Ctrl Pts',(-1.49291374415963,0.209427358776284,
-26.7441959507517));
#23971=CARTESIAN_POINT('Ctrl Pts',(-1.46138855081052,0.368703742541458,
-26.7524076631357));
#23972=CARTESIAN_POINT('Ctrl Pts',(-1.37516087375663,0.603706007214842,
-26.7654670202156));
#23973=CARTESIAN_POINT('Ctrl Pts',(-1.33661136820521,0.68555664639347,-26.7702202361326));
#23974=CARTESIAN_POINT('Ctrl Pts',(-1.2448441354841,0.841472035895783,-26.7800100546894));
#23975=CARTESIAN_POINT('Ctrl Pts',(-1.1916507879262,0.915262310204792,-26.7850425184109));
#23976=CARTESIAN_POINT('Ctrl Pts',(-1.00987125882251,1.12359212643019,-26.7999793803873));
#23977=CARTESIAN_POINT('Ctrl Pts',(-0.86135529066732,1.24034483336812,-26.8094788432607));
#23978=CARTESIAN_POINT('Ctrl Pts',(-0.617304190663664,1.36916322477178,
-26.823865733921));
#23979=CARTESIAN_POINT('Ctrl Pts',(-0.533635780763124,1.40423385403138,
-26.8286254950898));
#23980=CARTESIAN_POINT('Ctrl Pts',(-0.359394154914502,1.45906580714,-26.8384961681381));
#23981=CARTESIAN_POINT('Ctrl Pts',(-0.268988163959942,1.47840340652547,
-26.8436062466654));
#23982=CARTESIAN_POINT('Ctrl Pts',(0.00732540329836662,1.5107086221588,
-26.8586170253155));
#23983=CARTESIAN_POINT('Ctrl Pts',(0.195979873932844,1.49733320545277,-26.8681241570776));
#23984=CARTESIAN_POINT('Ctrl Pts',(0.463267412983477,1.42864141281074,-26.8825180045602));
#23985=CARTESIAN_POINT('Ctrl Pts',(0.548609796066798,1.39844020086262,-26.8872712335173));
#23986=CARTESIAN_POINT('Ctrl Pts',(0.714355014249309,1.32201980761357,-26.8971412079893));
#23987=CARTESIAN_POINT('Ctrl Pts',(0.794334488308791,1.27556785177849,-26.9022544655732));
#23988=CARTESIAN_POINT('Ctrl Pts',(1.02067770564489,1.11375913918672,-26.9172619308146));
#23989=CARTESIAN_POINT('Ctrl Pts',(1.15135498077534,0.977128794457907,-26.9267635866013));
#23990=CARTESIAN_POINT('Ctrl Pts',(1.32471965108333,0.713890117675608,-26.9432059032433));
#23991=CARTESIAN_POINT('Ctrl Pts',(1.38204127770906,0.596833407966587,-26.9501142277202));
#23992=CARTESIAN_POINT('Ctrl Pts',(1.46873900176316,0.336259442922926,-26.9651555553315));
#23993=CARTESIAN_POINT('Ctrl Pts',(1.49355317711586,0.193731144783341,-26.9728184717108));
#23994=CARTESIAN_POINT('Ctrl Pts',(1.50400111145276,-0.134796170383052,
-26.9899382087099));
#23995=CARTESIAN_POINT('Ctrl Pts',(1.47619648535756,-0.321142588299731,
-26.9994252155968));
#23996=CARTESIAN_POINT('Ctrl Pts',(1.38706298095157,-0.576977166917857,
-27.0140901232008));
#23997=CARTESIAN_POINT('Ctrl Pts',(1.35176410527077,-0.655426009430809,
-27.0188416980206));
#23998=CARTESIAN_POINT('Ctrl Pts',(1.26341901571074,-0.813160526073467,
-27.0286181558124));
#23999=CARTESIAN_POINT('Ctrl Pts',(1.20901892461933,-0.891452413251942,
-27.0336144797392));
#24000=CARTESIAN_POINT('Ctrl Pts',(1.0284633921148,-1.10565620989746,-27.0482109139249));
#24001=CARTESIAN_POINT('Ctrl Pts',(0.883116781281584,-1.22570860803761,
-27.0576996903132));
#24002=CARTESIAN_POINT('Ctrl Pts',(0.644888168564368,-1.35688218325702,
-27.0724070805618));
#24003=CARTESIAN_POINT('Ctrl Pts',(0.565309749810226,-1.39191973600915,
-27.0772093561898));
#24004=CARTESIAN_POINT('Ctrl Pts',(0.341617477538992,-1.4675852545328,-27.0899790753639));
#24005=CARTESIAN_POINT('Ctrl Pts',(0.192800060504756,-1.4938398680087,-27.0977154107084));
#24006=CARTESIAN_POINT('Ctrl Pts',(-0.10177151207912,-1.50249575613366,
-27.1130005942386));
#24007=CARTESIAN_POINT('Ctrl Pts',(-0.247967527283484,-1.48610526266758,
-27.1205961668103));
#24008=CARTESIAN_POINT('Ctrl Pts',(-0.499452916756478,-1.41887331687768,
-27.1347845490264));
#24009=CARTESIAN_POINT('Ctrl Pts',(-0.605605262643713,-1.37672641961951,
-27.1410472347818));
#24010=CARTESIAN_POINT('Ctrl Pts',(-0.809424221127998,-1.26706377776192,
-27.1533216201516));
#24011=CARTESIAN_POINT('Ctrl Pts',(-0.905761853669422,-1.19975808356791,
-27.1593547939893));
#24012=CARTESIAN_POINT('Ctrl Pts',(-1.09031963371981,-1.0367207065882,-27.1721305544943));
#24013=CARTESIAN_POINT('Ctrl Pts',(-1.17668388134904,-0.938483389056613,
-27.178901138905));
#24014=CARTESIAN_POINT('Ctrl Pts',(-1.32462526276729,-0.716823167178535,
-27.193351009864));
#24015=CARTESIAN_POINT('Ctrl Pts',(-1.38389132700062,-0.593751662693113,
-27.2008076632993));
#24016=CARTESIAN_POINT('Ctrl Pts',(-1.42588748976423,-0.463325593694253,
-27.2080241608977));
#24017=CARTESIAN_POINT('',(-1.109870874299,-0.360618907335,-27.01554752692));
#24018=CARTESIAN_POINT('Ctrl Pts',(0.2686738342207,1.511381850733,-24.85156091023));
#24019=CARTESIAN_POINT('Ctrl Pts',(0.6390292315051,1.445544878716,-24.87106091023));
#24020=CARTESIAN_POINT('Ctrl Pts',(1.326904859784,1.029536455846,-24.91006091023));
#24021=CARTESIAN_POINT('Ctrl Pts',(1.674980827552,-0.126538586479,-24.96856091023));
#24022=CARTESIAN_POINT('Ctrl Pts',(1.157464687037,-1.217176691488,-25.02706091023));
#24023=CARTESIAN_POINT('Ctrl Pts',(0.0422160704956,-1.679143820308,-25.08556091023));
#24024=CARTESIAN_POINT('Ctrl Pts',(-1.094869212689,-1.273799959595,-25.14406091023));
#24025=CARTESIAN_POINT('Ctrl Pts',(-1.666428125978,-0.2105189542896,-25.20256091023));
#24026=CARTESIAN_POINT('Ctrl Pts',(-1.377251744299,0.9614989552941,-25.26106091023));
#24027=CARTESIAN_POINT('Ctrl Pts',(-0.3767015711466,1.636886726176,-25.31956091023));
#24028=CARTESIAN_POINT('Ctrl Pts',(0.818421000234,1.466795597545,-25.37806091023));
#24029=CARTESIAN_POINT('Ctrl Pts',(1.590815701598,0.5390803996589,-25.43656091023));
#24030=CARTESIAN_POINT('Ctrl Pts',(1.541527905363,-0.6670786928981,-25.49506091023));
#24031=CARTESIAN_POINT('Ctrl Pts',(0.6960155840139,-1.528680664665,-25.55356091023));
#24032=CARTESIAN_POINT('Ctrl Pts',(-0.5090002399164,-1.600693919274,-25.61206091023));
#24033=CARTESIAN_POINT('Ctrl Pts',(-1.451109064351,-0.8459224259632,-25.67056091023));
#24034=CARTESIAN_POINT('Ctrl Pts',(-1.643696179801,0.3457819196178,-25.72906091023));
#24035=CARTESIAN_POINT('Ctrl Pts',(-0.9872871721321,1.358884214036,-25.78756091023));
#24036=CARTESIAN_POINT('Ctrl Pts',(0.179071905278,1.670100452118,-25.84606091023));
#24037=CARTESIAN_POINT('Ctrl Pts',(1.252937397068,1.11868232596,-25.90456091023));
#24038=CARTESIAN_POINT('Ctrl Pts',(1.679640106794,-0.0105536288799,-25.96306091023));
#24039=CARTESIAN_POINT('Ctrl Pts',(1.238781063654,-1.134338460973,-26.02156091023));
#24040=CARTESIAN_POINT('Ctrl Pts',(0.1580712177019,-1.672218812138,-26.08006091023));
#24041=CARTESIAN_POINT('Ctrl Pts',(-1.004285013615,-1.3463706344,-26.13856091023));
#24042=CARTESIAN_POINT('Ctrl Pts',(-1.647911508744,-0.3250998584294,-26.19706091023));
#24043=CARTESIAN_POINT('Ctrl Pts',(-1.440364600074,0.8640903001927,-26.25556091023));
#24044=CARTESIAN_POINT('Ctrl Pts',(-0.4888456523225,1.606963763254,-26.31406091023));
#24045=CARTESIAN_POINT('Ctrl Pts',(0.7151700341124,1.519813393635,-26.37256091023));
#24046=CARTESIAN_POINT('Ctrl Pts',(1.549788945368,0.6476566642697,-26.43106091023));
#24047=CARTESIAN_POINT('Ctrl Pts',(1.583915188882,-0.559033845412,-26.48956091023));
#24048=CARTESIAN_POINT('Ctrl Pts',(0.7999275652393,-1.476942615815,-26.54806091023));
#24049=CARTESIAN_POINT('Ctrl Pts',(-0.3972521937322,-1.632104004379,-26.60656091023));
#24050=CARTESIAN_POINT('Ctrl Pts',(-1.389183506688,-0.9438172522165,-26.66506091023));
#24051=CARTESIAN_POINT('Ctrl Pts',(-1.572265768938,-0.161054981071,-26.70406091023));
#24052=CARTESIAN_POINT('Ctrl Pts',(-1.520434338468,0.2115186760726,-26.72356091023));
#24053=CARTESIAN_POINT('Ctrl Pts',(0.2451527031279,1.379067475031,-24.92915029444));
#24054=CARTESIAN_POINT('Ctrl Pts',(0.5830852265001,1.318994220401,-24.94865029444));
#24055=CARTESIAN_POINT('Ctrl Pts',(1.210740577374,0.9394053792083,-24.98765029444));
#24056=CARTESIAN_POINT('Ctrl Pts',(1.528344130543,-0.1154607281177,-25.04615029444));
#24057=CARTESIAN_POINT('Ctrl Pts',(1.056134095176,-1.110618594357,-25.10465029444));
#24058=CARTESIAN_POINT('Ctrl Pts',(0.0385202519905,-1.532142672854,-25.16315029444));
#24059=CARTESIAN_POINT('Ctrl Pts',(-0.9990185603326,-1.162284761539,-25.22165029444));
#24060=CARTESIAN_POINT('Ctrl Pts',(-1.520540177784,-0.1920890095362,-25.28015029444));
#24061=CARTESIAN_POINT('Ctrl Pts',(-1.256679828841,0.8773242419706,-25.33865029444));
#24062=CARTESIAN_POINT('Ctrl Pts',(-0.3437231195475,1.493584988654,-25.39715029444));
#24063=CARTESIAN_POINT('Ctrl Pts',(0.7467720892358,1.3383845387,-25.45565029444));
#24064=CARTESIAN_POINT('Ctrl Pts',(1.451547265688,0.4918864450011,-25.51415029444));
#24065=CARTESIAN_POINT('Ctrl Pts',(1.406574384301,-0.6086790894146,-25.57265029444));
#24066=CARTESIAN_POINT('Ctrl Pts',(0.6350826917518,-1.394851859129,-25.63115029444));
#24067=CARTESIAN_POINT('Ctrl Pts',(-0.4644396618308,-1.460560691846,-25.68965029444));
#24068=CARTESIAN_POINT('Ctrl Pts',(-1.324071287741,-0.7718658944325,-25.74815029444));
#24069=CARTESIAN_POINT('Ctrl Pts',(-1.499798306627,0.3155103381501,-25.80665029444));
#24070=CARTESIAN_POINT('Ctrl Pts',(-0.9008548216604,1.239920289503,-25.86515029444));
#24071=CARTESIAN_POINT('Ctrl Pts',(0.1633950018263,1.523891009035,-25.92365029444));
#24072=CARTESIAN_POINT('Ctrl Pts',(1.143248618282,1.020746947487,-25.98215029444));
#24073=CARTESIAN_POINT('Ctrl Pts',(1.532595511792,-0.00962970828634,-26.04065029444));
#24074=CARTESIAN_POINT('Ctrl Pts',(1.130331605306,-1.035032461483,-26.09915029444));
#24075=CARTESIAN_POINT('Ctrl Pts',(0.1442328257187,-1.525823916594,-26.15765029444));
#24076=CARTESIAN_POINT('Ctrl Pts',(-0.9163645820317,-1.228502214935,-26.21615029444));
#24077=CARTESIAN_POINT('Ctrl Pts',(-1.503644603339,-0.296638894188,-26.27465029444));
#24078=CARTESIAN_POINT('Ctrl Pts',(-1.3142674508,0.7884432566844,-26.33315029444));
#24079=CARTESIAN_POINT('Ctrl Pts',(-0.4460495136298,1.466281640462,-26.39165029444));
#24080=CARTESIAN_POINT('Ctrl Pts',(0.6525602597933,1.386760875991,-26.45015029444));
#24081=CARTESIAN_POINT('Ctrl Pts',(1.414112209091,0.5909573680856,-26.50865029444));
#24082=CARTESIAN_POINT('Ctrl Pts',(1.445250860419,-0.510093060384,-26.56715029444));
#24083=CARTESIAN_POINT('Ctrl Pts',(0.7298976675334,-1.347643233224,-26.62565029444));
#24084=CARTESIAN_POINT('Ctrl Pts',(-0.3624746317386,-1.489220971666,-26.68415029444));
#24085=CARTESIAN_POINT('Ctrl Pts',(-1.267567021527,-0.8611904888719,-26.74265029444));
#24086=CARTESIAN_POINT('Ctrl Pts',(-1.434621292425,-0.1469553746322,-26.78165029444));
#24087=CARTESIAN_POINT('Ctrl Pts',(-1.387327460022,0.193001210377,-26.80115029444));
#24088=CARTESIAN_POINT('Ctrl Pts',(0.2216315720351,1.246753099329,-25.00673967864));
#24089=CARTESIAN_POINT('Ctrl Pts',(0.527141221495,1.192443562085,-25.02623967864));
#24090=CARTESIAN_POINT('Ctrl Pts',(1.094576294964,0.8492743025702,-25.06523967864));
#24091=CARTESIAN_POINT('Ctrl Pts',(1.381707433535,-0.1043828697565,-25.12373967864));
#24092=CARTESIAN_POINT('Ctrl Pts',(0.9548035033152,-1.004060497225,-25.18223967864));
#24093=CARTESIAN_POINT('Ctrl Pts',(0.0348244334854,-1.385141525401,-25.24073967864));
#24094=CARTESIAN_POINT('Ctrl Pts',(-0.9031679079763,-1.050769563483,-25.29923967864));
#24095=CARTESIAN_POINT('Ctrl Pts',(-1.37465222959,-0.1736590647829,-25.35773967864));
#24096=CARTESIAN_POINT('Ctrl Pts',(-1.136107913383,0.793149528647,-25.41623967864));
#24097=CARTESIAN_POINT('Ctrl Pts',(-0.3107446679484,1.350283251132,-25.47473967864));
#24098=CARTESIAN_POINT('Ctrl Pts',(0.6751231782377,1.209973479856,-25.53323967864));
#24099=CARTESIAN_POINT('Ctrl Pts',(1.312278829779,0.4446924903434,-25.59173967864));
#24100=CARTESIAN_POINT('Ctrl Pts',(1.27162086324,-0.5502794859312,-25.65023967864));
#24101=CARTESIAN_POINT('Ctrl Pts',(0.5741497994896,-1.261023053592,-25.70873967864));
#24102=CARTESIAN_POINT('Ctrl Pts',(-0.4198790837452,-1.320427464418,-25.76723967864));
#24103=CARTESIAN_POINT('Ctrl Pts',(-1.197033511132,-0.6978093629019,-25.82573967864));
#24104=CARTESIAN_POINT('Ctrl Pts',(-1.355900433453,0.2852387566824,-25.88423967864));
#24105=CARTESIAN_POINT('Ctrl Pts',(-0.8144224711886,1.120956364969,-25.94273967864));
#24106=CARTESIAN_POINT('Ctrl Pts',(0.1477180983746,1.377681565952,-26.00123967864));
#24107=CARTESIAN_POINT('Ctrl Pts',(1.033559839496,0.9228115690148,-26.05973967864));
#24108=CARTESIAN_POINT('Ctrl Pts',(1.38555091679,-0.008705787692769,-26.11823967864));
#24109=CARTESIAN_POINT('Ctrl Pts',(1.021882146958,-0.9357264619928,-26.17673967864));
#24110=CARTESIAN_POINT('Ctrl Pts',(0.1303944337356,-1.37942902105,-26.23523967864));
#24111=CARTESIAN_POINT('Ctrl Pts',(-0.8284441504486,-1.11063379547,-26.29373967864));
#24112=CARTESIAN_POINT('Ctrl Pts',(-1.359377697933,-0.2681779299465,-26.35223967864));
#24113=CARTESIAN_POINT('Ctrl Pts',(-1.188170301526,0.712796213176,-26.41073967864));
#24114=CARTESIAN_POINT('Ctrl Pts',(-0.403253374937,1.32559951767,-26.46923967864));
#24115=CARTESIAN_POINT('Ctrl Pts',(0.5899504854742,1.253708358346,-26.52773967864));
#24116=CARTESIAN_POINT('Ctrl Pts',(1.278435472814,0.5342580719014,-26.58623967864));
#24117=CARTESIAN_POINT('Ctrl Pts',(1.306586531957,-0.461152275356,-26.64473967864));
#24118=CARTESIAN_POINT('Ctrl Pts',(0.6598677698274,-1.218343850632,-26.70323967864));
#24119=CARTESIAN_POINT('Ctrl Pts',(-0.3276970697449,-1.346337938953,-26.76173967864));
#24120=CARTESIAN_POINT('Ctrl Pts',(-1.145950536365,-0.7785637255274,-26.82023967864));
#24121=CARTESIAN_POINT('Ctrl Pts',(-1.296976815913,-0.1328557681934,-26.85923967864));
#24122=CARTESIAN_POINT('Ctrl Pts',(-1.254220581577,0.1744837446815,-26.87873967864));
#24123=CARTESIAN_POINT('Ctrl Pts',(0.1981104409423,1.114438723627,-25.08432906285));
#24124=CARTESIAN_POINT('Ctrl Pts',(0.47119721649,1.065892903769,-25.10382906285));
#24125=CARTESIAN_POINT('Ctrl Pts',(0.9784120125535,0.7591432259322,-25.14282906285));
#24126=CARTESIAN_POINT('Ctrl Pts',(1.235070736526,-0.09330501139523,-25.20132906285));
#24127=CARTESIAN_POINT('Ctrl Pts',(0.8534729114545,-0.8975024000936,-25.25982906285));
#24128=CARTESIAN_POINT('Ctrl Pts',(0.03112861498029,-1.238140377948,-25.31832906285));
#24129=CARTESIAN_POINT('Ctrl Pts',(-0.80731725562,-0.9392543654266,-25.37682906285));
#24130=CARTESIAN_POINT('Ctrl Pts',(-1.228764281396,-0.1552291200295,-25.43532906285));
#24131=CARTESIAN_POINT('Ctrl Pts',(-1.015535997925,0.7089748153235,-25.49382906285));
#24132=CARTESIAN_POINT('Ctrl Pts',(-0.2777662163492,1.206981513611,-25.55232906285));
#24133=CARTESIAN_POINT('Ctrl Pts',(0.6034742672396,1.081562421011,-25.61082906285));
#24134=CARTESIAN_POINT('Ctrl Pts',(1.173010393869,0.3974985356856,-25.66932906285));
#24135=CARTESIAN_POINT('Ctrl Pts',(1.136667342178,-0.4918798824477,-25.72782906285));
#24136=CARTESIAN_POINT('Ctrl Pts',(0.5132169072275,-1.127194248056,-25.78632906285));
#24137=CARTESIAN_POINT('Ctrl Pts',(-0.3753185056597,-1.180294236991,-25.84482906285));
#24138=CARTESIAN_POINT('Ctrl Pts',(-1.069995734522,-0.6237528313713,-25.90332906285));
#24139=CARTESIAN_POINT('Ctrl Pts',(-1.212002560279,0.2549671752147,-25.96182906285));
#24140=CARTESIAN_POINT('Ctrl Pts',(-0.7279901207168,1.001992440436,-26.02032906285));
#24141=CARTESIAN_POINT('Ctrl Pts',(0.1320411949229,1.231472122869,-26.07882906285));
#24142=CARTESIAN_POINT('Ctrl Pts',(0.9238710607092,0.8248761905421,-26.13732906285));
#24143=CARTESIAN_POINT('Ctrl Pts',(1.238506321788,-0.007781867099204,-26.19582906285));
#24144=CARTESIAN_POINT('Ctrl Pts',(0.9134326886102,-0.8364204625026,-26.25432906285));
#24145=CARTESIAN_POINT('Ctrl Pts',(0.1165560417524,-1.233034125506,-26.31282906285));
#24146=CARTESIAN_POINT('Ctrl Pts',(-0.7405237188655,-0.992765376005,-26.37132906285));
#24147=CARTESIAN_POINT('Ctrl Pts',(-1.215110792527,-0.2397169657051,-26.42982906285));
#24148=CARTESIAN_POINT('Ctrl Pts',(-1.062073152252,0.6371491696676,-26.48832906285));
#24149=CARTESIAN_POINT('Ctrl Pts',(-0.3604572362442,1.184917394878,-26.54682906285));
#24150=CARTESIAN_POINT('Ctrl Pts',(0.5273407111551,1.120655840702,-26.60532906285));
#24151=CARTESIAN_POINT('Ctrl Pts',(1.142758736536,0.4775587757172,-26.66382906285));
#24152=CARTESIAN_POINT('Ctrl Pts',(1.167922203495,-0.412211490328,-26.72232906285));
#24153=CARTESIAN_POINT('Ctrl Pts',(0.5898378721215,-1.089044468041,-26.78082906285));
#24154=CARTESIAN_POINT('Ctrl Pts',(-0.2929195077513,-1.20345490624,-26.83932906285));
#24155=CARTESIAN_POINT('Ctrl Pts',(-1.024334051204,-0.6959369621828,-26.89782906285));
#24156=CARTESIAN_POINT('Ctrl Pts',(-1.1593323394,-0.1187561617546,-26.93682906285));
#24157=CARTESIAN_POINT('Ctrl Pts',(-1.121113703131,0.1559662789859,-26.95632906285));
#24158=CARTESIAN_POINT('',(-1.426584774443,-0.4635254915624,-26.7078125));
#24159=CARTESIAN_POINT('Ctrl Pts',(-1.105729660272,-1.064811084801,-26.65156091023));
#24160=CARTESIAN_POINT('Ctrl Pts',(-1.366655469426,-0.7938584149506,-26.67106091023));
#24161=CARTESIAN_POINT('Ctrl Pts',(-1.678634926928,-0.05297738133179,-26.71006091023));
#24162=CARTESIAN_POINT('Ctrl Pts',(-1.280710439764,1.086900895213,-26.76856091023));
#24163=CARTESIAN_POINT('Ctrl Pts',(-0.2209700935106,1.665057301661,-26.82706091023));
#24164=CARTESIAN_POINT('Ctrl Pts',(0.9528224555883,1.383269870276,-26.88556091023));
#24165=CARTESIAN_POINT('Ctrl Pts',(1.634488630304,0.386977838339,-26.94406091023));
#24166=CARTESIAN_POINT('Ctrl Pts',(1.47190861048,-0.809188464797,-27.00256091023));
#24167=CARTESIAN_POINT('Ctrl Pts',(0.549065160654,-1.5873972589,-27.06106091023));
#24168=CARTESIAN_POINT('Ctrl Pts',(-0.657379904454,-1.545688807378,-27.11956091023));
#24169=CARTESIAN_POINT('Ctrl Pts',(-1.524277318107,-0.7056067715846,-27.17806091023));
#24170=CARTESIAN_POINT('Ctrl Pts',(-1.603860446231,0.4989328038561,-27.23656091023));
#24171=CARTESIAN_POINT('Ctrl Pts',(-0.8550232549381,1.44576536791,-27.29506091023));
#24172=CARTESIAN_POINT('Ctrl Pts',(0.3354475143376,1.645836332335,-27.35356091023));
#24173=CARTESIAN_POINT('Ctrl Pts',(1.352654123417,0.9958057490488,-27.41206091023));
#24174=CARTESIAN_POINT('Ctrl Pts',(1.671192620316,-0.1685748889662,-27.47056091023));
#24175=CARTESIAN_POINT('Ctrl Pts',(1.126532630187,-1.245883823055,-27.52906091023));
#24176=CARTESIAN_POINT('Ctrl Pts',(0.,-1.6796732621,-27.58756091023));
#24177=CARTESIAN_POINT('Ctrl Pts',(-1.126532630187,-1.245883823055,-27.64606091023));
#24178=CARTESIAN_POINT('Ctrl Pts',(-1.671192620316,-0.1685748889661,-27.70456091023));
#24179=CARTESIAN_POINT('Ctrl Pts',(-1.352654123417,0.9958057490488,-27.76306091023));
#24180=CARTESIAN_POINT('Ctrl Pts',(-0.3354475143376,1.645836332335,-27.82156091023));
#24181=CARTESIAN_POINT('Ctrl Pts',(0.8550232549381,1.44576536791,-27.88006091023));
#24182=CARTESIAN_POINT('Ctrl Pts',(1.603860446231,0.4989328038561,-27.93856091023));
#24183=CARTESIAN_POINT('Ctrl Pts',(1.524277318107,-0.7056067715846,-27.99706091023));
#24184=CARTESIAN_POINT('Ctrl Pts',(0.657379904454,-1.545688807378,-28.05556091023));
#24185=CARTESIAN_POINT('Ctrl Pts',(-0.549065160654,-1.5873972589,-28.11406091023));
#24186=CARTESIAN_POINT('Ctrl Pts',(-1.47190861048,-0.809188464797,-28.17256091023));
#24187=CARTESIAN_POINT('Ctrl Pts',(-1.634488630304,0.3869778383391,-28.23106091023));
#24188=CARTESIAN_POINT('Ctrl Pts',(-0.9528224555883,1.383269870276,-28.28956091023));
#24189=CARTESIAN_POINT('Ctrl Pts',(0.2209700935106,1.665057301661,-28.34806091023));
#24190=CARTESIAN_POINT('Ctrl Pts',(1.280710439764,1.086900895213,-28.40656091023));
#24191=CARTESIAN_POINT('Ctrl Pts',(1.678634926928,-0.05297738133181,-28.46506091023));
#24192=CARTESIAN_POINT('Ctrl Pts',(1.366655469426,-0.7938584149506,-28.50406091023));
#24193=CARTESIAN_POINT('Ctrl Pts',(1.105729660272,-1.064811084801,-28.52356091023));
#24194=CARTESIAN_POINT('Ctrl Pts',(-1.008928226787,-0.9715918802313,-26.72915029444));
#24195=CARTESIAN_POINT('Ctrl Pts',(-1.247011208018,-0.7243598428201,-26.74865029444));
#24196=CARTESIAN_POINT('Ctrl Pts',(-1.531678330698,-0.0483394606542,-26.78765029444));
#24197=CARTESIAN_POINT('Ctrl Pts',(-1.168590261656,0.9917478315913,-26.84615029444));
#24198=CARTESIAN_POINT('Ctrl Pts',(-0.2016252006515,1.519289362691,-26.90465029444));
#24199=CARTESIAN_POINT('Ctrl Pts',(0.8694073290239,1.262171096181,-26.96315029444));
#24200=CARTESIAN_POINT('Ctrl Pts',(1.491396834802,0.3530997478581,-27.02165029444));
#24201=CARTESIAN_POINT('Ctrl Pts',(1.34304993139,-0.7383478188722,-27.08015029444));
#24202=CARTESIAN_POINT('Ctrl Pts',(0.5009970871116,-1.448428091577,-27.13865029444));
#24203=CARTESIAN_POINT('Ctrl Pts',(-0.5998293843028,-1.410371018906,-27.19715029444));
#24204=CARTESIAN_POINT('Ctrl Pts',(-1.390834004861,-0.6438342159409,-27.25565029444));
#24205=CARTESIAN_POINT('Ctrl Pts',(-1.463450004255,0.4552535824685,-27.31415029444));
#24206=CARTESIAN_POINT('Ctrl Pts',(-0.7801699886157,1.319195406802,-27.37265029444));
#24207=CARTESIAN_POINT('Ctrl Pts',(0.3060806614679,1.501751098868,-27.43115029444));
#24208=CARTESIAN_POINT('Ctrl Pts',(1.234235614028,0.9086276372156,-27.48965029444));
#24209=CARTESIAN_POINT('Ctrl Pts',(1.524887563041,-0.1538169499438,-27.54815029444));
#24210=CARTESIAN_POINT('Ctrl Pts',(1.027909994485,-1.136812551513,-27.60665029444));
#24211=CARTESIAN_POINT('Ctrl Pts',(0.,-1.532625764506,-27.66515029444));
#24212=CARTESIAN_POINT('Ctrl Pts',(-1.027909994485,-1.136812551513,-27.72365029444));
#24213=CARTESIAN_POINT('Ctrl Pts',(-1.524887563041,-0.1538169499438,-27.78215029444));
#24214=CARTESIAN_POINT('Ctrl Pts',(-1.234235614028,0.9086276372156,-27.84065029444));
#24215=CARTESIAN_POINT('Ctrl Pts',(-0.3060806614679,1.501751098868,-27.89915029444));
#24216=CARTESIAN_POINT('Ctrl Pts',(0.7801699886157,1.319195406802,-27.95765029444));
#24217=CARTESIAN_POINT('Ctrl Pts',(1.463450004255,0.4552535824684,-28.01615029444));
#24218=CARTESIAN_POINT('Ctrl Pts',(1.390834004861,-0.6438342159409,-28.07465029444));
#24219=CARTESIAN_POINT('Ctrl Pts',(0.5998293843027,-1.410371018906,-28.13315029444));
#24220=CARTESIAN_POINT('Ctrl Pts',(-0.5009970871116,-1.448428091577,-28.19165029444));
#24221=CARTESIAN_POINT('Ctrl Pts',(-1.34304993139,-0.7383478188722,-28.25015029444));
#24222=CARTESIAN_POINT('Ctrl Pts',(-1.491396834802,0.3530997478581,-28.30865029444));
#24223=CARTESIAN_POINT('Ctrl Pts',(-0.8694073290239,1.262171096181,-28.36715029444));
#24224=CARTESIAN_POINT('Ctrl Pts',(0.2016252006515,1.519289362691,-28.42565029444));
#24225=CARTESIAN_POINT('Ctrl Pts',(1.168590261656,0.9917478315913,-28.48415029444));
#24226=CARTESIAN_POINT('Ctrl Pts',(1.531678330698,-0.04833946065422,-28.54265029444));
#24227=CARTESIAN_POINT('Ctrl Pts',(1.247011208018,-0.7243598428201,-28.58165029444));
#24228=CARTESIAN_POINT('Ctrl Pts',(1.008928226787,-0.9715918802313,-28.60115029444));
#24229=CARTESIAN_POINT('Ctrl Pts',(-0.9121267933018,-0.8783726756619,-26.80673967864));
#24230=CARTESIAN_POINT('Ctrl Pts',(-1.12736694661,-0.6548612706895,-26.82623967864));
#24231=CARTESIAN_POINT('Ctrl Pts',(-1.384721734467,-0.04370153997662,-26.86523967864));
#24232=CARTESIAN_POINT('Ctrl Pts',(-1.056470083549,0.8965947679692,-26.92373967864));
#24233=CARTESIAN_POINT('Ctrl Pts',(-0.1822803077923,1.373521423722,-26.98223967864));
#24234=CARTESIAN_POINT('Ctrl Pts',(0.7859922024595,1.141072322086,-27.04073967864));
#24235=CARTESIAN_POINT('Ctrl Pts',(1.3483050393,0.3192216573772,-27.09923967864));
#24236=CARTESIAN_POINT('Ctrl Pts',(1.2141912523,-0.6675071729475,-27.15773967864));
#24237=CARTESIAN_POINT('Ctrl Pts',(0.4529290135692,-1.309458924255,-27.21623967864));
#24238=CARTESIAN_POINT('Ctrl Pts',(-0.5422788641515,-1.275053230434,-27.27473967864));
#24239=CARTESIAN_POINT('Ctrl Pts',(-1.257390691615,-0.5820616602972,-27.33323967864));
#24240=CARTESIAN_POINT('Ctrl Pts',(-1.323039562278,0.4115743610808,-27.39173967864));
#24241=CARTESIAN_POINT('Ctrl Pts',(-0.7053167222932,1.192625445694,-27.45023967864));
#24242=CARTESIAN_POINT('Ctrl Pts',(0.2767138085983,1.357665865401,-27.50873967864));
#24243=CARTESIAN_POINT('Ctrl Pts',(1.11581710464,0.8214495253824,-27.56723967864));
#24244=CARTESIAN_POINT('Ctrl Pts',(1.378582505767,-0.1390590109215,-27.62573967864));
#24245=CARTESIAN_POINT('Ctrl Pts',(0.9292873587837,-1.027741279971,-27.68423967864));
#24246=CARTESIAN_POINT('Ctrl Pts',(0.,-1.385578266913,-27.74273967864));
#24247=CARTESIAN_POINT('Ctrl Pts',(-0.9292873587837,-1.027741279971,-27.80123967864));
#24248=CARTESIAN_POINT('Ctrl Pts',(-1.378582505767,-0.1390590109214,-27.85973967864));
#24249=CARTESIAN_POINT('Ctrl Pts',(-1.11581710464,0.8214495253824,-27.91823967864));
#24250=CARTESIAN_POINT('Ctrl Pts',(-0.2767138085983,1.357665865401,-27.97673967864));
#24251=CARTESIAN_POINT('Ctrl Pts',(0.7053167222932,1.192625445694,-28.03523967864));
#24252=CARTESIAN_POINT('Ctrl Pts',(1.323039562278,0.4115743610808,-28.09373967864));
#24253=CARTESIAN_POINT('Ctrl Pts',(1.257390691615,-0.5820616602972,-28.15223967864));
#24254=CARTESIAN_POINT('Ctrl Pts',(0.5422788641515,-1.275053230434,-28.21073967864));
#24255=CARTESIAN_POINT('Ctrl Pts',(-0.4529290135692,-1.309458924255,-28.26923967864));
#24256=CARTESIAN_POINT('Ctrl Pts',(-1.2141912523,-0.6675071729475,-28.32773967864));
#24257=CARTESIAN_POINT('Ctrl Pts',(-1.3483050393,0.3192216573772,-28.38623967864));
#24258=CARTESIAN_POINT('Ctrl Pts',(-0.7859922024595,1.141072322086,-28.44473967864));
#24259=CARTESIAN_POINT('Ctrl Pts',(0.1822803077923,1.373521423722,-28.50323967864));
#24260=CARTESIAN_POINT('Ctrl Pts',(1.056470083549,0.8965947679692,-28.56173967864));
#24261=CARTESIAN_POINT('Ctrl Pts',(1.384721734467,-0.04370153997664,-28.62023967864));
#24262=CARTESIAN_POINT('Ctrl Pts',(1.12736694661,-0.6548612706895,-28.65923967864));
#24263=CARTESIAN_POINT('Ctrl Pts',(0.9121267933018,-0.8783726756619,-28.67873967864));
#24264=CARTESIAN_POINT('Ctrl Pts',(-0.8153253598169,-0.7851534710925,-26.88432906285));
#24265=CARTESIAN_POINT('Ctrl Pts',(-1.007722685201,-0.585362698559,-26.90382906285));
#24266=CARTESIAN_POINT('Ctrl Pts',(-1.237765138237,-0.03906361929903,-26.94282906285));
#24267=CARTESIAN_POINT('Ctrl Pts',(-0.9443499054416,0.8014417043471,-27.00132906285));
#24268=CARTESIAN_POINT('Ctrl Pts',(-0.1629354149332,1.227753484752,-27.05982906285));
#24269=CARTESIAN_POINT('Ctrl Pts',(0.7025770758952,1.019973547991,-27.11832906285));
#24270=CARTESIAN_POINT('Ctrl Pts',(1.205213243798,0.2853435668963,-27.17682906285));
#24271=CARTESIAN_POINT('Ctrl Pts',(1.08533257321,-0.5966665270227,-27.23532906285));
#24272=CARTESIAN_POINT('Ctrl Pts',(0.4048609400268,-1.170489756933,-27.29382906285));
#24273=CARTESIAN_POINT('Ctrl Pts',(-0.4847283440002,-1.139735441963,-27.35232906285));
#24274=CARTESIAN_POINT('Ctrl Pts',(-1.123947378369,-0.5202891046535,-27.41082906285));
#24275=CARTESIAN_POINT('Ctrl Pts',(-1.182629120302,0.3678951396931,-27.46932906285));
#24276=CARTESIAN_POINT('Ctrl Pts',(-0.6304634559708,1.066055484586,-27.52782906285));
#24277=CARTESIAN_POINT('Ctrl Pts',(0.2473469557286,1.213580631934,-27.58632906285));
#24278=CARTESIAN_POINT('Ctrl Pts',(0.9973985952512,0.7342714135492,-27.64482906285));
#24279=CARTESIAN_POINT('Ctrl Pts',(1.232277448493,-0.1243010718991,-27.70332906285));
#24280=CARTESIAN_POINT('Ctrl Pts',(0.8306647230819,-0.9186700084293,-27.76182906285));
#24281=CARTESIAN_POINT('Ctrl Pts',(0.,-1.23853076932,-27.82032906285));
#24282=CARTESIAN_POINT('Ctrl Pts',(-0.8306647230819,-0.9186700084293,-27.87882906285));
#24283=CARTESIAN_POINT('Ctrl Pts',(-1.232277448493,-0.1243010718991,-27.93732906285));
#24284=CARTESIAN_POINT('Ctrl Pts',(-0.9973985952511,0.7342714135493,-27.99582906285));
#24285=CARTESIAN_POINT('Ctrl Pts',(-0.2473469557286,1.213580631934,-28.05432906285));
#24286=CARTESIAN_POINT('Ctrl Pts',(0.6304634559708,1.066055484586,-28.11282906285));
#24287=CARTESIAN_POINT('Ctrl Pts',(1.182629120302,0.3678951396931,-28.17132906285));
#24288=CARTESIAN_POINT('Ctrl Pts',(1.123947378369,-0.5202891046535,-28.22982906285));
#24289=CARTESIAN_POINT('Ctrl Pts',(0.4847283440002,-1.139735441963,-28.28832906285));
#24290=CARTESIAN_POINT('Ctrl Pts',(-0.4048609400269,-1.170489756933,-28.34682906285));
#24291=CARTESIAN_POINT('Ctrl Pts',(-1.08533257321,-0.5966665270227,-28.40532906285));
#24292=CARTESIAN_POINT('Ctrl Pts',(-1.205213243798,0.2853435668963,-28.46382906285));
#24293=CARTESIAN_POINT('Ctrl Pts',(-0.7025770758952,1.019973547991,-28.52232906285));
#24294=CARTESIAN_POINT('Ctrl Pts',(0.1629354149332,1.227753484752,-28.58082906285));
#24295=CARTESIAN_POINT('Ctrl Pts',(0.9443499054416,0.8014417043471,-28.63932906285));
#24296=CARTESIAN_POINT('Ctrl Pts',(1.237765138237,-0.03906361929905,-28.69782906285));
#24297=CARTESIAN_POINT('Ctrl Pts',(1.007722685201,-0.585362698559,-28.73682906285));
#24298=CARTESIAN_POINT('Ctrl Pts',(0.8153253598169,-0.7851534710925,-28.75632906285));
#24299=CARTESIAN_POINT('',(1.42616365839207,-0.463388665150997,-28.5080680843046));
#24300=CARTESIAN_POINT('',(1.426584774443,-0.4635254915624,-28.5078125));
#24301=CARTESIAN_POINT('Ctrl Pts',(1.42592296431875,-0.463335877700853,
-28.5076220976351));
#24302=CARTESIAN_POINT('Ctrl Pts',(1.4516646730899,-0.383939856993698,-28.503323569032));
#24303=CARTESIAN_POINT('Ctrl Pts',(1.47080306466018,-0.302401817242002,
-28.4990861959195));
#24304=CARTESIAN_POINT('Ctrl Pts',(1.49271878036586,-0.154988761660788,
-28.4913957131492));
#24305=CARTESIAN_POINT('Ctrl Pts',(1.49813264451624,-0.0894476287888264,
-28.4879643848815));
#24306=CARTESIAN_POINT('Ctrl Pts',(1.5006482312565,0.0698946699337639,-28.4793972302415));
#24307=CARTESIAN_POINT('Ctrl Pts',(1.49328387783098,0.163646013371891,-28.4741909039621));
#24308=CARTESIAN_POINT('Ctrl Pts',(1.46690763178642,0.315977876498846,-28.4656689062437));
#24309=CARTESIAN_POINT('Ctrl Pts',(1.45284440993149,0.375451041534454,-28.4623263523921));
#24310=CARTESIAN_POINT('Ctrl Pts',(1.40056433535711,0.548273795567868,-28.4526654076531));
#24311=CARTESIAN_POINT('Ctrl Pts',(1.35213073740469,0.658369858497446,-28.4466068811747));
#24312=CARTESIAN_POINT('Ctrl Pts',(1.25646955925034,0.820805928945592,-28.436976157127));
#24313=CARTESIAN_POINT('Ctrl Pts',(1.21727123019692,0.878004524876435,-28.4334250716445));
#24314=CARTESIAN_POINT('Ctrl Pts',(1.10251991809743,1.02275181198366,-28.4237016458728));
#24315=CARTESIAN_POINT('Ctrl Pts',(1.02042512302908,1.10451558663737,-28.4173189735821));
#24316=CARTESIAN_POINT('Ctrl Pts',(0.881164643456005,1.21473017110051,-28.4075323182098));
#24317=CARTESIAN_POINT('Ctrl Pts',(0.829533462102437,1.25058483394728,-28.4040917352513));
#24318=CARTESIAN_POINT('Ctrl Pts',(0.675514033222316,1.34367687607065,-28.3944542505251));
#24319=CARTESIAN_POINT('Ctrl Pts',(0.568131647479671,1.39230007563897,-28.3884997720049));
#24320=CARTESIAN_POINT('Ctrl Pts',(0.389136578471147,1.44958560114917,-28.37889107636));
#24321=CARTESIAN_POINT('Ctrl Pts',(0.320018924005801,1.46645692540373,-28.3752483096082));
#24322=CARTESIAN_POINT('Ctrl Pts',(0.134162099992888,1.4980066036685,-28.3653254266851));
#24323=CARTESIAN_POINT('Ctrl Pts',(0.0164281179871881,1.50378688439387,
-28.3588302237474));
#24324=CARTESIAN_POINT('Ctrl Pts',(-0.162337185079902,1.49183709314879,
-28.3489565986272));
#24325=CARTESIAN_POINT('Ctrl Pts',(-0.224273388847288,1.48381261253025,
-28.3455389282578));
#24326=CARTESIAN_POINT('Ctrl Pts',(-0.401194807636539,1.44946528421081,
-28.335889754369));
#24327=CARTESIAN_POINT('Ctrl Pts',(-0.514067816300854,1.41320064504075,
-28.3299056019057));
#24328=CARTESIAN_POINT('Ctrl Pts',(-0.685303550305146,1.33529407650487,
-28.3202890842721));
#24329=CARTESIAN_POINT('Ctrl Pts',(-0.74742371702866,1.30161270724248,-28.3166707000832));
#24330=CARTESIAN_POINT('Ctrl Pts',(-0.905674963820369,1.20070679515175,
-28.306791048473));
#24331=CARTESIAN_POINT('Ctrl Pts',(-0.99658655727132,1.12622597733011,-28.3003149224196));
#24332=CARTESIAN_POINT('Ctrl Pts',(-1.12095380474306,0.997698499287579,
-28.2904587338548));
#24333=CARTESIAN_POINT('Ctrl Pts',(-1.16153071863231,0.950185721820537,
-28.2870394568104));
#24334=CARTESIAN_POINT('Ctrl Pts',(-1.2696777687758,0.806104733354828,-28.277393898246));
#24335=CARTESIAN_POINT('Ctrl Pts',(-1.32903537158566,0.703594749870364,
-28.2714142267783));
#24336=CARTESIAN_POINT('Ctrl Pts',(-1.40381150836108,0.53101108089913,-28.2617995366514));
#24337=CARTESIAN_POINT('Ctrl Pts',(-1.42732663669233,0.464310956122346,
-28.2581781571965));
#24338=CARTESIAN_POINT('Ctrl Pts',(-1.47705738103529,0.283275185944521,
-28.2482956416959));
#24339=CARTESIAN_POINT('Ctrl Pts',(-1.49454352171617,0.167060440209565,
-28.2418198776906));
#24340=CARTESIAN_POINT('Ctrl Pts',(-1.50060179387312,-0.0116989017369946,
-28.2319629537923));
#24341=CARTESIAN_POINT('Ctrl Pts',(-1.49883556041021,-0.0741723425411832,
-28.2285427453193));
#24342=CARTESIAN_POINT('Ctrl Pts',(-1.48242439855621,-0.253579384345749,
-28.2188969692646));
#24343=CARTESIAN_POINT('Ctrl Pts',(-1.45770808385869,-0.369412498303161,
-28.2129179176856));
#24344=CARTESIAN_POINT('Ctrl Pts',(-1.39743345394519,-0.547577876420512,
-28.2033032573019));
#24345=CARTESIAN_POINT('Ctrl Pts',(-1.37013861575826,-0.612836186582772,
-28.1996812284657));
#24346=CARTESIAN_POINT('Ctrl Pts',(-1.28559069101167,-0.780517974958821,
-28.1897961151518));
#24347=CARTESIAN_POINT('Ctrl Pts',(-1.22059622835544,-0.878477224158937,
-28.1833182398528));
#24348=CARTESIAN_POINT('Ctrl Pts',(-1.10517739974363,-1.01514695362663,
-28.1734599981016));
#24349=CARTESIAN_POINT('Ctrl Pts',(-1.06197439538667,-1.06029133708738,
-28.1700404840139));
#24350=CARTESIAN_POINT('Ctrl Pts',(-0.929492016747349,-1.18233895555091,
-28.1603961172978));
#24351=CARTESIAN_POINT('Ctrl Pts',(-0.833481330188796,-1.25167244016774,
-28.1544177203215));
#24352=CARTESIAN_POINT('Ctrl Pts',(-0.669291333748551,-1.34339519624346,
-28.1448037300712));
#24353=CARTESIAN_POINT('Ctrl Pts',(-0.605277730231828,-1.37349435639921,
-28.1411817119154));
#24354=CARTESIAN_POINT('Ctrl Pts',(-0.430071077583583,-1.44117968319116,
-28.1312948271126));
#24355=CARTESIAN_POINT('Ctrl Pts',(-0.316127250170529,-1.47025476212026,
-28.1248149638959));
#24356=CARTESIAN_POINT('Ctrl Pts',(-0.13883142420414,-1.49421045876829,
-28.1149556143986));
#24357=CARTESIAN_POINT('Ctrl Pts',(-0.0765212037758559,-1.49871626806615,
-28.1115368660599));
#24358=CARTESIAN_POINT('Ctrl Pts',(0.103476408041793,-1.5003822934613,-28.1018993613209));
#24359=CARTESIAN_POINT('Ctrl Pts',(0.22107994522376,-1.48743842556337,-28.0959263852764));
#24360=CARTESIAN_POINT('Ctrl Pts',(0.404325714405427,-1.44540238901112,
-28.0863159307243));
#24361=CARTESIAN_POINT('Ctrl Pts',(0.472039677844878,-1.4247919824078,-28.0826917867747));
#24362=CARTESIAN_POINT('Ctrl Pts',(0.647640177920739,-1.35741391816062,
-28.0727916994037));
#24363=CARTESIAN_POINT('Ctrl Pts',(0.751841587366556,-1.30244714266978,
-28.0662996627543));
#24364=CARTESIAN_POINT('Ctrl Pts',(0.899497233796535,-1.20118067772247,
-28.056432960265));
#24365=CARTESIAN_POINT('Ctrl Pts',(0.948670279861992,-1.16276469467675,
-28.0530184176353));
#24366=CARTESIAN_POINT('Ctrl Pts',(1.08284208874631,-1.04364124354584,-28.0434127722028));
#24367=CARTESIAN_POINT('Ctrl Pts',(1.16107831074709,-0.955578476827092,
-28.037464424286));
#24368=CARTESIAN_POINT('Ctrl Pts',(1.26875583948425,-0.801842443670456,
-28.0278703050064));
#24369=CARTESIAN_POINT('Ctrl Pts',(1.30529835608295,-0.740996048005445,
-28.0242368253798));
#24370=CARTESIAN_POINT('Ctrl Pts',(1.39096959843416,-0.57223109919015,-28.0142761029451));
#24371=CARTESIAN_POINT('Ctrl Pts',(1.43167640473481,-0.460613253287086,
-28.0077276139323));
#24372=CARTESIAN_POINT('Ctrl Pts',(1.47316553590904,-0.285785232077346,
-27.9978269398273));
#24373=CARTESIAN_POINT('Ctrl Pts',(1.48374413368801,-0.224631418430332,
-27.9944319379755));
#24374=CARTESIAN_POINT('Ctrl Pts',(1.50292114375066,-0.0489988829097152,
-27.984976375275));
#24375=CARTESIAN_POINT('Ctrl Pts',(1.50209457818614,0.0663516175829957,
-27.9791444841177));
#24376=CARTESIAN_POINT('Ctrl Pts',(1.47976056185988,0.251244628382758,-27.9696267163725));
#24377=CARTESIAN_POINT('Ctrl Pts',(1.46608945011532,0.321842819328718,-27.965948568838));
#24378=CARTESIAN_POINT('Ctrl Pts',(1.42554988683578,0.47224606533571,-27.9577565207606));
#24379=CARTESIAN_POINT('Ctrl Pts',(1.396869339743,0.551196312457827,-27.9531910439495));
#24380=CARTESIAN_POINT('Ctrl Pts',(1.32828966134185,0.700068795939468,-27.9441614169721));
#24381=CARTESIAN_POINT('Ctrl Pts',(1.28886638514574,0.770287049061794,-27.9397080725723));
#24382=CARTESIAN_POINT('Ctrl Pts',(1.20105115222611,0.900844271197268,-27.9311879209186));
#24383=CARTESIAN_POINT('Ctrl Pts',(1.15323605214701,0.961173009596781,-27.927159390159));
#24384=CARTESIAN_POINT('Ctrl Pts',(1.03113117407888,1.09313678043491,-27.9178923624111));
#24385=CARTESIAN_POINT('Ctrl Pts',(0.953425800183683,1.16155713534289,-27.9126923047804));
#24386=CARTESIAN_POINT('Ctrl Pts',(0.806967245432844,1.26598668165696,-27.9033645286779));
#24387=CARTESIAN_POINT('Ctrl Pts',(0.741210820501912,1.30561869878126,-27.8992943166603));
#24388=CARTESIAN_POINT('Ctrl Pts',(0.583394542925378,1.38477568346781,-27.8896647037835));
#24389=CARTESIAN_POINT('Ctrl Pts',(0.489886871548345,1.42055251867229,-27.8841013444146));
#24390=CARTESIAN_POINT('Ctrl Pts',(0.31938036937766,1.46698849926037,-27.8744730836011));
#24391=CARTESIAN_POINT('Ctrl Pts',(0.243795335422544,1.48137909149889,-27.8704031474391));
#24392=CARTESIAN_POINT('Ctrl Pts',(0.0683128605550142,1.50095679663137,
-27.8612572972935));
#24393=CARTESIAN_POINT('Ctrl Pts',(-0.0317413520965657,1.50215917195855,
-27.8562262675331));
#24394=CARTESIAN_POINT('Ctrl Pts',(-0.209504424270073,1.48668492189799,
-27.84703302098));
#24395=CARTESIAN_POINT('Ctrl Pts',(-0.287482309193275,1.47367742627492,
-27.8428971115734));
#24396=CARTESIAN_POINT('Ctrl Pts',(-0.439655506240912,1.43555467259612,
-27.834397355129));
#24397=CARTESIAN_POINT('Ctrl Pts',(-0.513570900963485,1.41077773370975,
-27.8300876827913));
#24398=CARTESIAN_POINT('Ctrl Pts',(-0.668050563795896,1.3453186100834,-27.8208425020254));
#24399=CARTESIAN_POINT('Ctrl Pts',(-0.747822759524413,1.30272527256634,
-27.8159338884917));
#24400=CARTESIAN_POINT('Ctrl Pts',(-0.885124648788246,1.21236367813823,
-27.807317523479));
#24401=CARTESIAN_POINT('Ctrl Pts',(-0.943812698786729,1.16718169249958,
-27.8035396650792));
#24402=CARTESIAN_POINT('Ctrl Pts',(-1.08231919829256,1.04341463201487,-27.7940507301813));
#24403=CARTESIAN_POINT('Ctrl Pts',(-1.1575952931583,0.959492955612986,-27.7883285298767));
#24404=CARTESIAN_POINT('Ctrl Pts',(-1.25989871101654,0.815423160489302,
-27.7788404489654));
#24405=CARTESIAN_POINT('Ctrl Pts',(-1.29377727498199,0.760480307524973,
-27.7752997519017));
#24406=CARTESIAN_POINT('Ctrl Pts',(-1.37807329817412,0.601832309402957,
-27.7653917063489));
#24407=CARTESIAN_POINT('Ctrl Pts',(-1.42053833023185,0.493679521843405,
-27.7590125196674));
#24408=CARTESIAN_POINT('Ctrl Pts',(-1.46840257130333,0.311276579656757,
-27.7491172618014));
#24409=CARTESIAN_POINT('Ctrl Pts',(-1.48170726052789,0.239717958079749,
-27.7454006524031));
#24410=CARTESIAN_POINT('Ctrl Pts',(-1.50268591701451,0.0530482402031576,
-27.7358035549755));
#24411=CARTESIAN_POINT('Ctrl Pts',(-1.50248033205375,-0.0631325833269582,
-27.7299161711196));
#24412=CARTESIAN_POINT('Ctrl Pts',(-1.48106199660676,-0.242436234610995,
-27.7202154298389));
#24413=CARTESIAN_POINT('Ctrl Pts',(-1.4691465541843,-0.306362650752422,
-27.7166470421241));
#24414=CARTESIAN_POINT('Ctrl Pts',(-1.42512121626003,-0.47958137707748,
-27.7067890874004));
#24415=CARTESIAN_POINT('Ctrl Pts',(-1.38450563573437,-0.586910041995524,
-27.700490602839));
#24416=CARTESIAN_POINT('Ctrl Pts',(-1.29855947816122,-0.752865717018401,
-27.6906817952317));
#24417=CARTESIAN_POINT('Ctrl Pts',(-1.26063238477963,-0.814672299671888,
-27.6869780558361));
#24418=CARTESIAN_POINT('Ctrl Pts',(-1.15091158538457,-0.967701024939023,
-27.6773574534304));
#24419=CARTESIAN_POINT('Ctrl Pts',(-1.07238295580389,-1.05432331995669,
-27.6714347471479));
#24420=CARTESIAN_POINT('Ctrl Pts',(-0.935579451561983,-1.1734668006248,
-27.6616882873619));
#24421=CARTESIAN_POINT('Ctrl Pts',(-0.883768673628082,-1.21293683651046,
-27.6581138308857));
#24422=CARTESIAN_POINT('Ctrl Pts',(-0.735058866113722,-1.3117119427223,
-27.6482667621033));
#24423=CARTESIAN_POINT('Ctrl Pts',(-0.633217770969367,-1.36392203649838,
-27.6419858399696));
#24424=CARTESIAN_POINT('Ctrl Pts',(-0.458516968014841,-1.42927184788114,
-27.6321958325746));
#24425=CARTESIAN_POINT('Ctrl Pts',(-0.388991906692596,-1.44967668597002,
-27.6284948692181));
#24426=CARTESIAN_POINT('Ctrl Pts',(-0.204886892472027,-1.48966431845479,
-27.6188691445367));
#24427=CARTESIAN_POINT('Ctrl Pts',(-0.088384316819463,-1.50127550237707,
-27.6129387749736));
#24428=CARTESIAN_POINT('Ctrl Pts',(0.0931773509636978,-1.49788323251699,
-27.603182377091));
#24429=CARTESIAN_POINT('Ctrl Pts',(0.158102115673349,-1.49240393028911,
-27.5996065876513));
#24430=CARTESIAN_POINT('Ctrl Pts',(0.334605703811802,-1.46592065586156,
-27.5897619864405));
#24431=CARTESIAN_POINT('Ctrl Pts',(0.445093451049737,-1.43635788839267,
-27.5834849942358));
#24432=CARTESIAN_POINT('Ctrl Pts',(0.618429402724692,-1.36769837238986,
-27.573699316174));
#24433=CARTESIAN_POINT('Ctrl Pts',(0.68367212242673,-1.33621387385003,-27.5699990873574));
#24434=CARTESIAN_POINT('Ctrl Pts',(0.847075172364305,-1.24239707625671,
-27.5603722090784));
#24435=CARTESIAN_POINT('Ctrl Pts',(0.941310341369421,-1.17285269806391,
-27.5544400135388));
#24436=CARTESIAN_POINT('Ctrl Pts',(1.07373531512154,-1.04853649392191,-27.5446814006941));
#24437=CARTESIAN_POINT('Ctrl Pts',(1.11821899467738,-1.00092565180024,-27.5411054558441));
#24438=CARTESIAN_POINT('Ctrl Pts',(1.23137427531208,-0.86290252007411,-27.5312608956508));
#24439=CARTESIAN_POINT('Ctrl Pts',(1.29349708821054,-0.76687450479305,-27.5249841244415));
#24440=CARTESIAN_POINT('Ctrl Pts',(1.37601842237683,-0.59969000756072,-27.5151982923214));
#24441=CARTESIAN_POINT('Ctrl Pts',(1.40329689371724,-0.532573066997368,
-27.5114977353222));
#24442=CARTESIAN_POINT('Ctrl Pts',(1.46157520466307,-0.353389922872069,
-27.5018707007339));
#24443=CARTESIAN_POINT('Ctrl Pts',(1.4848282527389,-0.238607462222975,-27.4959386516808));
#24444=CARTESIAN_POINT('Ctrl Pts',(1.49967452896699,-0.0575740238518383,
-27.4861796041596));
#24445=CARTESIAN_POINT('Ctrl Pts',(1.50073662771819,0.00758669747972766,
-27.4826030317379));
#24446=CARTESIAN_POINT('Ctrl Pts',(1.49209334404164,0.185831428521481,-27.4727598316343));
#24447=CARTESIAN_POINT('Ctrl Pts',(1.47377345415873,0.298688849505142,-27.4664850934286));
#24448=CARTESIAN_POINT('Ctrl Pts',(1.42287499434697,0.477994779563694,-27.4567019590445));
#24449=CARTESIAN_POINT('Ctrl Pts',(1.39810301767802,0.546059877122668,-27.4530022054626));
#24450=CARTESIAN_POINT('Ctrl Pts',(1.3211654313417,0.718060732051041,-27.4433751381407));
#24451=CARTESIAN_POINT('Ctrl Pts',(1.26142600296818,0.818813512273715,-27.437442313619));
#24452=CARTESIAN_POINT('Ctrl Pts',(1.15102961233378,0.963050066249823,-27.4276836194461));
#24453=CARTESIAN_POINT('Ctrl Pts',(1.10813272831953,1.01208011949452,-27.4241083088924));
#24454=CARTESIAN_POINT('Ctrl Pts',(0.982182829837723,1.13850704971315,-27.4142648510938));
#24455=CARTESIAN_POINT('Ctrl Pts',(0.89288499655155,1.20995281268992,-27.4079884319172));
#24456=CARTESIAN_POINT('Ctrl Pts',(0.734889103031064,1.30881027007612,-27.3982060630653));
#24457=CARTESIAN_POINT('Ctrl Pts',(0.670903938435668,1.34266718389571,-27.3945084402764));
#24458=CARTESIAN_POINT('Ctrl Pts',(0.498457411270812,1.41867699508727,-27.384880025534));
#24459=CARTESIAN_POINT('Ctrl Pts',(0.386502941276246,1.45336875310848,-27.3789439127497));
#24460=CARTESIAN_POINT('Ctrl Pts',(0.207819195303042,1.4863173466136,-27.369182131404));
#24461=CARTESIAN_POINT('Ctrl Pts',(0.143130180356492,1.49391137164654,-27.3656076151228));
#24462=CARTESIAN_POINT('Ctrl Pts',(-0.0353700157144279,1.50322767800781,
-27.3557483256202));
#24463=CARTESIAN_POINT('Ctrl Pts',(-0.149822348418008,1.49627831076344,
-27.3494556410944));
#24464=CARTESIAN_POINT('Ctrl Pts',(-0.334031956674721,1.46339901016027,
-27.3396342747821));
#24465=CARTESIAN_POINT('Ctrl Pts',(-0.404614812010914,1.44541578204513,
-27.3359139830926));
#24466=CARTESIAN_POINT('Ctrl Pts',(-0.583249552166997,1.38593269121057,
-27.3262924142867));
#24467=CARTESIAN_POINT('Ctrl Pts',(-0.688942046966698,1.33675561562416,
-27.3203839820944));
#24468=CARTESIAN_POINT('Ctrl Pts',(-0.843365846049652,1.24143204859706,
-27.310632267231));
#24469=CARTESIAN_POINT('Ctrl Pts',(-0.896743611832975,1.20341140088442,
-27.3070351784615));
#24470=CARTESIAN_POINT('Ctrl Pts',(-1.03400096505333,1.09149366715439,-27.2972677764508));
#24471=CARTESIAN_POINT('Ctrl Pts',(-1.11286165108869,1.01112828548998,-27.2910898599694));
#24472=CARTESIAN_POINT('Ctrl Pts',(-1.2254782116242,0.866621664760356,-27.2814734939252));
#24473=CARTESIAN_POINT('Ctrl Pts',(-1.2650223103723,0.807682555639639,-27.2778476847045));
#24474=CARTESIAN_POINT('Ctrl Pts',(-1.35902803315271,0.643804534153842,
-27.2682017101556));
#24475=CARTESIAN_POINT('Ctrl Pts',(-1.40588725048421,0.534289432650414,
-27.2621823588722));
#24476=CARTESIAN_POINT('Ctrl Pts',(-1.45696707977077,0.35954224854904,-27.2524064771433));
#24477=CARTESIAN_POINT('Ctrl Pts',(-1.47087854861132,0.297450853862337,
-27.2489159472829));
#24478=CARTESIAN_POINT('Ctrl Pts',(-1.49565959677105,0.141117025706754,
-27.2401810071786));
#24479=CARTESIAN_POINT('Ctrl Pts',(-1.50165986851533,0.0460511064130723,
-27.234919360292));
#24480=CARTESIAN_POINT('Ctrl Pts',(-1.49516929085166,-0.152692475519053,
-27.2242975539347));
#24481=CARTESIAN_POINT('Ctrl Pts',(-1.48083468356298,-0.256280444645493,
-27.2189780886341));
#24482=CARTESIAN_POINT('Ctrl Pts',(-1.4473097275385,-0.393008834830006,
-27.2117760764486));
#24483=CARTESIAN_POINT('Ctrl Pts',(-1.4372563590701,-0.428379884357375,
-27.2098954320207));
#24484=CARTESIAN_POINT('Ctrl Pts',(-1.42592304848998,-0.463335618088616,
-27.2080029164204));
#24485=CARTESIAN_POINT('Ctrl Pts',(-0.8153253598169,-0.7851534710925,-26.95929593715));
#24486=CARTESIAN_POINT('Ctrl Pts',(-1.007722685201,-0.585362698559,-26.97879593715));
#24487=CARTESIAN_POINT('Ctrl Pts',(-1.237765138237,-0.03906361929903,-27.01779593715));
#24488=CARTESIAN_POINT('Ctrl Pts',(-0.9443499054416,0.8014417043471,-27.07629593715));
#24489=CARTESIAN_POINT('Ctrl Pts',(-0.1629354149332,1.227753484752,-27.13479593715));
#24490=CARTESIAN_POINT('Ctrl Pts',(0.7025770758952,1.019973547991,-27.19329593715));
#24491=CARTESIAN_POINT('Ctrl Pts',(1.205213243798,0.2853435668963,-27.25179593715));
#24492=CARTESIAN_POINT('Ctrl Pts',(1.08533257321,-0.5966665270227,-27.31029593715));
#24493=CARTESIAN_POINT('Ctrl Pts',(0.4048609400268,-1.170489756933,-27.36879593715));
#24494=CARTESIAN_POINT('Ctrl Pts',(-0.4847283440002,-1.139735441963,-27.42729593715));
#24495=CARTESIAN_POINT('Ctrl Pts',(-1.123947378369,-0.5202891046535,-27.48579593715));
#24496=CARTESIAN_POINT('Ctrl Pts',(-1.182629120302,0.3678951396931,-27.54429593715));
#24497=CARTESIAN_POINT('Ctrl Pts',(-0.6304634559708,1.066055484586,-27.60279593715));
#24498=CARTESIAN_POINT('Ctrl Pts',(0.2473469557286,1.213580631934,-27.66129593715));
#24499=CARTESIAN_POINT('Ctrl Pts',(0.9973985952512,0.7342714135492,-27.71979593715));
#24500=CARTESIAN_POINT('Ctrl Pts',(1.232277448493,-0.1243010718991,-27.77829593715));
#24501=CARTESIAN_POINT('Ctrl Pts',(0.8306647230819,-0.9186700084293,-27.83679593715));
#24502=CARTESIAN_POINT('Ctrl Pts',(0.,-1.23853076932,-27.89529593715));
#24503=CARTESIAN_POINT('Ctrl Pts',(-0.8306647230819,-0.9186700084293,-27.95379593715));
#24504=CARTESIAN_POINT('Ctrl Pts',(-1.232277448493,-0.1243010718991,-28.01229593715));
#24505=CARTESIAN_POINT('Ctrl Pts',(-0.9973985952511,0.7342714135493,-28.07079593715));
#24506=CARTESIAN_POINT('Ctrl Pts',(-0.2473469557286,1.213580631934,-28.12929593715));
#24507=CARTESIAN_POINT('Ctrl Pts',(0.6304634559708,1.066055484586,-28.18779593715));
#24508=CARTESIAN_POINT('Ctrl Pts',(1.182629120302,0.3678951396931,-28.24629593715));
#24509=CARTESIAN_POINT('Ctrl Pts',(1.123947378369,-0.5202891046535,-28.30479593715));
#24510=CARTESIAN_POINT('Ctrl Pts',(0.4847283440002,-1.139735441963,-28.36329593715));
#24511=CARTESIAN_POINT('Ctrl Pts',(-0.4048609400269,-1.170489756933,-28.42179593715));
#24512=CARTESIAN_POINT('Ctrl Pts',(-1.08533257321,-0.5966665270227,-28.48029593715));
#24513=CARTESIAN_POINT('Ctrl Pts',(-1.205213243798,0.2853435668963,-28.53879593715));
#24514=CARTESIAN_POINT('Ctrl Pts',(-0.7025770758952,1.019973547991,-28.59729593715));
#24515=CARTESIAN_POINT('Ctrl Pts',(0.1629354149332,1.227753484752,-28.65579593715));
#24516=CARTESIAN_POINT('Ctrl Pts',(0.9443499054416,0.8014417043471,-28.71429593715));
#24517=CARTESIAN_POINT('Ctrl Pts',(1.237765138237,-0.03906361929905,-28.77279593715));
#24518=CARTESIAN_POINT('Ctrl Pts',(1.007722685201,-0.585362698559,-28.81179593715));
#24519=CARTESIAN_POINT('Ctrl Pts',(0.8153253598169,-0.7851534710925,-28.83129593715));
#24520=CARTESIAN_POINT('Ctrl Pts',(-0.9121267933018,-0.8783726756619,-27.03688532136));
#24521=CARTESIAN_POINT('Ctrl Pts',(-1.12736694661,-0.6548612706895,-27.05638532136));
#24522=CARTESIAN_POINT('Ctrl Pts',(-1.384721734467,-0.04370153997662,-27.09538532136));
#24523=CARTESIAN_POINT('Ctrl Pts',(-1.056470083549,0.8965947679692,-27.15388532136));
#24524=CARTESIAN_POINT('Ctrl Pts',(-0.1822803077923,1.373521423722,-27.21238532136));
#24525=CARTESIAN_POINT('Ctrl Pts',(0.7859922024595,1.141072322086,-27.27088532136));
#24526=CARTESIAN_POINT('Ctrl Pts',(1.3483050393,0.3192216573772,-27.32938532136));
#24527=CARTESIAN_POINT('Ctrl Pts',(1.2141912523,-0.6675071729475,-27.38788532136));
#24528=CARTESIAN_POINT('Ctrl Pts',(0.4529290135692,-1.309458924255,-27.44638532136));
#24529=CARTESIAN_POINT('Ctrl Pts',(-0.5422788641515,-1.275053230434,-27.50488532136));
#24530=CARTESIAN_POINT('Ctrl Pts',(-1.257390691615,-0.5820616602972,-27.56338532136));
#24531=CARTESIAN_POINT('Ctrl Pts',(-1.323039562278,0.4115743610808,-27.62188532136));
#24532=CARTESIAN_POINT('Ctrl Pts',(-0.7053167222932,1.192625445694,-27.68038532136));
#24533=CARTESIAN_POINT('Ctrl Pts',(0.2767138085983,1.357665865401,-27.73888532136));
#24534=CARTESIAN_POINT('Ctrl Pts',(1.11581710464,0.8214495253824,-27.79738532136));
#24535=CARTESIAN_POINT('Ctrl Pts',(1.378582505767,-0.1390590109215,-27.85588532136));
#24536=CARTESIAN_POINT('Ctrl Pts',(0.9292873587837,-1.027741279971,-27.91438532136));
#24537=CARTESIAN_POINT('Ctrl Pts',(0.,-1.385578266913,-27.97288532136));
#24538=CARTESIAN_POINT('Ctrl Pts',(-0.9292873587837,-1.027741279971,-28.03138532136));
#24539=CARTESIAN_POINT('Ctrl Pts',(-1.378582505767,-0.1390590109215,-28.08988532136));
#24540=CARTESIAN_POINT('Ctrl Pts',(-1.11581710464,0.8214495253824,-28.14838532136));
#24541=CARTESIAN_POINT('Ctrl Pts',(-0.2767138085983,1.357665865401,-28.20688532136));
#24542=CARTESIAN_POINT('Ctrl Pts',(0.7053167222932,1.192625445694,-28.26538532136));
#24543=CARTESIAN_POINT('Ctrl Pts',(1.323039562278,0.4115743610808,-28.32388532136));
#24544=CARTESIAN_POINT('Ctrl Pts',(1.257390691615,-0.5820616602972,-28.38238532136));
#24545=CARTESIAN_POINT('Ctrl Pts',(0.5422788641515,-1.275053230434,-28.44088532136));
#24546=CARTESIAN_POINT('Ctrl Pts',(-0.4529290135692,-1.309458924255,-28.49938532136));
#24547=CARTESIAN_POINT('Ctrl Pts',(-1.2141912523,-0.6675071729475,-28.55788532136));
#24548=CARTESIAN_POINT('Ctrl Pts',(-1.3483050393,0.3192216573772,-28.61638532136));
#24549=CARTESIAN_POINT('Ctrl Pts',(-0.7859922024595,1.141072322086,-28.67488532136));
#24550=CARTESIAN_POINT('Ctrl Pts',(0.1822803077923,1.373521423722,-28.73338532136));
#24551=CARTESIAN_POINT('Ctrl Pts',(1.056470083549,0.8965947679692,-28.79188532136));
#24552=CARTESIAN_POINT('Ctrl Pts',(1.384721734467,-0.04370153997664,-28.85038532136));
#24553=CARTESIAN_POINT('Ctrl Pts',(1.12736694661,-0.6548612706895,-28.88938532136));
#24554=CARTESIAN_POINT('Ctrl Pts',(0.9121267933018,-0.8783726756619,-28.90888532136));
#24555=CARTESIAN_POINT('Ctrl Pts',(-1.008928226787,-0.9715918802313,-27.11447470556));
#24556=CARTESIAN_POINT('Ctrl Pts',(-1.247011208018,-0.7243598428201,-27.13397470556));
#24557=CARTESIAN_POINT('Ctrl Pts',(-1.531678330698,-0.0483394606542,-27.17297470556));
#24558=CARTESIAN_POINT('Ctrl Pts',(-1.168590261656,0.9917478315913,-27.23147470556));
#24559=CARTESIAN_POINT('Ctrl Pts',(-0.2016252006515,1.519289362691,-27.28997470556));
#24560=CARTESIAN_POINT('Ctrl Pts',(0.8694073290239,1.262171096181,-27.34847470556));
#24561=CARTESIAN_POINT('Ctrl Pts',(1.491396834802,0.3530997478581,-27.40697470556));
#24562=CARTESIAN_POINT('Ctrl Pts',(1.34304993139,-0.7383478188722,-27.46547470556));
#24563=CARTESIAN_POINT('Ctrl Pts',(0.5009970871116,-1.448428091577,-27.52397470556));
#24564=CARTESIAN_POINT('Ctrl Pts',(-0.5998293843028,-1.410371018906,-27.58247470556));
#24565=CARTESIAN_POINT('Ctrl Pts',(-1.390834004861,-0.6438342159409,-27.64097470556));
#24566=CARTESIAN_POINT('Ctrl Pts',(-1.463450004255,0.4552535824685,-27.69947470556));
#24567=CARTESIAN_POINT('Ctrl Pts',(-0.7801699886157,1.319195406802,-27.75797470556));
#24568=CARTESIAN_POINT('Ctrl Pts',(0.3060806614679,1.501751098868,-27.81647470556));
#24569=CARTESIAN_POINT('Ctrl Pts',(1.234235614028,0.9086276372156,-27.87497470556));
#24570=CARTESIAN_POINT('Ctrl Pts',(1.524887563041,-0.1538169499438,-27.93347470556));
#24571=CARTESIAN_POINT('Ctrl Pts',(1.027909994485,-1.136812551513,-27.99197470556));
#24572=CARTESIAN_POINT('Ctrl Pts',(0.,-1.532625764506,-28.05047470556));
#24573=CARTESIAN_POINT('Ctrl Pts',(-1.027909994485,-1.136812551513,-28.10897470556));
#24574=CARTESIAN_POINT('Ctrl Pts',(-1.524887563041,-0.1538169499438,-28.16747470556));
#24575=CARTESIAN_POINT('Ctrl Pts',(-1.234235614028,0.9086276372156,-28.22597470556));
#24576=CARTESIAN_POINT('Ctrl Pts',(-0.3060806614679,1.501751098868,-28.28447470556));
#24577=CARTESIAN_POINT('Ctrl Pts',(0.7801699886157,1.319195406802,-28.34297470556));
#24578=CARTESIAN_POINT('Ctrl Pts',(1.463450004255,0.4552535824684,-28.40147470556));
#24579=CARTESIAN_POINT('Ctrl Pts',(1.390834004861,-0.6438342159409,-28.45997470556));
#24580=CARTESIAN_POINT('Ctrl Pts',(0.5998293843027,-1.410371018906,-28.51847470556));
#24581=CARTESIAN_POINT('Ctrl Pts',(-0.5009970871116,-1.448428091577,-28.57697470556));
#24582=CARTESIAN_POINT('Ctrl Pts',(-1.34304993139,-0.7383478188722,-28.63547470556));
#24583=CARTESIAN_POINT('Ctrl Pts',(-1.491396834802,0.3530997478581,-28.69397470556));
#24584=CARTESIAN_POINT('Ctrl Pts',(-0.8694073290239,1.262171096181,-28.75247470556));
#24585=CARTESIAN_POINT('Ctrl Pts',(0.2016252006515,1.519289362691,-28.81097470556));
#24586=CARTESIAN_POINT('Ctrl Pts',(1.168590261656,0.9917478315913,-28.86947470556));
#24587=CARTESIAN_POINT('Ctrl Pts',(1.531678330698,-0.04833946065422,-28.92797470556));
#24588=CARTESIAN_POINT('Ctrl Pts',(1.247011208018,-0.7243598428201,-28.96697470556));
#24589=CARTESIAN_POINT('Ctrl Pts',(1.008928226787,-0.9715918802313,-28.98647470556));
#24590=CARTESIAN_POINT('Ctrl Pts',(-1.105729660272,-1.064811084801,-27.19206408977));
#24591=CARTESIAN_POINT('Ctrl Pts',(-1.366655469426,-0.7938584149506,-27.21156408977));
#24592=CARTESIAN_POINT('Ctrl Pts',(-1.678634926928,-0.05297738133179,-27.25056408977));
#24593=CARTESIAN_POINT('Ctrl Pts',(-1.280710439764,1.086900895213,-27.30906408977));
#24594=CARTESIAN_POINT('Ctrl Pts',(-0.2209700935106,1.665057301661,-27.36756408977));
#24595=CARTESIAN_POINT('Ctrl Pts',(0.9528224555883,1.383269870276,-27.42606408977));
#24596=CARTESIAN_POINT('Ctrl Pts',(1.634488630304,0.386977838339,-27.48456408977));
#24597=CARTESIAN_POINT('Ctrl Pts',(1.47190861048,-0.809188464797,-27.54306408977));
#24598=CARTESIAN_POINT('Ctrl Pts',(0.549065160654,-1.5873972589,-27.60156408977));
#24599=CARTESIAN_POINT('Ctrl Pts',(-0.657379904454,-1.545688807378,-27.66006408977));
#24600=CARTESIAN_POINT('Ctrl Pts',(-1.524277318107,-0.7056067715846,-27.71856408977));
#24601=CARTESIAN_POINT('Ctrl Pts',(-1.603860446231,0.4989328038561,-27.77706408977));
#24602=CARTESIAN_POINT('Ctrl Pts',(-0.8550232549381,1.44576536791,-27.83556408977));
#24603=CARTESIAN_POINT('Ctrl Pts',(0.3354475143376,1.645836332335,-27.89406408977));
#24604=CARTESIAN_POINT('Ctrl Pts',(1.352654123417,0.9958057490488,-27.95256408977));
#24605=CARTESIAN_POINT('Ctrl Pts',(1.671192620316,-0.1685748889662,-28.01106408977));
#24606=CARTESIAN_POINT('Ctrl Pts',(1.126532630187,-1.245883823055,-28.06956408977));
#24607=CARTESIAN_POINT('Ctrl Pts',(0.,-1.6796732621,-28.12806408977));
#24608=CARTESIAN_POINT('Ctrl Pts',(-1.126532630187,-1.245883823055,-28.18656408977));
#24609=CARTESIAN_POINT('Ctrl Pts',(-1.671192620316,-0.1685748889661,-28.24506408977));
#24610=CARTESIAN_POINT('Ctrl Pts',(-1.352654123417,0.9958057490488,-28.30356408977));
#24611=CARTESIAN_POINT('Ctrl Pts',(-0.3354475143376,1.645836332335,-28.36206408977));
#24612=CARTESIAN_POINT('Ctrl Pts',(0.8550232549381,1.44576536791,-28.42056408977));
#24613=CARTESIAN_POINT('Ctrl Pts',(1.603860446231,0.4989328038561,-28.47906408977));
#24614=CARTESIAN_POINT('Ctrl Pts',(1.524277318107,-0.7056067715846,-28.53756408977));
#24615=CARTESIAN_POINT('Ctrl Pts',(0.657379904454,-1.545688807378,-28.59606408977));
#24616=CARTESIAN_POINT('Ctrl Pts',(-0.549065160654,-1.5873972589,-28.65456408977));
#24617=CARTESIAN_POINT('Ctrl Pts',(-1.47190861048,-0.809188464797,-28.71306408977));
#24618=CARTESIAN_POINT('Ctrl Pts',(-1.634488630304,0.3869778383391,-28.77156408977));
#24619=CARTESIAN_POINT('Ctrl Pts',(-0.9528224555883,1.383269870276,-28.83006408977));
#24620=CARTESIAN_POINT('Ctrl Pts',(0.2209700935106,1.665057301661,-28.88856408977));
#24621=CARTESIAN_POINT('Ctrl Pts',(1.280710439764,1.086900895213,-28.94706408977));
#24622=CARTESIAN_POINT('Ctrl Pts',(1.678634926928,-0.05297738133181,-29.00556408977));
#24623=CARTESIAN_POINT('Ctrl Pts',(1.366655469426,-0.7938584149506,-29.04456408977));
#24624=CARTESIAN_POINT('Ctrl Pts',(1.105729660272,-1.064811084801,-29.06406408977));
#24625=CARTESIAN_POINT('',(1.4261636598539,-0.463388660650212,-29.0075569156963));
#24626=CARTESIAN_POINT('Ctrl Pts',(1.42588748976426,-0.463325593694187,
-28.5076008391023));
#24627=CARTESIAN_POINT('Ctrl Pts',(1.36763435850362,-0.644240382503966,
-28.5176108865489));
#24628=CARTESIAN_POINT('Ctrl Pts',(1.27635777503622,-0.810368050117181,
-28.5280493786989));
#24629=CARTESIAN_POINT('Ctrl Pts',(1.04966047086561,-1.08239655987774,-28.5467699661616));
#24630=CARTESIAN_POINT('Ctrl Pts',(0.92408437639176,-1.19119500289366,-28.5551483209267));
#24631=CARTESIAN_POINT('Ctrl Pts',(0.650993762866597,-1.35990451072788,
-28.5719826080011));
#24632=CARTESIAN_POINT('Ctrl Pts',(0.506122406967541,-1.42066853677114,
-28.5805563431055));
#24633=CARTESIAN_POINT('Ctrl Pts',(0.17319726482727,-1.50083470355692,-28.5991123122149));
#24634=CARTESIAN_POINT('Ctrl Pts',(-0.0154175621686597,-1.51001365521321,
-28.6086217388051));
#24635=CARTESIAN_POINT('Ctrl Pts',(-0.290548624637289,-1.47357359252911,
-28.6230737569627));
#24636=CARTESIAN_POINT('Ctrl Pts',(-0.380656394221635,-1.4532427499571,
-28.6279092732768));
#24637=CARTESIAN_POINT('Ctrl Pts',(-0.55146398302981,-1.39751115884482,
-28.6375975079592));
#24638=CARTESIAN_POINT('Ctrl Pts',(-0.631949162462057,-1.36300673570578,
-28.6424324236474));
#24639=CARTESIAN_POINT('Ctrl Pts',(-0.872545759602894,-1.23342936288932,
-28.6572473951109));
#24640=CARTESIAN_POINT('Ctrl Pts',(-1.01929935175539,-1.1141922477245,-28.6667738905754));
#24641=CARTESIAN_POINT('Ctrl Pts',(-1.20040868387976,-0.902724249081157,
-28.6812689206855));
#24642=CARTESIAN_POINT('Ctrl Pts',(-1.25431324256695,-0.826787649429299,
-28.6861411185158));
#24643=CARTESIAN_POINT('Ctrl Pts',(-1.34485942327074,-0.669797661876857,
-28.6959089784289));
#24644=CARTESIAN_POINT('Ctrl Pts',(-1.38190065281194,-0.589606962202177,
-28.7007869332204));
#24645=CARTESIAN_POINT('Ctrl Pts',(-1.47404045297103,-0.331532746153138,
-28.7156502560038));
#24646=CARTESIAN_POINT('Ctrl Pts',(-1.50313736921478,-0.14475772903156,
-28.7251754824662));
#24647=CARTESIAN_POINT('Ctrl Pts',(-1.4946984766088,0.184912210312043,-28.7423412654415));
#24648=CARTESIAN_POINT('Ctrl Pts',(-1.47059029656801,0.328302251719719,
-28.7500231835792));
#24649=CARTESIAN_POINT('Ctrl Pts',(-1.38029529461018,0.604358529743169,
-28.7659327193717));
#24650=CARTESIAN_POINT('Ctrl Pts',(-1.31482559171509,0.734543079084308,
-28.7736172520995));
#24651=CARTESIAN_POINT('Ctrl Pts',(-1.12699633808168,1.00498587237804,-28.790749820465));
#24652=CARTESIAN_POINT('Ctrl Pts',(-0.993718884421314,1.13801109826558,
-28.80024663256));
#24653=CARTESIAN_POINT('Ctrl Pts',(-0.767703357131606,1.2914636138517,-28.8150755728019));
#24654=CARTESIAN_POINT('Ctrl Pts',(-0.690707069155562,1.33422204109302,
-28.819937578582));
#24655=CARTESIAN_POINT('Ctrl Pts',(-0.521044176936707,1.40932035982866,
-28.829930987713));
#24656=CARTESIAN_POINT('Ctrl Pts',(-0.42823822289558,1.43987608466915,-28.835031597656));
#24657=CARTESIAN_POINT('Ctrl Pts',(-0.15314209694067,1.50221839993919,-28.8497015983913));
#24658=CARTESIAN_POINT('Ctrl Pts',(0.0350342398075006,1.51046308074883,
-28.8592116967669));
#24659=CARTESIAN_POINT('Ctrl Pts',(0.310681305755836,1.47026975261959,-28.8743513270056));
#24660=CARTESIAN_POINT('Ctrl Pts',(0.401173810472036,1.44817012665623,-28.8794868055435));
#24661=CARTESIAN_POINT('Ctrl Pts',(0.584487442095495,1.38436006314717,-28.8898945742583));
#24662=CARTESIAN_POINT('Ctrl Pts',(0.676037547156664,1.34165567091835,-28.8951444215516));
#24663=CARTESIAN_POINT('Ctrl Pts',(0.907732947634239,1.20443826480559,-28.9091253563677));
#24664=CARTESIAN_POINT('Ctrl Pts',(1.05426821906179,1.08526766225066,-28.9186722332121));
#24665=CARTESIAN_POINT('Ctrl Pts',(1.23666629088399,0.853735003985556,-28.9347757104616));
#24666=CARTESIAN_POINT('Ctrl Pts',(1.28715303728387,0.775330858687689,-28.9398939533167));
#24667=CARTESIAN_POINT('Ctrl Pts',(1.37900484632935,0.597594224210385,-28.9505712707679));
#24668=CARTESIAN_POINT('Ctrl Pts',(1.41770465425374,0.497920187231623,-28.9560998903939));
#24669=CARTESIAN_POINT('Ctrl Pts',(1.48279256077328,0.259677223472442,-28.9689074648145));
#24670=CARTESIAN_POINT('Ctrl Pts',(1.50120345823689,0.118782629153447,-28.9761921486419));
#24671=CARTESIAN_POINT('Ctrl Pts',(1.49761271373553,-0.172199249620244,
-28.9918596395611));
#24672=CARTESIAN_POINT('Ctrl Pts',(1.47277821573864,-0.320301248088973,
-29.0000996307118));
#24673=CARTESIAN_POINT('Ctrl Pts',(1.42590316226892,-0.463277358684229,
-29.0080241608978));
#24674=CARTESIAN_POINT('',(1.109870874299,-0.360618907335,-28.81554752692));
#24675=CARTESIAN_POINT('Ctrl Pts',(1.121113703131,0.1559662789859,-28.75929593715));
#24676=CARTESIAN_POINT('Ctrl Pts',(1.1593323394,-0.1187561617546,-28.77879593715));
#24677=CARTESIAN_POINT('Ctrl Pts',(1.024334051204,-0.6959369621828,-28.81779593715));
#24678=CARTESIAN_POINT('Ctrl Pts',(0.2929195077513,-1.20345490624,-28.87629593715));
#24679=CARTESIAN_POINT('Ctrl Pts',(-0.5898378721215,-1.089044468041,-28.93479593715));
#24680=CARTESIAN_POINT('Ctrl Pts',(-1.167922203495,-0.4122114903279,-28.99329593715));
#24681=CARTESIAN_POINT('Ctrl Pts',(-1.142758736536,0.4775587757172,-29.05179593715));
#24682=CARTESIAN_POINT('Ctrl Pts',(-0.5273407111551,1.120655840702,-29.11029593715));
#24683=CARTESIAN_POINT('Ctrl Pts',(0.3604572362443,1.184917394878,-29.16879593715));
#24684=CARTESIAN_POINT('Ctrl Pts',(1.062073152252,0.6371491696676,-29.22729593715));
#24685=CARTESIAN_POINT('Ctrl Pts',(1.215110792527,-0.2397169657051,-29.28579593715));
#24686=CARTESIAN_POINT('Ctrl Pts',(0.7405237188655,-0.992765376005,-29.34429593715));
#24687=CARTESIAN_POINT('Ctrl Pts',(-0.1165560417524,-1.233034125506,-29.40279593715));
#24688=CARTESIAN_POINT('Ctrl Pts',(-0.9134326886102,-0.8364204625026,-29.46129593715));
#24689=CARTESIAN_POINT('Ctrl Pts',(-1.238506321788,-0.007781867099199,-29.51979593715));
#24690=CARTESIAN_POINT('Ctrl Pts',(-0.9238710607092,0.8248761905421,-29.57829593715));
#24691=CARTESIAN_POINT('Ctrl Pts',(-0.1320411949229,1.231472122869,-29.63679593715));
#24692=CARTESIAN_POINT('Ctrl Pts',(0.7279901207168,1.001992440436,-29.69529593715));
#24693=CARTESIAN_POINT('Ctrl Pts',(1.212002560279,0.2549671752147,-29.75379593715));
#24694=CARTESIAN_POINT('Ctrl Pts',(1.069995734522,-0.6237528313713,-29.81229593715));
#24695=CARTESIAN_POINT('Ctrl Pts',(0.3753185056597,-1.180294236991,-29.87079593715));
#24696=CARTESIAN_POINT('Ctrl Pts',(-0.5132169072275,-1.127194248056,-29.92929593715));
#24697=CARTESIAN_POINT('Ctrl Pts',(-1.136667342178,-0.4918798824477,-29.98779593715));
#24698=CARTESIAN_POINT('Ctrl Pts',(-1.173010393869,0.3974985356856,-30.04629593715));
#24699=CARTESIAN_POINT('Ctrl Pts',(-0.6034742672396,1.081562421011,-30.10479593715));
#24700=CARTESIAN_POINT('Ctrl Pts',(0.2777662163492,1.206981513611,-30.16329593715));
#24701=CARTESIAN_POINT('Ctrl Pts',(1.015535997925,0.7089748153235,-30.22179593715));
#24702=CARTESIAN_POINT('Ctrl Pts',(1.228764281396,-0.1552291200295,-30.28029593715));
#24703=CARTESIAN_POINT('Ctrl Pts',(0.80731725562,-0.9392543654266,-30.33879593715));
#24704=CARTESIAN_POINT('Ctrl Pts',(-0.03112861498029,-1.238140377948,-30.39729593715));
#24705=CARTESIAN_POINT('Ctrl Pts',(-0.8534729114545,-0.8975024000936,-30.45579593715));
#24706=CARTESIAN_POINT('Ctrl Pts',(-1.235070736526,-0.09330501139524,-30.51429593715));
#24707=CARTESIAN_POINT('Ctrl Pts',(-0.9784120125535,0.7591432259322,-30.57279593715));
#24708=CARTESIAN_POINT('Ctrl Pts',(-0.47119721649,1.065892903769,-30.61179593715));
#24709=CARTESIAN_POINT('Ctrl Pts',(-0.1981104409423,1.114438723627,-30.63129593715));
#24710=CARTESIAN_POINT('Ctrl Pts',(1.254220581577,0.1744837446815,-28.83688532136));
#24711=CARTESIAN_POINT('Ctrl Pts',(1.296976815913,-0.1328557681934,-28.85638532136));
#24712=CARTESIAN_POINT('Ctrl Pts',(1.145950536365,-0.7785637255274,-28.89538532136));
#24713=CARTESIAN_POINT('Ctrl Pts',(0.3276970697449,-1.346337938953,-28.95388532136));
#24714=CARTESIAN_POINT('Ctrl Pts',(-0.6598677698274,-1.218343850632,-29.01238532136));
#24715=CARTESIAN_POINT('Ctrl Pts',(-1.306586531957,-0.461152275356,-29.07088532136));
#24716=CARTESIAN_POINT('Ctrl Pts',(-1.278435472814,0.5342580719014,-29.12938532136));
#24717=CARTESIAN_POINT('Ctrl Pts',(-0.5899504854742,1.253708358346,-29.18788532136));
#24718=CARTESIAN_POINT('Ctrl Pts',(0.403253374937,1.32559951767,-29.24638532136));
#24719=CARTESIAN_POINT('Ctrl Pts',(1.188170301526,0.712796213176,-29.30488532136));
#24720=CARTESIAN_POINT('Ctrl Pts',(1.359377697933,-0.2681779299465,-29.36338532136));
#24721=CARTESIAN_POINT('Ctrl Pts',(0.8284441504486,-1.11063379547,-29.42188532136));
#24722=CARTESIAN_POINT('Ctrl Pts',(-0.1303944337356,-1.37942902105,-29.48038532136));
#24723=CARTESIAN_POINT('Ctrl Pts',(-1.021882146958,-0.9357264619928,-29.53888532136));
#24724=CARTESIAN_POINT('Ctrl Pts',(-1.38555091679,-0.008705787692765,-29.59738532136));
#24725=CARTESIAN_POINT('Ctrl Pts',(-1.033559839496,0.9228115690148,-29.65588532136));
#24726=CARTESIAN_POINT('Ctrl Pts',(-0.1477180983746,1.377681565952,-29.71438532136));
#24727=CARTESIAN_POINT('Ctrl Pts',(0.8144224711886,1.120956364969,-29.77288532136));
#24728=CARTESIAN_POINT('Ctrl Pts',(1.355900433453,0.2852387566824,-29.83138532136));
#24729=CARTESIAN_POINT('Ctrl Pts',(1.197033511132,-0.6978093629019,-29.88988532136));
#24730=CARTESIAN_POINT('Ctrl Pts',(0.4198790837453,-1.320427464418,-29.94838532136));
#24731=CARTESIAN_POINT('Ctrl Pts',(-0.5741497994896,-1.261023053592,-30.00688532136));
#24732=CARTESIAN_POINT('Ctrl Pts',(-1.27162086324,-0.5502794859312,-30.06538532136));
#24733=CARTESIAN_POINT('Ctrl Pts',(-1.312278829779,0.4446924903434,-30.12388532136));
#24734=CARTESIAN_POINT('Ctrl Pts',(-0.6751231782377,1.209973479856,-30.18238532136));
#24735=CARTESIAN_POINT('Ctrl Pts',(0.3107446679484,1.350283251132,-30.24088532136));
#24736=CARTESIAN_POINT('Ctrl Pts',(1.136107913383,0.793149528647,-30.29938532136));
#24737=CARTESIAN_POINT('Ctrl Pts',(1.37465222959,-0.1736590647829,-30.35788532136));
#24738=CARTESIAN_POINT('Ctrl Pts',(0.9031679079763,-1.050769563483,-30.41638532136));
#24739=CARTESIAN_POINT('Ctrl Pts',(-0.03482443348539,-1.385141525401,-30.47488532136));
#24740=CARTESIAN_POINT('Ctrl Pts',(-0.9548035033152,-1.004060497225,-30.53338532136));
#24741=CARTESIAN_POINT('Ctrl Pts',(-1.381707433535,-0.1043828697565,-30.59188532136));
#24742=CARTESIAN_POINT('Ctrl Pts',(-1.094576294964,0.8492743025702,-30.65038532136));
#24743=CARTESIAN_POINT('Ctrl Pts',(-0.527141221495,1.192443562085,-30.68938532136));
#24744=CARTESIAN_POINT('Ctrl Pts',(-0.2216315720351,1.246753099329,-30.70888532136));
#24745=CARTESIAN_POINT('Ctrl Pts',(1.387327460022,0.193001210377,-28.91447470556));
#24746=CARTESIAN_POINT('Ctrl Pts',(1.434621292425,-0.1469553746322,-28.93397470556));
#24747=CARTESIAN_POINT('Ctrl Pts',(1.267567021527,-0.8611904888719,-28.97297470556));
#24748=CARTESIAN_POINT('Ctrl Pts',(0.3624746317385,-1.489220971666,-29.03147470556));
#24749=CARTESIAN_POINT('Ctrl Pts',(-0.7298976675334,-1.347643233224,-29.08997470556));
#24750=CARTESIAN_POINT('Ctrl Pts',(-1.445250860419,-0.510093060384,-29.14847470556));
#24751=CARTESIAN_POINT('Ctrl Pts',(-1.414112209091,0.5909573680856,-29.20697470556));
#24752=CARTESIAN_POINT('Ctrl Pts',(-0.6525602597933,1.386760875991,-29.26547470556));
#24753=CARTESIAN_POINT('Ctrl Pts',(0.4460495136298,1.466281640462,-29.32397470556));
#24754=CARTESIAN_POINT('Ctrl Pts',(1.3142674508,0.7884432566843,-29.38247470556));
#24755=CARTESIAN_POINT('Ctrl Pts',(1.503644603339,-0.296638894188,-29.44097470556));
#24756=CARTESIAN_POINT('Ctrl Pts',(0.9163645820317,-1.228502214935,-29.49947470556));
#24757=CARTESIAN_POINT('Ctrl Pts',(-0.1442328257188,-1.525823916594,-29.55797470556));
#24758=CARTESIAN_POINT('Ctrl Pts',(-1.130331605306,-1.035032461483,-29.61647470556));
#24759=CARTESIAN_POINT('Ctrl Pts',(-1.532595511792,-0.009629708286331,-29.67497470556));
#24760=CARTESIAN_POINT('Ctrl Pts',(-1.143248618282,1.020746947487,-29.73347470556));
#24761=CARTESIAN_POINT('Ctrl Pts',(-0.1633950018263,1.523891009035,-29.79197470556));
#24762=CARTESIAN_POINT('Ctrl Pts',(0.9008548216604,1.239920289503,-29.85047470556));
#24763=CARTESIAN_POINT('Ctrl Pts',(1.499798306627,0.3155103381501,-29.90897470556));
#24764=CARTESIAN_POINT('Ctrl Pts',(1.324071287741,-0.7718658944325,-29.96747470556));
#24765=CARTESIAN_POINT('Ctrl Pts',(0.4644396618308,-1.460560691846,-30.02597470556));
#24766=CARTESIAN_POINT('Ctrl Pts',(-0.6350826917518,-1.394851859129,-30.08447470556));
#24767=CARTESIAN_POINT('Ctrl Pts',(-1.406574384301,-0.6086790894146,-30.14297470556));
#24768=CARTESIAN_POINT('Ctrl Pts',(-1.451547265688,0.4918864450011,-30.20147470556));
#24769=CARTESIAN_POINT('Ctrl Pts',(-0.7467720892358,1.3383845387,-30.25997470556));
#24770=CARTESIAN_POINT('Ctrl Pts',(0.3437231195475,1.493584988654,-30.31847470556));
#24771=CARTESIAN_POINT('Ctrl Pts',(1.256679828841,0.8773242419706,-30.37697470556));
#24772=CARTESIAN_POINT('Ctrl Pts',(1.520540177784,-0.1920890095362,-30.43547470556));
#24773=CARTESIAN_POINT('Ctrl Pts',(0.9990185603327,-1.162284761539,-30.49397470556));
#24774=CARTESIAN_POINT('Ctrl Pts',(-0.03852025199049,-1.532142672854,-30.55247470556));
#24775=CARTESIAN_POINT('Ctrl Pts',(-1.056134095176,-1.110618594357,-30.61097470556));
#24776=CARTESIAN_POINT('Ctrl Pts',(-1.528344130543,-0.1154607281177,-30.66947470556));
#24777=CARTESIAN_POINT('Ctrl Pts',(-1.210740577374,0.9394053792083,-30.72797470556));
#24778=CARTESIAN_POINT('Ctrl Pts',(-0.5830852265001,1.318994220401,-30.76697470556));
#24779=CARTESIAN_POINT('Ctrl Pts',(-0.2451527031279,1.379067475031,-30.78647470556));
#24780=CARTESIAN_POINT('Ctrl Pts',(1.520434338468,0.2115186760726,-28.99206408977));
#24781=CARTESIAN_POINT('Ctrl Pts',(1.572265768938,-0.161054981071,-29.01156408977));
#24782=CARTESIAN_POINT('Ctrl Pts',(1.389183506688,-0.9438172522165,-29.05056408977));
#24783=CARTESIAN_POINT('Ctrl Pts',(0.3972521937322,-1.632104004379,-29.10906408977));
#24784=CARTESIAN_POINT('Ctrl Pts',(-0.7999275652393,-1.476942615815,-29.16756408977));
#24785=CARTESIAN_POINT('Ctrl Pts',(-1.583915188882,-0.559033845412,-29.22606408977));
#24786=CARTESIAN_POINT('Ctrl Pts',(-1.549788945368,0.6476566642697,-29.28456408977));
#24787=CARTESIAN_POINT('Ctrl Pts',(-0.7151700341124,1.519813393635,-29.34306408977));
#24788=CARTESIAN_POINT('Ctrl Pts',(0.4888456523225,1.606963763254,-29.40156408977));
#24789=CARTESIAN_POINT('Ctrl Pts',(1.440364600074,0.8640903001927,-29.46006408977));
#24790=CARTESIAN_POINT('Ctrl Pts',(1.647911508744,-0.3250998584294,-29.51856408977));
#24791=CARTESIAN_POINT('Ctrl Pts',(1.004285013615,-1.3463706344,-29.57706408977));
#24792=CARTESIAN_POINT('Ctrl Pts',(-0.1580712177019,-1.672218812138,-29.63556408977));
#24793=CARTESIAN_POINT('Ctrl Pts',(-1.238781063654,-1.134338460973,-29.69406408977));
#24794=CARTESIAN_POINT('Ctrl Pts',(-1.679640106794,-0.0105536288799,-29.75256408977));
#24795=CARTESIAN_POINT('Ctrl Pts',(-1.252937397068,1.11868232596,-29.81106408977));
#24796=CARTESIAN_POINT('Ctrl Pts',(-0.179071905278,1.670100452118,-29.86956408977));
#24797=CARTESIAN_POINT('Ctrl Pts',(0.9872871721321,1.358884214036,-29.92806408977));
#24798=CARTESIAN_POINT('Ctrl Pts',(1.643696179801,0.3457819196178,-29.98656408977));
#24799=CARTESIAN_POINT('Ctrl Pts',(1.451109064351,-0.8459224259632,-30.04506408977));
#24800=CARTESIAN_POINT('Ctrl Pts',(0.5090002399164,-1.600693919274,-30.10356408977));
#24801=CARTESIAN_POINT('Ctrl Pts',(-0.6960155840139,-1.528680664665,-30.16206408977));
#24802=CARTESIAN_POINT('Ctrl Pts',(-1.541527905363,-0.6670786928981,-30.22056408977));
#24803=CARTESIAN_POINT('Ctrl Pts',(-1.590815701598,0.5390803996589,-30.27906408977));
#24804=CARTESIAN_POINT('Ctrl Pts',(-0.818421000234,1.466795597545,-30.33756408977));
#24805=CARTESIAN_POINT('Ctrl Pts',(0.3767015711466,1.636886726176,-30.39606408977));
#24806=CARTESIAN_POINT('Ctrl Pts',(1.377251744299,0.9614989552941,-30.45456408977));
#24807=CARTESIAN_POINT('Ctrl Pts',(1.666428125978,-0.2105189542896,-30.51306408977));
#24808=CARTESIAN_POINT('Ctrl Pts',(1.094869212689,-1.273799959595,-30.57156408977));
#24809=CARTESIAN_POINT('Ctrl Pts',(-0.0422160704956,-1.679143820308,-30.63006408977));
#24810=CARTESIAN_POINT('Ctrl Pts',(-1.157464687037,-1.217176691488,-30.68856408977));
#24811=CARTESIAN_POINT('Ctrl Pts',(-1.674980827552,-0.126538586479,-30.74706408977));
#24812=CARTESIAN_POINT('Ctrl Pts',(-1.326904859784,1.029536455846,-30.80556408977));
#24813=CARTESIAN_POINT('Ctrl Pts',(-0.6390292315051,1.445544878716,-30.84456408977));
#24814=CARTESIAN_POINT('Ctrl Pts',(-0.2686738342207,1.511381850733,-30.86406408977));
#24815=CARTESIAN_POINT('Ctrl Pts',(1.42593782207375,-0.463290149673499,
-29.0080029164203));
#24816=CARTESIAN_POINT('Ctrl Pts',(1.4000955218869,-0.542653335440824,-29.0123014375039));
#24817=CARTESIAN_POINT('Ctrl Pts',(1.36765200184006,-0.619868124763615,
-29.0165388034481));
#24818=CARTESIAN_POINT('Ctrl Pts',(1.29873520723083,-0.752009101820746,
-29.0242292609336));
#24819=CARTESIAN_POINT('Ctrl Pts',(1.26459120876806,-0.808214901017139,
-29.0276605707244));
#24820=CARTESIAN_POINT('Ctrl Pts',(1.17296738697668,-0.93860426373619,-29.036227725297));
#24821=CARTESIAN_POINT('Ctrl Pts',(1.11190361127669,-1.01012236415906,-29.0414340737163));
#24822=CARTESIAN_POINT('Ctrl Pts',(1.00102607386565,-1.11785813869305,-29.049956093286));
#24823=CARTESIAN_POINT('Ctrl Pts',(0.95469123817742,-1.15770678670362,-29.0532986472221));
#24824=CARTESIAN_POINT('Ctrl Pts',(0.810813094380322,-1.26679388253448,
-29.0629595926022));
#24825=CARTESIAN_POINT('Ctrl Pts',(0.70691663902075,-1.32739491843066,-29.0690181195741));
#24826=CARTESIAN_POINT('Ctrl Pts',(0.534047586467599,-1.40258022987199,
-29.0786488439575));
#24827=CARTESIAN_POINT('Ctrl Pts',(0.468714984262451,-1.42581466419004,
-29.0821999292582));
#24828=CARTESIAN_POINT('Ctrl Pts',(0.290798924709339,-1.4754685423226,-29.0919233537941));
#24829=CARTESIAN_POINT('Ctrl Pts',(0.176323319900497,-1.49336271384772,
-29.0983060249261));
#24830=CARTESIAN_POINT('Ctrl Pts',(-0.0011232688530839,-1.50067293458033,
-29.1080926796056));
#24831=CARTESIAN_POINT('Ctrl Pts',(-0.0639686211733561,-1.49933192056413,
-29.1115332629733));
#24832=CARTESIAN_POINT('Ctrl Pts',(-0.243291143340492,-1.4841146140882,
-29.1211707508265));
#24833=CARTESIAN_POINT('Ctrl Pts',(-0.358745366957707,-1.46033381204158,
-29.1271252317688));
#24834=CARTESIAN_POINT('Ctrl Pts',(-0.537227030820788,-1.40146808975044,
-29.1367339290109));
#24835=CARTESIAN_POINT('Ctrl Pts',(-0.603061083869039,-1.37449094299913,
-29.1403766948368));
#24836=CARTESIAN_POINT('Ctrl Pts',(-0.771966740133044,-1.29077131310097,
-29.1502995717576));
#24837=CARTESIAN_POINT('Ctrl Pts',(-0.870613016983697,-1.22624541954956,
-29.1567947691127));
#24838=CARTESIAN_POINT('Ctrl Pts',(-1.00821324287481,-1.11150228748402,
-29.1666683908791));
#24839=CARTESIAN_POINT('Ctrl Pts',(-1.05360404238008,-1.0686051413095,-29.1700860631929));
#24840=CARTESIAN_POINT('Ctrl Pts',(-1.17654781894306,-0.936825581166674,
-29.1797352518379));
#24841=CARTESIAN_POINT('Ctrl Pts',(-1.24654830775745,-0.841141577531135,
-29.1857194157032));
#24842=CARTESIAN_POINT('Ctrl Pts',(-1.33928860282852,-0.677463839254871,
-29.1953359409272));
#24843=CARTESIAN_POINT('Ctrl Pts',(-1.36974740351839,-0.613701793509182,
-29.1989543208077));
#24844=CARTESIAN_POINT('Ctrl Pts',(-1.43846410791663,-0.4390499407593,-29.2088339443768));
#24845=CARTESIAN_POINT('Ctrl Pts',(-1.46823431736669,-0.325357653795937,
-29.2153100443318));
#24846=CARTESIAN_POINT('Ctrl Pts',(-1.49330306011693,-0.148275815140815,
-29.2251662171994));
#24847=CARTESIAN_POINT('Ctrl Pts',(-1.49820320931145,-0.0859865051388653,
-29.228585503324));
#24848=CARTESIAN_POINT('Ctrl Pts',(-1.5010074205354,0.0941459644453279,
-29.2382311308569));
#24849=CARTESIAN_POINT('Ctrl Pts',(-1.48877467195723,0.211968912555517,
-29.2442108556331));
#24850=CARTESIAN_POINT('Ctrl Pts',(-1.4478272251766,0.395544928525086,-29.2538255812004));
#24851=CARTESIAN_POINT('Ctrl Pts',(-1.42764604026499,0.463327876329372,
-29.25744694048));
#24852=CARTESIAN_POINT('Ctrl Pts',(-1.36146963093795,0.639017431313202,
-29.2673293247307));
#24853=CARTESIAN_POINT('Ctrl Pts',(-1.30730802162139,0.743313376844862,
-29.2738049665947));
#24854=CARTESIAN_POINT('Ctrl Pts',(-1.20713841752504,0.891492870058028,
-29.2836618170511));
#24855=CARTESIAN_POINT('Ctrl Pts',(-1.16898821411711,0.940997459424659,
-29.2870820680485));
#24856=CARTESIAN_POINT('Ctrl Pts',(-1.05025484597231,1.07649922644131,-29.2967281671057));
#24857=CARTESIAN_POINT('Ctrl Pts',(-0.962169757854717,1.15568550758944,
-29.3027074683553));
#24858=CARTESIAN_POINT('Ctrl Pts',(-0.808680084431039,1.26439632004502,
-29.312322294698));
#24859=CARTESIAN_POINT('Ctrl Pts',(-0.748241673711729,1.30114647916462,
-29.3159442290259));
#24860=CARTESIAN_POINT('Ctrl Pts',(-0.581290337223563,1.38710162391503,
-29.3258287276009));
#24861=CARTESIAN_POINT('Ctrl Pts',(-0.471139424218073,1.42814660880992,
-29.3323060308231));
#24862=CARTESIAN_POINT('Ctrl Pts',(-0.297438103245898,1.47087436946332,
-29.3421639285785));
#24863=CARTESIAN_POINT('Ctrl Pts',(-0.235947676930806,1.48200420050721,
-29.3455836417905));
#24864=CARTESIAN_POINT('Ctrl Pts',(-0.0570020925865009,1.50287634541186,
-29.3552295209647));
#24865=CARTESIAN_POINT('Ctrl Pts',(0.0614499559187976,1.50253268545666,
-29.3612090870096));
#24866=CARTESIAN_POINT('Ctrl Pts',(0.24820953664258,1.48022037915887,-29.3708238543927));
#24867=CARTESIAN_POINT('Ctrl Pts',(0.317679980760958,1.4669444814521,-29.3744454300582));
#24868=CARTESIAN_POINT('Ctrl Pts',(0.499154349324895,1.41872967225326,-29.3843294368258));
#24869=CARTESIAN_POINT('Ctrl Pts',(0.608383825636182,1.37529774561873,-29.3908066217182));
#24870=CARTESIAN_POINT('Ctrl Pts',(0.765879412679508,1.29049204594782,-29.4006643606365));
#24871=CARTESIAN_POINT('Ctrl Pts',(0.818953429590234,1.25750673778986,-29.4040840410556));
#24872=CARTESIAN_POINT('Ctrl Pts',(0.965663498578195,1.15298535586764,-29.4137286274331));
#24873=CARTESIAN_POINT('Ctrl Pts',(1.05327773123505,1.07330395093089,-29.4197070779835));
#24874=CARTESIAN_POINT('Ctrl Pts',(1.17683781014979,0.931511944925617,-29.4293211698108));
#24875=CARTESIAN_POINT('Ctrl Pts',(1.21947089419789,0.875065016530118,-29.432943240646));
#24876=CARTESIAN_POINT('Ctrl Pts',(1.32177199388042,0.717549504139619,-29.4428298530652));
#24877=CARTESIAN_POINT('Ctrl Pts',(1.37367890501952,0.612037813295693,-29.44930934989));
#24878=CARTESIAN_POINT('Ctrl Pts',(1.43362095888831,0.443475239829729,-29.4591685104264));
#24879=CARTESIAN_POINT('Ctrl Pts',(1.45085892857129,0.3834248374722,-29.4625874127304));
#24880=CARTESIAN_POINT('Ctrl Pts',(1.48955047484412,0.207602469875726,-29.4722262250227));
#24881=CARTESIAN_POINT('Ctrl Pts',(1.50109445264084,0.0898315631773016,
-29.4782002269599));
#24882=CARTESIAN_POINT('Ctrl Pts',(1.49767544684285,-0.0981555915514404,
-29.4878113535259));
#24883=CARTESIAN_POINT('Ctrl Pts',(1.49144511132647,-0.168653636923899,
-29.4914350984059));
#24884=CARTESIAN_POINT('Ctrl Pts',(1.46166396955629,-0.354315276620493,
-29.5013327052724));
#24885=CARTESIAN_POINT('Ctrl Pts',(1.42933928187306,-0.4675621445785,-29.5078224540884));
#24886=CARTESIAN_POINT('Ctrl Pts',(1.3606586283959,-0.632882317148081,-29.5176877742471));
#24887=CARTESIAN_POINT('Ctrl Pts',(1.33318501212234,-0.688924104651172,
-29.5211031065141));
#24888=CARTESIAN_POINT('Ctrl Pts',(1.24418462634253,-0.844844025520772,
-29.5307147857776));
#24889=CARTESIAN_POINT('Ctrl Pts',(1.17404956835561,-0.939607737096756,
-29.5366678050766));
#24890=CARTESIAN_POINT('Ctrl Pts',(1.04571137208454,-1.07665016627595,-29.546265015286));
#24891=CARTESIAN_POINT('Ctrl Pts',(0.993712342102203,-1.12490439718285,
-29.5498967185494));
#24892=CARTESIAN_POINT('Ctrl Pts',(0.846363214782337,-1.24333002925605,
-29.5598459409067));
#24893=CARTESIAN_POINT('Ctrl Pts',(0.745683333010676,-1.30605320820971,
-29.5663837258148));
#24894=CARTESIAN_POINT('Ctrl Pts',(0.583272603705027,-1.38263899253368,
-29.5762779547346));
#24895=CARTESIAN_POINT('Ctrl Pts',(0.525552156721495,-1.40561680906026,
-29.5796766498336));
#24896=CARTESIAN_POINT('Ctrl Pts',(0.357140973166551,-1.46072903308538,
-29.5891607967467));
#24897=CARTESIAN_POINT('Ctrl Pts',(0.243627541970809,-1.48372465370254,
-29.5950149192744));
#24898=CARTESIAN_POINT('Ctrl Pts',(0.0578093582639404,-1.49981650319702,
-29.6045471525713));
#24899=CARTESIAN_POINT('Ctrl Pts',(-0.0139122887500927,-1.50092767768368,
-29.6082167101067));
#24900=CARTESIAN_POINT('Ctrl Pts',(-0.207419868633202,-1.49001433957701,
-29.6184109075986));
#24901=CARTESIAN_POINT('Ctrl Pts',(-0.32808953137425,-1.46803030233152,
-29.6251771153634));
#24902=CARTESIAN_POINT('Ctrl Pts',(-0.502081418207972,-1.41409095323784,
-29.6352089803415));
#24903=CARTESIAN_POINT('Ctrl Pts',(-0.55894291523991,-1.39261798704368,
-29.6385298514441));
#24904=CARTESIAN_POINT('Ctrl Pts',(-0.709589558883048,-1.32491590422671,
-29.6473577240915));
#24905=CARTESIAN_POINT('Ctrl Pts',(-0.80028128622474,-1.27203083155135,
-29.6526918901923));
#24906=CARTESIAN_POINT('Ctrl Pts',(-0.970678122639343,-1.14751854395336,
-29.663472590764));
#24907=CARTESIAN_POINT('Ctrl Pts',(-1.05026685851864,-1.07537692391356,
-29.6689386958154));
#24908=CARTESIAN_POINT('Ctrl Pts',(-1.16364069583314,-0.947688958144565,
-29.6781017466052));
#24909=CARTESIAN_POINT('Ctrl Pts',(-1.20288749268217,-0.897310890384465,
-29.6816027079286));
#24910=CARTESIAN_POINT('Ctrl Pts',(-1.30485094509196,-0.747746430700471,
-29.6915841548083));
#24911=CARTESIAN_POINT('Ctrl Pts',(-1.35969032092745,-0.642944917584904,
-29.698081098428));
#24912=CARTESIAN_POINT('Ctrl Pts',(-1.42743368712507,-0.464312075170907,
-29.7081027051918));
#24913=CARTESIAN_POINT('Ctrl Pts',(-1.44831173355896,-0.394167874022602,
-29.7118384577069));
#24914=CARTESIAN_POINT('Ctrl Pts',(-1.48860958462676,-0.211378996370762,
-29.7214010962492));
#24915=CARTESIAN_POINT('Ctrl Pts',(-1.5005971977563,-0.0969130400351905,
-29.727236335208));
#24916=CARTESIAN_POINT('Ctrl Pts',(-1.49850151240142,0.082424701531096,
-29.7368697375097));
#24917=CARTESIAN_POINT('Ctrl Pts',(-1.49351601330572,0.14710677398852,-29.7404292575701));
#24918=CARTESIAN_POINT('Ctrl Pts',(-1.46828906970983,0.324341670760753,
-29.7503031910294));
#24919=CARTESIAN_POINT('Ctrl Pts',(-1.43925965497355,0.435838974217578,
-29.7566274304292));
#24920=CARTESIAN_POINT('Ctrl Pts',(-1.37126409426303,0.610499512478932,
-29.7664638324321));
#24921=CARTESIAN_POINT('Ctrl Pts',(-1.3400864136786,0.676065726814819,-29.770171673663));
#24922=CARTESIAN_POINT('Ctrl Pts',(-1.24731552899021,0.839758478885043,
-29.7797847505764));
#24923=CARTESIAN_POINT('Ctrl Pts',(-1.1785941035599,0.934058007629023,-29.785696171446));
#24924=CARTESIAN_POINT('Ctrl Pts',(-1.05546483765357,1.06692218661126,-29.7954280112206));
#24925=CARTESIAN_POINT('Ctrl Pts',(-1.00818706494207,1.11167326541079,-29.7990005193374));
#24926=CARTESIAN_POINT('Ctrl Pts',(-0.870823071904622,1.22580137835212,
-29.8088510704562));
#24927=CARTESIAN_POINT('Ctrl Pts',(-0.775048385234494,1.28863138475216,
-29.8151376173598));
#24928=CARTESIAN_POINT('Ctrl Pts',(-0.608201585969179,1.372278790715,-29.8249336332071));
#24929=CARTESIAN_POINT('Ctrl Pts',(-0.541229418304693,1.39998227251173,
-29.8286354732767));
#24930=CARTESIAN_POINT('Ctrl Pts',(-0.362461907410498,1.45934520329591,
-29.8382595610624));
#24931=CARTESIAN_POINT('Ctrl Pts',(-0.247910310152804,1.48329652730199,
-29.8441874915178));
#24932=CARTESIAN_POINT('Ctrl Pts',(-0.067079679465184,1.49927833357457,
-29.8539407146482));
#24933=CARTESIAN_POINT('Ctrl Pts',(-0.00194837874329868,1.50075347353078,
-29.8575160674771));
#24934=CARTESIAN_POINT('Ctrl Pts',(0.176388759810885,1.49324364664456,-29.8673615289051));
#24935=CARTESIAN_POINT('Ctrl Pts',(0.289422272377968,1.47562607794796,-29.8736398585918));
#24936=CARTESIAN_POINT('Ctrl Pts',(0.469118635181389,1.42582691494393,-29.8834270879709));
#24937=CARTESIAN_POINT('Ctrl Pts',(0.537351848546642,1.40147387957845,-29.8871276392637));
#24938=CARTESIAN_POINT('Ctrl Pts',(0.709816341005259,1.32561097995918,-29.896754122299));
#24939=CARTESIAN_POINT('Ctrl Pts',(0.810915190645302,1.26651567965261,-29.9026856271651));
#24940=CARTESIAN_POINT('Ctrl Pts',(0.955828205322697,1.15703460075147,-29.9124434958545));
#24941=CARTESIAN_POINT('Ctrl Pts',(1.00513484970065,1.11443713551617,-29.9160194809169));
#24942=CARTESIAN_POINT('Ctrl Pts',(1.13235626326785,0.989268123702891,-29.9258637314856));
#24943=CARTESIAN_POINT('Ctrl Pts',(1.20435935345013,0.900415694635981,-29.9321401581186));
#24944=CARTESIAN_POINT('Ctrl Pts',(1.30422842122028,0.742995114867555,-29.9419252301247));
#24945=CARTESIAN_POINT('Ctrl Pts',(1.33850428637846,0.679176789630696,-29.9456253690681));
#24946=CARTESIAN_POINT('Ctrl Pts',(1.41555872677202,0.507229225985164,-29.9552524128281));
#24947=CARTESIAN_POINT('Ctrl Pts',(1.45092135482842,0.395571776845064,-29.9611848560455));
#24948=CARTESIAN_POINT('Ctrl Pts',(1.48498494282667,0.217154597218618,-29.9709437897809));
#24949=CARTESIAN_POINT('Ctrl Pts',(1.49298796863473,0.152489011855701,-29.974519777317));
#24950=CARTESIAN_POINT('Ctrl Pts',(1.50340388108982,-0.0256836768169241,
-29.9843642610041));
#24951=CARTESIAN_POINT('Ctrl Pts',(1.49721842404337,-0.139884647900195,
-29.9906409088091));
#24952=CARTESIAN_POINT('Ctrl Pts',(1.46571162513833,-0.323642057804169,
-30.0004266086903));
#24953=CARTESIAN_POINT('Ctrl Pts',(1.44833022129799,-0.393974312375014,
-30.0041271460791));
#24954=CARTESIAN_POINT('Ctrl Pts',(1.39015726367332,-0.573192420094281,
-30.0137542167653));
#24955=CARTESIAN_POINT('Ctrl Pts',(1.34150154456984,-0.679722243649215,
-30.0196863198532));
#24956=CARTESIAN_POINT('Ctrl Pts',(1.24710292264637,-0.834908846390197,
-30.0294454373799));
#24957=CARTESIAN_POINT('Ctrl Pts',(1.20966154490511,-0.888249374199367,
-30.0330220191137));
#24958=CARTESIAN_POINT('Ctrl Pts',(1.09789944996753,-1.02737167537288,-30.0428652025311));
#24959=CARTESIAN_POINT('Ctrl Pts',(1.01674273887224,-1.10790672760907,-30.0491399138216));
#24960=CARTESIAN_POINT('Ctrl Pts',(0.870172106627214,-1.22305059251458,
-30.0589230193631));
#24961=CARTESIAN_POINT('Ctrl Pts',(0.810123582582305,-1.26355577891347,
-30.0626227686683));
#24962=CARTESIAN_POINT('Ctrl Pts',(0.646780107007148,-1.35748475497531,
-30.0722498438669));
#24963=CARTESIAN_POINT('Ctrl Pts',(0.539228676745347,-1.40388162608679,
-30.0781826801763));
#24964=CARTESIAN_POINT('Ctrl Pts',(0.365135729805777,-1.45568214313488,
-30.087941389622));
#24965=CARTESIAN_POINT('Ctrl Pts',(0.301612243337302,-1.47013413365298,
-30.0915167022075));
#24966=CARTESIAN_POINT('Ctrl Pts',(0.125404811940233,-1.49838413751754,
-30.1013601563619));
#24967=CARTESIAN_POINT('Ctrl Pts',(0.0111666855167293,-1.5036970131519,
-30.1076365696618));
#24968=CARTESIAN_POINT('Ctrl Pts',(-0.174761510899895,-1.49080673748828,
-30.1174189322172));
#24969=CARTESIAN_POINT('Ctrl Pts',(-0.246427172421646,-1.48058802757682,
-30.121116554073));
#24970=CARTESIAN_POINT('Ctrl Pts',(-0.430616825462687,-1.44071973987913,
-30.1307449705376));
#24971=CARTESIAN_POINT('Ctrl Pts',(-0.541581250336894,-1.40298076176452,
-30.136681085897));
#24972=CARTESIAN_POINT('Ctrl Pts',(-0.705506188167064,-1.32460903371917,
-30.1464428705794));
#24973=CARTESIAN_POINT('Ctrl Pts',(-0.762304362372859,-1.29272947476832,
-30.1500173873045));
#24974=CARTESIAN_POINT('Ctrl Pts',(-0.912190026328416,-1.19534674499311,
-30.1598766760129));
#24975=CARTESIAN_POINT('Ctrl Pts',(-1.00069915444838,-1.12245120893206,
-30.1661693592564));
#24976=CARTESIAN_POINT('Ctrl Pts',(-1.13040187285673,-0.987575625605336,
-30.1759907241941));
#24977=CARTESIAN_POINT('Ctrl Pts',(-1.17693432414073,-0.931539330981527,
-30.1797110156791));
#24978=CARTESIAN_POINT('Ctrl Pts',(-1.28648958818024,-0.778417630040102,
-30.1893325848552));
#24979=CARTESIAN_POINT('Ctrl Pts',(-1.34309105930442,-0.676508040664117,
-30.1952410176057));
#24980=CARTESIAN_POINT('Ctrl Pts',(-1.41199275451509,-0.508621610801896,
-30.2049927331912));
#24981=CARTESIAN_POINT('Ctrl Pts',(-1.43282829831979,-0.446487595443442,
-30.2085898220565));
#24982=CARTESIAN_POINT('Ctrl Pts',(-1.47808823425589,-0.275266401610107,
-30.2183572238959));
#24983=CARTESIAN_POINT('Ctrl Pts',(-1.49465028229549,-0.163896298659272,
-30.2245351401014));
#24984=CARTESIAN_POINT('Ctrl Pts',(-1.50082013332007,0.0192063609786526,
-30.2341515058503));
#24985=CARTESIAN_POINT('Ctrl Pts',(-1.4981684423692,0.0901325390511118,
-30.2377773150278));
#24986=CARTESIAN_POINT('Ctrl Pts',(-1.47789558605186,0.277967822606107,
-30.2474232896606));
#24987=CARTESIAN_POINT('Ctrl Pts',(-1.45143412726189,0.394110560301101,
-30.2534426410668));
#24988=CARTESIAN_POINT('Ctrl Pts',(-1.39004475838229,0.565507974979767,
-30.2632185229554));
#24989=CARTESIAN_POINT('Ctrl Pts',(-1.36480296677769,0.623917925008732,
-30.2667090528369));
#24990=CARTESIAN_POINT('Ctrl Pts',(-1.29296053725923,0.764960582826655,
-30.2754439929124));
#24991=CARTESIAN_POINT('Ctrl Pts',(-1.24193651414017,0.845397397549996,
-30.2807056397472));
#24992=CARTESIAN_POINT('Ctrl Pts',(-1.11986698073447,1.0023692661947,-30.2913274460477));
#24993=CARTESIAN_POINT('Ctrl Pts',(-1.04738255940246,1.07774802276584,-30.2966469113402));
#24994=CARTESIAN_POINT('Ctrl Pts',(-0.939893368921114,1.16865813938709,
-30.3038489235285));
#24995=CARTESIAN_POINT('Ctrl Pts',(-0.91096944153804,1.19136469798677,-30.3057295679678));
#24996=CARTESIAN_POINT('Ctrl Pts',(-0.88125413572515,1.21298292793906,-30.3076220835796));
#24997=CARTESIAN_POINT('Ctrl Pts',(1.520434338468,0.2115186760726,-28.45156091023));
#24998=CARTESIAN_POINT('Ctrl Pts',(1.572265768938,-0.161054981071,-28.47106091023));
#24999=CARTESIAN_POINT('Ctrl Pts',(1.389183506688,-0.9438172522165,-28.51006091023));
#25000=CARTESIAN_POINT('Ctrl Pts',(0.3972521937322,-1.632104004379,-28.56856091023));
#25001=CARTESIAN_POINT('Ctrl Pts',(-0.7999275652393,-1.476942615815,-28.62706091023));
#25002=CARTESIAN_POINT('Ctrl Pts',(-1.583915188882,-0.559033845412,-28.68556091023));
#25003=CARTESIAN_POINT('Ctrl Pts',(-1.549788945368,0.6476566642697,-28.74406091023));
#25004=CARTESIAN_POINT('Ctrl Pts',(-0.7151700341124,1.519813393635,-28.80256091023));
#25005=CARTESIAN_POINT('Ctrl Pts',(0.4888456523225,1.606963763254,-28.86106091023));
#25006=CARTESIAN_POINT('Ctrl Pts',(1.440364600074,0.8640903001927,-28.91956091023));
#25007=CARTESIAN_POINT('Ctrl Pts',(1.647911508744,-0.3250998584294,-28.97806091023));
#25008=CARTESIAN_POINT('Ctrl Pts',(1.004285013615,-1.3463706344,-29.03656091023));
#25009=CARTESIAN_POINT('Ctrl Pts',(-0.1580712177019,-1.672218812138,-29.09506091023));
#25010=CARTESIAN_POINT('Ctrl Pts',(-1.238781063654,-1.134338460973,-29.15356091023));
#25011=CARTESIAN_POINT('Ctrl Pts',(-1.679640106794,-0.0105536288799,-29.21206091023));
#25012=CARTESIAN_POINT('Ctrl Pts',(-1.252937397068,1.11868232596,-29.27056091023));
#25013=CARTESIAN_POINT('Ctrl Pts',(-0.179071905278,1.670100452118,-29.32906091023));
#25014=CARTESIAN_POINT('Ctrl Pts',(0.9872871721321,1.358884214036,-29.38756091023));
#25015=CARTESIAN_POINT('Ctrl Pts',(1.643696179801,0.3457819196178,-29.44606091023));
#25016=CARTESIAN_POINT('Ctrl Pts',(1.451109064351,-0.8459224259632,-29.50456091023));
#25017=CARTESIAN_POINT('Ctrl Pts',(0.5090002399164,-1.600693919274,-29.56306091023));
#25018=CARTESIAN_POINT('Ctrl Pts',(-0.6960155840139,-1.528680664665,-29.62156091023));
#25019=CARTESIAN_POINT('Ctrl Pts',(-1.541527905363,-0.6670786928981,-29.68006091023));
#25020=CARTESIAN_POINT('Ctrl Pts',(-1.590815701598,0.5390803996589,-29.73856091023));
#25021=CARTESIAN_POINT('Ctrl Pts',(-0.818421000234,1.466795597545,-29.79706091023));
#25022=CARTESIAN_POINT('Ctrl Pts',(0.3767015711466,1.636886726176,-29.85556091023));
#25023=CARTESIAN_POINT('Ctrl Pts',(1.377251744299,0.9614989552941,-29.91406091023));
#25024=CARTESIAN_POINT('Ctrl Pts',(1.666428125978,-0.2105189542896,-29.97256091023));
#25025=CARTESIAN_POINT('Ctrl Pts',(1.094869212689,-1.273799959595,-30.03106091023));
#25026=CARTESIAN_POINT('Ctrl Pts',(-0.0422160704956,-1.679143820308,-30.08956091023));
#25027=CARTESIAN_POINT('Ctrl Pts',(-1.157464687037,-1.217176691488,-30.14806091023));
#25028=CARTESIAN_POINT('Ctrl Pts',(-1.674980827552,-0.126538586479,-30.20656091023));
#25029=CARTESIAN_POINT('Ctrl Pts',(-1.326904859784,1.029536455846,-30.26506091023));
#25030=CARTESIAN_POINT('Ctrl Pts',(-0.6390292315051,1.445544878716,-30.30406091023));
#25031=CARTESIAN_POINT('Ctrl Pts',(-0.2686738342207,1.511381850733,-30.32356091023));
#25032=CARTESIAN_POINT('Ctrl Pts',(1.387327460022,0.193001210377,-28.52915029444));
#25033=CARTESIAN_POINT('Ctrl Pts',(1.434621292425,-0.1469553746322,-28.54865029444));
#25034=CARTESIAN_POINT('Ctrl Pts',(1.267567021527,-0.8611904888719,-28.58765029444));
#25035=CARTESIAN_POINT('Ctrl Pts',(0.3624746317385,-1.489220971666,-28.64615029444));
#25036=CARTESIAN_POINT('Ctrl Pts',(-0.7298976675334,-1.347643233224,-28.70465029444));
#25037=CARTESIAN_POINT('Ctrl Pts',(-1.445250860419,-0.510093060384,-28.76315029444));
#25038=CARTESIAN_POINT('Ctrl Pts',(-1.414112209091,0.5909573680856,-28.82165029444));
#25039=CARTESIAN_POINT('Ctrl Pts',(-0.6525602597933,1.386760875991,-28.88015029444));
#25040=CARTESIAN_POINT('Ctrl Pts',(0.4460495136298,1.466281640462,-28.93865029444));
#25041=CARTESIAN_POINT('Ctrl Pts',(1.3142674508,0.7884432566843,-28.99715029444));
#25042=CARTESIAN_POINT('Ctrl Pts',(1.503644603339,-0.296638894188,-29.05565029444));
#25043=CARTESIAN_POINT('Ctrl Pts',(0.9163645820317,-1.228502214935,-29.11415029444));
#25044=CARTESIAN_POINT('Ctrl Pts',(-0.1442328257188,-1.525823916594,-29.17265029444));
#25045=CARTESIAN_POINT('Ctrl Pts',(-1.130331605306,-1.035032461483,-29.23115029444));
#25046=CARTESIAN_POINT('Ctrl Pts',(-1.532595511792,-0.009629708286331,-29.28965029444));
#25047=CARTESIAN_POINT('Ctrl Pts',(-1.143248618282,1.020746947487,-29.34815029444));
#25048=CARTESIAN_POINT('Ctrl Pts',(-0.1633950018263,1.523891009035,-29.40665029444));
#25049=CARTESIAN_POINT('Ctrl Pts',(0.9008548216604,1.239920289503,-29.46515029444));
#25050=CARTESIAN_POINT('Ctrl Pts',(1.499798306627,0.3155103381501,-29.52365029444));
#25051=CARTESIAN_POINT('Ctrl Pts',(1.324071287741,-0.7718658944325,-29.58215029444));
#25052=CARTESIAN_POINT('Ctrl Pts',(0.4644396618308,-1.460560691846,-29.64065029444));
#25053=CARTESIAN_POINT('Ctrl Pts',(-0.6350826917518,-1.394851859129,-29.69915029444));
#25054=CARTESIAN_POINT('Ctrl Pts',(-1.406574384302,-0.6086790894146,-29.75765029444));
#25055=CARTESIAN_POINT('Ctrl Pts',(-1.451547265688,0.4918864450011,-29.81615029444));
#25056=CARTESIAN_POINT('Ctrl Pts',(-0.7467720892358,1.3383845387,-29.87465029444));
#25057=CARTESIAN_POINT('Ctrl Pts',(0.3437231195475,1.493584988654,-29.93315029444));
#25058=CARTESIAN_POINT('Ctrl Pts',(1.256679828841,0.8773242419706,-29.99165029444));
#25059=CARTESIAN_POINT('Ctrl Pts',(1.520540177784,-0.1920890095362,-30.05015029444));
#25060=CARTESIAN_POINT('Ctrl Pts',(0.9990185603327,-1.162284761539,-30.10865029444));
#25061=CARTESIAN_POINT('Ctrl Pts',(-0.03852025199049,-1.532142672854,-30.16715029444));
#25062=CARTESIAN_POINT('Ctrl Pts',(-1.056134095176,-1.110618594357,-30.22565029444));
#25063=CARTESIAN_POINT('Ctrl Pts',(-1.528344130543,-0.1154607281177,-30.28415029444));
#25064=CARTESIAN_POINT('Ctrl Pts',(-1.210740577374,0.9394053792083,-30.34265029444));
#25065=CARTESIAN_POINT('Ctrl Pts',(-0.5830852265001,1.318994220401,-30.38165029444));
#25066=CARTESIAN_POINT('Ctrl Pts',(-0.2451527031279,1.379067475031,-30.40115029444));
#25067=CARTESIAN_POINT('Ctrl Pts',(1.254220581577,0.1744837446815,-28.60673967864));
#25068=CARTESIAN_POINT('Ctrl Pts',(1.296976815913,-0.1328557681934,-28.62623967864));
#25069=CARTESIAN_POINT('Ctrl Pts',(1.145950536365,-0.7785637255274,-28.66523967864));
#25070=CARTESIAN_POINT('Ctrl Pts',(0.3276970697449,-1.346337938953,-28.72373967864));
#25071=CARTESIAN_POINT('Ctrl Pts',(-0.6598677698274,-1.218343850632,-28.78223967864));
#25072=CARTESIAN_POINT('Ctrl Pts',(-1.306586531957,-0.461152275356,-28.84073967864));
#25073=CARTESIAN_POINT('Ctrl Pts',(-1.278435472814,0.5342580719014,-28.89923967864));
#25074=CARTESIAN_POINT('Ctrl Pts',(-0.5899504854742,1.253708358346,-28.95773967864));
#25075=CARTESIAN_POINT('Ctrl Pts',(0.403253374937,1.32559951767,-29.01623967864));
#25076=CARTESIAN_POINT('Ctrl Pts',(1.188170301526,0.712796213176,-29.07473967864));
#25077=CARTESIAN_POINT('Ctrl Pts',(1.359377697933,-0.2681779299465,-29.13323967864));
#25078=CARTESIAN_POINT('Ctrl Pts',(0.8284441504486,-1.11063379547,-29.19173967864));
#25079=CARTESIAN_POINT('Ctrl Pts',(-0.1303944337356,-1.37942902105,-29.25023967864));
#25080=CARTESIAN_POINT('Ctrl Pts',(-1.021882146958,-0.9357264619928,-29.30873967864));
#25081=CARTESIAN_POINT('Ctrl Pts',(-1.38555091679,-0.008705787692765,-29.36723967864));
#25082=CARTESIAN_POINT('Ctrl Pts',(-1.033559839496,0.9228115690148,-29.42573967864));
#25083=CARTESIAN_POINT('Ctrl Pts',(-0.1477180983746,1.377681565952,-29.48423967864));
#25084=CARTESIAN_POINT('Ctrl Pts',(0.8144224711886,1.120956364969,-29.54273967864));
#25085=CARTESIAN_POINT('Ctrl Pts',(1.355900433453,0.2852387566824,-29.60123967864));
#25086=CARTESIAN_POINT('Ctrl Pts',(1.197033511132,-0.6978093629019,-29.65973967864));
#25087=CARTESIAN_POINT('Ctrl Pts',(0.4198790837453,-1.320427464418,-29.71823967864));
#25088=CARTESIAN_POINT('Ctrl Pts',(-0.5741497994896,-1.261023053592,-29.77673967864));
#25089=CARTESIAN_POINT('Ctrl Pts',(-1.27162086324,-0.5502794859312,-29.83523967864));
#25090=CARTESIAN_POINT('Ctrl Pts',(-1.312278829779,0.4446924903434,-29.89373967864));
#25091=CARTESIAN_POINT('Ctrl Pts',(-0.6751231782377,1.209973479856,-29.95223967864));
#25092=CARTESIAN_POINT('Ctrl Pts',(0.3107446679484,1.350283251132,-30.01073967864));
#25093=CARTESIAN_POINT('Ctrl Pts',(1.136107913383,0.793149528647,-30.06923967864));
#25094=CARTESIAN_POINT('Ctrl Pts',(1.37465222959,-0.1736590647829,-30.12773967864));
#25095=CARTESIAN_POINT('Ctrl Pts',(0.9031679079763,-1.050769563483,-30.18623967864));
#25096=CARTESIAN_POINT('Ctrl Pts',(-0.03482443348539,-1.385141525401,-30.24473967864));
#25097=CARTESIAN_POINT('Ctrl Pts',(-0.9548035033152,-1.004060497225,-30.30323967864));
#25098=CARTESIAN_POINT('Ctrl Pts',(-1.381707433535,-0.1043828697565,-30.36173967864));
#25099=CARTESIAN_POINT('Ctrl Pts',(-1.094576294964,0.8492743025702,-30.42023967864));
#25100=CARTESIAN_POINT('Ctrl Pts',(-0.527141221495,1.192443562085,-30.45923967864));
#25101=CARTESIAN_POINT('Ctrl Pts',(-0.2216315720351,1.246753099329,-30.47873967864));
#25102=CARTESIAN_POINT('Ctrl Pts',(1.121113703131,0.1559662789859,-28.68432906285));
#25103=CARTESIAN_POINT('Ctrl Pts',(1.1593323394,-0.1187561617546,-28.70382906285));
#25104=CARTESIAN_POINT('Ctrl Pts',(1.024334051204,-0.6959369621828,-28.74282906285));
#25105=CARTESIAN_POINT('Ctrl Pts',(0.2929195077513,-1.20345490624,-28.80132906285));
#25106=CARTESIAN_POINT('Ctrl Pts',(-0.5898378721215,-1.089044468041,-28.85982906285));
#25107=CARTESIAN_POINT('Ctrl Pts',(-1.167922203495,-0.4122114903279,-28.91832906285));
#25108=CARTESIAN_POINT('Ctrl Pts',(-1.142758736536,0.4775587757172,-28.97682906285));
#25109=CARTESIAN_POINT('Ctrl Pts',(-0.5273407111551,1.120655840702,-29.03532906285));
#25110=CARTESIAN_POINT('Ctrl Pts',(0.3604572362443,1.184917394878,-29.09382906285));
#25111=CARTESIAN_POINT('Ctrl Pts',(1.062073152252,0.6371491696676,-29.15232906285));
#25112=CARTESIAN_POINT('Ctrl Pts',(1.215110792527,-0.2397169657051,-29.21082906285));
#25113=CARTESIAN_POINT('Ctrl Pts',(0.7405237188655,-0.992765376005,-29.26932906285));
#25114=CARTESIAN_POINT('Ctrl Pts',(-0.1165560417524,-1.233034125506,-29.32782906285));
#25115=CARTESIAN_POINT('Ctrl Pts',(-0.9134326886102,-0.8364204625026,-29.38632906285));
#25116=CARTESIAN_POINT('Ctrl Pts',(-1.238506321788,-0.007781867099199,-29.44482906285));
#25117=CARTESIAN_POINT('Ctrl Pts',(-0.9238710607092,0.8248761905421,-29.50332906285));
#25118=CARTESIAN_POINT('Ctrl Pts',(-0.1320411949229,1.231472122869,-29.56182906285));
#25119=CARTESIAN_POINT('Ctrl Pts',(0.7279901207168,1.001992440436,-29.62032906285));
#25120=CARTESIAN_POINT('Ctrl Pts',(1.212002560279,0.2549671752147,-29.67882906285));
#25121=CARTESIAN_POINT('Ctrl Pts',(1.069995734522,-0.6237528313713,-29.73732906285));
#25122=CARTESIAN_POINT('Ctrl Pts',(0.3753185056597,-1.180294236991,-29.79582906285));
#25123=CARTESIAN_POINT('Ctrl Pts',(-0.5132169072275,-1.127194248056,-29.85432906285));
#25124=CARTESIAN_POINT('Ctrl Pts',(-1.136667342178,-0.4918798824477,-29.91282906285));
#25125=CARTESIAN_POINT('Ctrl Pts',(-1.173010393869,0.3974985356856,-29.97132906285));
#25126=CARTESIAN_POINT('Ctrl Pts',(-0.6034742672396,1.081562421011,-30.02982906285));
#25127=CARTESIAN_POINT('Ctrl Pts',(0.2777662163492,1.206981513611,-30.08832906285));
#25128=CARTESIAN_POINT('Ctrl Pts',(1.015535997925,0.7089748153235,-30.14682906285));
#25129=CARTESIAN_POINT('Ctrl Pts',(1.228764281396,-0.1552291200295,-30.20532906285));
#25130=CARTESIAN_POINT('Ctrl Pts',(0.80731725562,-0.9392543654266,-30.26382906285));
#25131=CARTESIAN_POINT('Ctrl Pts',(-0.03112861498029,-1.238140377948,-30.32232906285));
#25132=CARTESIAN_POINT('Ctrl Pts',(-0.8534729114545,-0.8975024000936,-30.38082906285));
#25133=CARTESIAN_POINT('Ctrl Pts',(-1.235070736526,-0.09330501139524,-30.43932906285));
#25134=CARTESIAN_POINT('Ctrl Pts',(-0.9784120125535,0.7591432259322,-30.49782906285));
#25135=CARTESIAN_POINT('Ctrl Pts',(-0.47119721649,1.065892903769,-30.53682906285));
#25136=CARTESIAN_POINT('Ctrl Pts',(-0.1981104409423,1.114438723627,-30.55632906285));
#25137=CARTESIAN_POINT('Origin',(0.,-1.5,-32.2));
#25138=CARTESIAN_POINT('',(0.,0.,0.));
#25139=CARTESIAN_POINT('Origin',(0.,0.,0.));
#25140=CARTESIAN_POINT('',(3.1999696579293,0.,0.0139351473551933));
#25141=CARTESIAN_POINT('Origin',(0.,0.,0.));
#25142=CARTESIAN_POINT('',(-1.6,0.,1.95943487863577E-16));
#25143=CARTESIAN_POINT('Origin',(0.,0.,0.));
#25144=CARTESIAN_POINT('Origin',(0.,0.,0.));
#25145=CARTESIAN_POINT('',(-1.6,0.5,1.95943487863577E-16));
#25146=CARTESIAN_POINT('',(-1.6,0.,1.95943487863577E-16));
#25147=CARTESIAN_POINT('Origin',(0.,0.5,0.));
#25148=CARTESIAN_POINT('Origin',(0.,0.5,0.));
#25149=CARTESIAN_POINT('',(3.1999696579293,0.5,0.0139351473551933));
#25150=CARTESIAN_POINT('Origin',(0.,0.5,0.));
#25151=CARTESIAN_POINT('Origin',(0.,0.25,0.));
#25152=CARTESIAN_POINT('Origin',(3.1999696579293,0.25,0.0139351473551933));
#25153=CARTESIAN_POINT('',(0.,0.,0.));
#25154=CARTESIAN_POINT('Origin',(0.,0.,-6.89357235801));
#25155=CARTESIAN_POINT('',(-1.03412062617695E-14,-1.37969296796376,-6.93054085392112));
#25156=CARTESIAN_POINT('',(1.63050934631669E-16,-1.331411920116,-7.06319194267));
#25157=CARTESIAN_POINT('',(1.70611472889645E-16,-1.393148400081,-6.89357235801));
#25158=CARTESIAN_POINT('',(-1.20239717356391,0.571750590758655,-7.06319194267005));
#25159=CARTESIAN_POINT('Ctrl Pts',(-1.20239717356391,0.571750590758656,
-7.06319194267005));
#25160=CARTESIAN_POINT('Ctrl Pts',(-1.26030469923467,0.455247401086438,
-7.05696595606331));
#25161=CARTESIAN_POINT('Ctrl Pts',(-1.30086063595672,0.330766210654013,
-7.05076352264625));
#25162=CARTESIAN_POINT('Ctrl Pts',(-1.34734301081266,0.060099744643785,
-7.03707105795902));
#25163=CARTESIAN_POINT('Ctrl Pts',(-1.34870825310244,-0.0856619352215133,
-7.02959898147411));
#25164=CARTESIAN_POINT('Ctrl Pts',(-1.31385805616803,-0.311224915923542,
-7.01860006937098));
#25165=CARTESIAN_POINT('Ctrl Pts',(-1.29345890223884,-0.392254545151923,
-7.01471383675719));
#25166=CARTESIAN_POINT('Ctrl Pts',(-1.21199792405986,-0.623330282323326,
-7.00312293352462));
#25167=CARTESIAN_POINT('Ctrl Pts',(-1.13128222774601,-0.765171563245202,
-6.99520004112136));
#25168=CARTESIAN_POINT('Ctrl Pts',(-0.91224190618221,-1.02781571641453,
-6.97811271159856));
#25169=CARTESIAN_POINT('Ctrl Pts',(-0.770549270084647,-1.14145066385306,
-6.9698410678562));
#25170=CARTESIAN_POINT('Ctrl Pts',(-0.462335849194596,-1.30185701421122,
-6.95353112872913));
#25171=CARTESIAN_POINT('Ctrl Pts',(-0.300584338674426,-1.35146726655285,
-6.94528925745892));
#25172=CARTESIAN_POINT('Ctrl Pts',(-0.0895408850961822,-1.37594598073772,
-6.93485347223636));
#25173=CARTESIAN_POINT('Ctrl Pts',(-0.0447547005702977,-1.37891813490286,
-6.9326696902598));
#25174=CARTESIAN_POINT('Ctrl Pts',(-2.1941503253841E-14,-1.37969296796376,
-6.93054085392112));
#25175=CARTESIAN_POINT('Origin',(0.,0.,-7.06319194267));
#25176=CARTESIAN_POINT('Origin',(0.,0.,0.));
#25177=CARTESIAN_POINT('',(-1.56243020438409E-6,1.11698728404643,-6.50503918006705E-18));
#25178=CARTESIAN_POINT('',(0.396369471088371,1.04429491357745,0.));
#25179=CARTESIAN_POINT('Origin',(0.,0.,0.));
#25180=CARTESIAN_POINT('Ctrl Pts',(0.396304186491244,1.0441270568326,-3.46944695195361E-18));
#25181=CARTESIAN_POINT('Ctrl Pts',(0.375051486067047,1.05226594471596,1.97766776596492E-18));
#25182=CARTESIAN_POINT('Ctrl Pts',(0.353598170411701,1.05972570838993,1.11865001012778E-17));
#25183=CARTESIAN_POINT('Ctrl Pts',(0.331925748890776,1.06650339612009,1.04083408558608E-17));
#25184=CARTESIAN_POINT('Ctrl Pts',(0.32239163755152,1.06948503014652,1.00660137707996E-17));
#25185=CARTESIAN_POINT('Ctrl Pts',(0.312814080654242,1.07233474927852,-1.11256302644907E-18));
#25186=CARTESIAN_POINT('Ctrl Pts',(0.303195534691942,1.07505027411597,0.));
#25187=CARTESIAN_POINT('Ctrl Pts',(0.278245422830036,1.08209423364204,2.88594264373481E-18));
#25188=CARTESIAN_POINT('Ctrl Pts',(0.253025137328642,1.08823279472093,5.24541165579042E-18));
#25189=CARTESIAN_POINT('Ctrl Pts',(0.227630604189116,1.09346325276002,3.46944695195361E-18));
#25190=CARTESIAN_POINT('Ctrl Pts',(0.201257125734747,1.09889534208581,1.62501978351495E-18));
#25191=CARTESIAN_POINT('Ctrl Pts',(0.17468865526933,1.10335050639761,-1.22639140354306E-17));
#25192=CARTESIAN_POINT('Ctrl Pts',(0.147988322547862,1.10683727158896,-1.38777878078145E-17));
#25193=CARTESIAN_POINT('Ctrl Pts',(0.123448118283646,1.11004194813399,-1.53610948678466E-17));
#25194=CARTESIAN_POINT('Ctrl Pts',(0.098802275556219,1.11242704532112,-1.21825797392063E-17));
#25195=CARTESIAN_POINT('Ctrl Pts',(0.0741337916335476,1.11399860667177,
-1.38777878078145E-17));
#25196=CARTESIAN_POINT('Ctrl Pts',(0.0494653077108761,1.11557016802241,
-1.55729958764226E-17));
#25197=CARTESIAN_POINT('Ctrl Pts',(0.0247654680032384,1.11633121467664,
-6.35703025728058E-19));
#25198=CARTESIAN_POINT('Ctrl Pts',(3.76960662823445E-6,1.11628565725144,
0.));
#25199=CARTESIAN_POINT('Origin',(0.,0.,0.));
#25200=CARTESIAN_POINT('',(-5.22672044210748E-8,1.11698648602171,-0.0288570210841246));
#25201=CARTESIAN_POINT('',(0.,1.116987298108,-0.02886751345948));
#25202=CARTESIAN_POINT('',(0.744968168489605,0.832275826917867,-0.0288675134594948));
#25203=CARTESIAN_POINT('Origin',(0.,0.,-0.02886751345948));
#25204=CARTESIAN_POINT('',(0.741143876287569,0.835683180862249,-0.0288670915312841));
#25205=CARTESIAN_POINT('Ctrl Pts',(0.741143755062205,0.835683044173541,
-0.028867407977449));
#25206=CARTESIAN_POINT('Ctrl Pts',(0.742421161214912,0.834550230034564,
-0.0288674431381309));
#25207=CARTESIAN_POINT('Ctrl Pts',(0.743695970158679,0.833414486969343,
-0.0288674782988128));
#25208=CARTESIAN_POINT('Ctrl Pts',(0.744968168489605,0.832275826917867,
-0.0288675134594948));
#25209=CARTESIAN_POINT('Ctrl Pts',(0.396369471088371,1.04429491357745,0.));
#25210=CARTESIAN_POINT('Ctrl Pts',(0.43828755116425,1.02838461179134,-0.003194245975093));
#25211=CARTESIAN_POINT('Ctrl Pts',(0.479311242034271,1.00992758066369,-0.00639321053358202));
#25212=CARTESIAN_POINT('Ctrl Pts',(0.519226227239376,0.988971561310726,
-0.0096049957435327));
#25213=CARTESIAN_POINT('Ctrl Pts',(0.547511184299327,0.974121496742234,
-0.0118809631848942));
#25214=CARTESIAN_POINT('Ctrl Pts',(0.575237639768719,0.958011828605387,
-0.0141633685999232));
#25215=CARTESIAN_POINT('Ctrl Pts',(0.602193922372281,0.940756665664665,
-0.0164435627914911));
#25216=CARTESIAN_POINT('Ctrl Pts',(0.613277634633324,0.933661797879479,
-0.0173811184882584));
#25217=CARTESIAN_POINT('Ctrl Pts',(0.624231431056695,0.926373805934684,
-0.0183183003473072));
#25218=CARTESIAN_POINT('Ctrl Pts',(0.635041961763314,0.918902786443926,
-0.019254507123577));
#25219=CARTESIAN_POINT('Ctrl Pts',(0.672142748844026,0.893262907059214,
-0.0224674861356659));
#25220=CARTESIAN_POINT('Ctrl Pts',(0.70755889976264,0.865468750629288,-0.0256689806051503));
#25221=CARTESIAN_POINT('Ctrl Pts',(0.741143876287569,0.835683180862249,
-0.0288670915312841));
#25222=CARTESIAN_POINT('Ctrl Pts',(-0.4755900604755,1.010680324589,0.07987340093689));
#25223=CARTESIAN_POINT('Ctrl Pts',(-0.2348081643589,1.123983684464,0.06091506760356));
#25224=CARTESIAN_POINT('Ctrl Pts',(0.329952574922,1.170452920957,0.02299840093689));
#25225=CARTESIAN_POINT('Ctrl Pts',(1.016551442463,0.6677408946503,-0.03387659906311));
#25226=CARTESIAN_POINT('Ctrl Pts',(1.205358893105,-0.1619074151071,-0.09075159906311));
#25227=CARTESIAN_POINT('Ctrl Pts',(0.8042879589087,-0.9122802996697,-0.1476265990631));
#25228=CARTESIAN_POINT('Ctrl Pts',(0.009550993186476,-1.216158607898,-0.2045015990631));
#25229=CARTESIAN_POINT('Ctrl Pts',(-0.7898556864549,-0.9248023542725,-0.2613765990631));
#25230=CARTESIAN_POINT('Ctrl Pts',(-1.202679571961,-0.180814804896,-0.3182515990631));
#25231=CARTESIAN_POINT('Ctrl Pts',(-1.026867975908,0.6516702524068,-0.3751265990631));
#25232=CARTESIAN_POINT('Ctrl Pts',(-0.348469933747,1.165204139133,-0.4320015990631));
#25233=CARTESIAN_POINT('Ctrl Pts',(0.5004819949382,1.108444747226,-0.4888765990631));
#25234=CARTESIAN_POINT('Ctrl Pts',(1.104479823299,0.5091721726955,-0.5457515990631));
#25235=CARTESIAN_POINT('Ctrl Pts',(1.167905052019,-0.3393077836576,-0.6026265990631));
#25236=CARTESIAN_POINT('Ctrl Pts',(0.6597150647482,-1.02171816845,-0.6595015990631));
#25237=CARTESIAN_POINT('Ctrl Pts',(-0.1713634724997,-1.204062516105,-0.7163765990631));
#25238=CARTESIAN_POINT('Ctrl Pts',(-0.9185704929214,-0.7970948701029,-0.7732515990631));
#25239=CARTESIAN_POINT('Ctrl Pts',(-1.216195700701,0.,-0.8301265990631));
#25240=CARTESIAN_POINT('Ctrl Pts',(-0.9185704929214,0.7970948701029,-0.8870015990631));
#25241=CARTESIAN_POINT('Ctrl Pts',(-0.1713634724997,1.204062516105,-0.9438765990631));
#25242=CARTESIAN_POINT('Ctrl Pts',(0.6597150647482,1.02171816845,-1.000751599063));
#25243=CARTESIAN_POINT('Ctrl Pts',(1.167905052019,0.3393077836576,-1.057626599063));
#25244=CARTESIAN_POINT('Ctrl Pts',(1.104479823299,-0.5091721726955,-1.114501599063));
#25245=CARTESIAN_POINT('Ctrl Pts',(0.5004819949382,-1.108444747226,-1.171376599063));
#25246=CARTESIAN_POINT('Ctrl Pts',(-0.348469933747,-1.165204139133,-1.228251599063));
#25247=CARTESIAN_POINT('Ctrl Pts',(-1.026867975908,-0.6516702524068,-1.285126599063));
#25248=CARTESIAN_POINT('Ctrl Pts',(-1.202679571961,0.180814804896,-1.342001599063));
#25249=CARTESIAN_POINT('Ctrl Pts',(-0.7898556864549,0.9248023542725,-1.398876599063));
#25250=CARTESIAN_POINT('Ctrl Pts',(0.009550993186476,1.216158607898,-1.455751599063));
#25251=CARTESIAN_POINT('Ctrl Pts',(0.8042879589087,0.9122802996697,-1.512626599063));
#25252=CARTESIAN_POINT('Ctrl Pts',(1.205358893105,0.161907415107,-1.569501599063));
#25253=CARTESIAN_POINT('Ctrl Pts',(1.016551442463,-0.6677408946503,-1.626376599063));
#25254=CARTESIAN_POINT('Ctrl Pts',(0.329952574922,-1.170452920957,-1.683251599063));
#25255=CARTESIAN_POINT('Ctrl Pts',(-0.2348081643589,-1.123983684464,-1.72116826573));
#25256=CARTESIAN_POINT('Ctrl Pts',(-0.4755900604755,-1.010680324589,-1.740126599063));
#25257=CARTESIAN_POINT('Ctrl Pts',(-0.4755900604755,1.010680324589,0.0499578003123));
#25258=CARTESIAN_POINT('Ctrl Pts',(-0.2348081643589,1.123983684464,0.03099946697896));
#25259=CARTESIAN_POINT('Ctrl Pts',(0.329952574922,1.170452920957,-0.006917199687702));
#25260=CARTESIAN_POINT('Ctrl Pts',(1.016551442463,0.6677408946503,-0.0637921996877));
#25261=CARTESIAN_POINT('Ctrl Pts',(1.205358893105,-0.1619074151071,-0.1206671996877));
#25262=CARTESIAN_POINT('Ctrl Pts',(0.8042879589087,-0.9122802996697,-0.1775421996877));
#25263=CARTESIAN_POINT('Ctrl Pts',(0.009550993186476,-1.216158607898,-0.2344171996877));
#25264=CARTESIAN_POINT('Ctrl Pts',(-0.7898556864549,-0.9248023542725,-0.2912921996877));
#25265=CARTESIAN_POINT('Ctrl Pts',(-1.202679571961,-0.180814804896,-0.3481671996877));
#25266=CARTESIAN_POINT('Ctrl Pts',(-1.026867975908,0.6516702524068,-0.4050421996877));
#25267=CARTESIAN_POINT('Ctrl Pts',(-0.348469933747,1.165204139133,-0.4619171996877));
#25268=CARTESIAN_POINT('Ctrl Pts',(0.5004819949382,1.108444747226,-0.5187921996877));
#25269=CARTESIAN_POINT('Ctrl Pts',(1.104479823299,0.5091721726955,-0.5756671996877));
#25270=CARTESIAN_POINT('Ctrl Pts',(1.167905052019,-0.3393077836576,-0.6325421996877));
#25271=CARTESIAN_POINT('Ctrl Pts',(0.6597150647482,-1.02171816845,-0.6894171996877));
#25272=CARTESIAN_POINT('Ctrl Pts',(-0.1713634724997,-1.204062516105,-0.7462921996877));
#25273=CARTESIAN_POINT('Ctrl Pts',(-0.9185704929214,-0.7970948701029,-0.8031671996877));
#25274=CARTESIAN_POINT('Ctrl Pts',(-1.216195700701,0.,-0.8600421996877));
#25275=CARTESIAN_POINT('Ctrl Pts',(-0.9185704929214,0.7970948701029,-0.9169171996877));
#25276=CARTESIAN_POINT('Ctrl Pts',(-0.1713634724997,1.204062516105,-0.9737921996877));
#25277=CARTESIAN_POINT('Ctrl Pts',(0.6597150647482,1.02171816845,-1.030667199688));
#25278=CARTESIAN_POINT('Ctrl Pts',(1.167905052019,0.3393077836576,-1.087542199688));
#25279=CARTESIAN_POINT('Ctrl Pts',(1.104479823299,-0.5091721726955,-1.144417199688));
#25280=CARTESIAN_POINT('Ctrl Pts',(0.5004819949382,-1.108444747226,-1.201292199688));
#25281=CARTESIAN_POINT('Ctrl Pts',(-0.348469933747,-1.165204139133,-1.258167199688));
#25282=CARTESIAN_POINT('Ctrl Pts',(-1.026867975908,-0.6516702524068,-1.315042199688));
#25283=CARTESIAN_POINT('Ctrl Pts',(-1.202679571961,0.180814804896,-1.371917199688));
#25284=CARTESIAN_POINT('Ctrl Pts',(-0.7898556864549,0.9248023542725,-1.428792199688));
#25285=CARTESIAN_POINT('Ctrl Pts',(0.009550993186476,1.216158607898,-1.485667199688));
#25286=CARTESIAN_POINT('Ctrl Pts',(0.8042879589087,0.9122802996697,-1.542542199688));
#25287=CARTESIAN_POINT('Ctrl Pts',(1.205358893105,0.161907415107,-1.599417199688));
#25288=CARTESIAN_POINT('Ctrl Pts',(1.016551442463,-0.6677408946503,-1.656292199688));
#25289=CARTESIAN_POINT('Ctrl Pts',(0.329952574922,-1.170452920957,-1.713167199688));
#25290=CARTESIAN_POINT('Ctrl Pts',(-0.2348081643589,-1.123983684464,-1.751083866354));
#25291=CARTESIAN_POINT('Ctrl Pts',(-0.4755900604755,-1.010680324589,-1.770042199688));
#25292=CARTESIAN_POINT('Ctrl Pts',(-0.4755900604755,1.010680324589,0.0200421996877));
#25293=CARTESIAN_POINT('Ctrl Pts',(-0.2348081643589,1.123983684464,0.001083866354369));
#25294=CARTESIAN_POINT('Ctrl Pts',(0.329952574922,1.170452920957,-0.0368328003123));
#25295=CARTESIAN_POINT('Ctrl Pts',(1.016551442463,0.6677408946503,-0.0937078003123));
#25296=CARTESIAN_POINT('Ctrl Pts',(1.205358893105,-0.1619074151071,-0.1505828003123));
#25297=CARTESIAN_POINT('Ctrl Pts',(0.8042879589087,-0.9122802996697,-0.2074578003123));
#25298=CARTESIAN_POINT('Ctrl Pts',(0.009550993186476,-1.216158607898,-0.2643328003123));
#25299=CARTESIAN_POINT('Ctrl Pts',(-0.7898556864549,-0.9248023542725,-0.3212078003123));
#25300=CARTESIAN_POINT('Ctrl Pts',(-1.202679571961,-0.180814804896,-0.3780828003123));
#25301=CARTESIAN_POINT('Ctrl Pts',(-1.026867975908,0.6516702524068,-0.4349578003123));
#25302=CARTESIAN_POINT('Ctrl Pts',(-0.348469933747,1.165204139133,-0.4918328003123));
#25303=CARTESIAN_POINT('Ctrl Pts',(0.5004819949382,1.108444747226,-0.5487078003123));
#25304=CARTESIAN_POINT('Ctrl Pts',(1.104479823299,0.5091721726955,-0.6055828003123));
#25305=CARTESIAN_POINT('Ctrl Pts',(1.167905052019,-0.3393077836576,-0.6624578003123));
#25306=CARTESIAN_POINT('Ctrl Pts',(0.6597150647482,-1.02171816845,-0.7193328003123));
#25307=CARTESIAN_POINT('Ctrl Pts',(-0.1713634724997,-1.204062516105,-0.7762078003123));
#25308=CARTESIAN_POINT('Ctrl Pts',(-0.9185704929214,-0.7970948701029,-0.8330828003123));
#25309=CARTESIAN_POINT('Ctrl Pts',(-1.216195700701,0.,-0.8899578003123));
#25310=CARTESIAN_POINT('Ctrl Pts',(-0.9185704929214,0.7970948701029,-0.9468328003123));
#25311=CARTESIAN_POINT('Ctrl Pts',(-0.1713634724997,1.204062516105,-1.003707800312));
#25312=CARTESIAN_POINT('Ctrl Pts',(0.6597150647482,1.02171816845,-1.060582800312));
#25313=CARTESIAN_POINT('Ctrl Pts',(1.167905052019,0.3393077836576,-1.117457800312));
#25314=CARTESIAN_POINT('Ctrl Pts',(1.104479823299,-0.5091721726955,-1.174332800312));
#25315=CARTESIAN_POINT('Ctrl Pts',(0.5004819949382,-1.108444747226,-1.231207800312));
#25316=CARTESIAN_POINT('Ctrl Pts',(-0.348469933747,-1.165204139133,-1.288082800312));
#25317=CARTESIAN_POINT('Ctrl Pts',(-1.026867975908,-0.6516702524068,-1.344957800312));
#25318=CARTESIAN_POINT('Ctrl Pts',(-1.202679571961,0.180814804896,-1.401832800312));
#25319=CARTESIAN_POINT('Ctrl Pts',(-0.7898556864549,0.9248023542725,-1.458707800312));
#25320=CARTESIAN_POINT('Ctrl Pts',(0.009550993186476,1.216158607898,-1.515582800312));
#25321=CARTESIAN_POINT('Ctrl Pts',(0.8042879589087,0.9122802996697,-1.572457800312));
#25322=CARTESIAN_POINT('Ctrl Pts',(1.205358893105,0.161907415107,-1.629332800312));
#25323=CARTESIAN_POINT('Ctrl Pts',(1.016551442463,-0.6677408946503,-1.686207800312));
#25324=CARTESIAN_POINT('Ctrl Pts',(0.329952574922,-1.170452920957,-1.743082800312));
#25325=CARTESIAN_POINT('Ctrl Pts',(-0.2348081643589,-1.123983684464,-1.780999466979));
#25326=CARTESIAN_POINT('Ctrl Pts',(-0.4755900604755,-1.010680324589,-1.799957800312));
#25327=CARTESIAN_POINT('Ctrl Pts',(-0.4755900604755,1.010680324589,-0.009873400936894));
#25328=CARTESIAN_POINT('Ctrl Pts',(-0.2348081643589,1.123983684464,-0.02883173427023));
#25329=CARTESIAN_POINT('Ctrl Pts',(0.329952574922,1.170452920957,-0.06674840093689));
#25330=CARTESIAN_POINT('Ctrl Pts',(1.016551442463,0.6677408946503,-0.1236234009369));
#25331=CARTESIAN_POINT('Ctrl Pts',(1.205358893105,-0.1619074151071,-0.1804984009369));
#25332=CARTESIAN_POINT('Ctrl Pts',(0.8042879589087,-0.9122802996697,-0.2373734009369));
#25333=CARTESIAN_POINT('Ctrl Pts',(0.009550993186476,-1.216158607898,-0.2942484009369));
#25334=CARTESIAN_POINT('Ctrl Pts',(-0.7898556864549,-0.9248023542725,-0.3511234009369));
#25335=CARTESIAN_POINT('Ctrl Pts',(-1.202679571961,-0.180814804896,-0.4079984009369));
#25336=CARTESIAN_POINT('Ctrl Pts',(-1.026867975908,0.6516702524068,-0.4648734009369));
#25337=CARTESIAN_POINT('Ctrl Pts',(-0.348469933747,1.165204139133,-0.5217484009369));
#25338=CARTESIAN_POINT('Ctrl Pts',(0.5004819949382,1.108444747226,-0.5786234009369));
#25339=CARTESIAN_POINT('Ctrl Pts',(1.104479823299,0.5091721726955,-0.6354984009369));
#25340=CARTESIAN_POINT('Ctrl Pts',(1.167905052019,-0.3393077836576,-0.6923734009369));
#25341=CARTESIAN_POINT('Ctrl Pts',(0.6597150647482,-1.02171816845,-0.7492484009369));
#25342=CARTESIAN_POINT('Ctrl Pts',(-0.1713634724997,-1.204062516105,-0.8061234009369));
#25343=CARTESIAN_POINT('Ctrl Pts',(-0.9185704929214,-0.7970948701029,-0.8629984009369));
#25344=CARTESIAN_POINT('Ctrl Pts',(-1.216195700701,0.,-0.9198734009369));
#25345=CARTESIAN_POINT('Ctrl Pts',(-0.9185704929214,0.7970948701029,-0.9767484009369));
#25346=CARTESIAN_POINT('Ctrl Pts',(-0.1713634724997,1.204062516105,-1.033623400937));
#25347=CARTESIAN_POINT('Ctrl Pts',(0.6597150647482,1.02171816845,-1.090498400937));
#25348=CARTESIAN_POINT('Ctrl Pts',(1.167905052019,0.3393077836576,-1.147373400937));
#25349=CARTESIAN_POINT('Ctrl Pts',(1.104479823299,-0.5091721726955,-1.204248400937));
#25350=CARTESIAN_POINT('Ctrl Pts',(0.5004819949382,-1.108444747226,-1.261123400937));
#25351=CARTESIAN_POINT('Ctrl Pts',(-0.348469933747,-1.165204139133,-1.317998400937));
#25352=CARTESIAN_POINT('Ctrl Pts',(-1.026867975908,-0.6516702524068,-1.374873400937));
#25353=CARTESIAN_POINT('Ctrl Pts',(-1.202679571961,0.180814804896,-1.431748400937));
#25354=CARTESIAN_POINT('Ctrl Pts',(-0.7898556864549,0.9248023542725,-1.488623400937));
#25355=CARTESIAN_POINT('Ctrl Pts',(0.009550993186476,1.216158607898,-1.545498400937));
#25356=CARTESIAN_POINT('Ctrl Pts',(0.8042879589087,0.9122802996697,-1.602373400937));
#25357=CARTESIAN_POINT('Ctrl Pts',(1.205358893105,0.161907415107,-1.659248400937));
#25358=CARTESIAN_POINT('Ctrl Pts',(1.016551442463,-0.6677408946503,-1.716123400937));
#25359=CARTESIAN_POINT('Ctrl Pts',(0.329952574922,-1.170452920957,-1.772998400937));
#25360=CARTESIAN_POINT('Ctrl Pts',(-0.2348081643589,-1.123983684464,-1.810915067604));
#25361=CARTESIAN_POINT('Ctrl Pts',(-0.4755900604755,-1.010680324589,-1.829873400937));
#25362=CARTESIAN_POINT('',(-2.15930259232053E-7,-1.11698671802919,-1.72115688661164));
#25363=CARTESIAN_POINT('Ctrl Pts',(0.740620592381851,0.835100532381467,
-0.0289497923354185));
#25364=CARTESIAN_POINT('Ctrl Pts',(0.796513037593552,0.78575378038458,-0.0342379290094453));
#25365=CARTESIAN_POINT('Ctrl Pts',(0.847573706129219,0.730904938153316,
-0.0395198235207524));
#25366=CARTESIAN_POINT('Ctrl Pts',(0.937932038832867,0.611387739176731,
-0.0501654329640508));
#25367=CARTESIAN_POINT('Ctrl Pts',(0.976471692706948,0.547333781599408,
-0.0554686789503681));
#25368=CARTESIAN_POINT('Ctrl Pts',(1.07054282678602,0.347984998632784,-0.0712031170738671));
#25369=CARTESIAN_POINT('Ctrl Pts',(1.10692249141229,0.203705684354229,-0.0816458765147045));
#25370=CARTESIAN_POINT('Ctrl Pts',(1.11904805235499,-0.0154853388500362,
-0.0972795741575819));
#25371=CARTESIAN_POINT('Ctrl Pts',(1.11588709227651,-0.0896747963869567,
-0.102518788484517));
#25372=CARTESIAN_POINT('Ctrl Pts',(1.08408659534245,-0.304356884899151,
-0.117921494634144));
#25373=CARTESIAN_POINT('Ctrl Pts',(1.03491689765162,-0.44140768856942,-0.128213717020561));
#25374=CARTESIAN_POINT('Ctrl Pts',(0.922288204707351,-0.633839472617977,
-0.144171751854915));
#25375=CARTESIAN_POINT('Ctrl Pts',(0.874557139837676,-0.698734383013323,
-0.149887101737748));
#25376=CARTESIAN_POINT('Ctrl Pts',(0.783538064083952,-0.797877565125105,
-0.15940176580863));
#25377=CARTESIAN_POINT('Ctrl Pts',(0.743769537021436,-0.835216308994231,
-0.16320369762073));
#25378=CARTESIAN_POINT('Ctrl Pts',(0.609333310871143,-0.943213119675615,
-0.175413924763073));
#25379=CARTESIAN_POINT('Ctrl Pts',(0.505701125475829,-1.00190544590687,
-0.183912879967629));
#25380=CARTESIAN_POINT('Ctrl Pts',(0.338835264532409,-1.06519787069243,
-0.196754094088973));
#25381=CARTESIAN_POINT('Ctrl Pts',(0.280161418331052,-1.08225571508646,
-0.201126888360145));
#25382=CARTESIAN_POINT('Ctrl Pts',(0.166767234429943,-1.1054758958236,-0.209363530411052));
#25383=CARTESIAN_POINT('Ctrl Pts',(0.112216529106593,-1.11255230532458,
-0.213229703934488));
#25384=CARTESIAN_POINT('Ctrl Pts',(0.0155582567028527,-1.1176927898296,
-0.219985145048376));
#25385=CARTESIAN_POINT('Ctrl Pts',(-0.0261352680459435,-1.11746162510164,
-0.222900761849483));
#25386=CARTESIAN_POINT('Ctrl Pts',(-0.177573634087521,-1.10788343875008,
-0.233664111859182));
#25387=CARTESIAN_POINT('Ctrl Pts',(-0.286247895212034,-1.08436597991008,
-0.24165713859263));
#25388=CARTESIAN_POINT('Ctrl Pts',(-0.450861460083075,-1.02313527330091,
-0.254340207177392));
#25389=CARTESIAN_POINT('Ctrl Pts',(-0.51049221102398,-0.994918085478592,
-0.259067571762949));
#25390=CARTESIAN_POINT('Ctrl Pts',(-0.611962301082644,-0.935521283217812,
-0.26739773754997));
#25391=CARTESIAN_POINT('Ctrl Pts',(-0.654909200479519,-0.906212039991709,
-0.271007441322454));
#25392=CARTESIAN_POINT('Ctrl Pts',(-0.720486485784318,-0.854171918393593,
-0.27681705109175));
#25393=CARTESIAN_POINT('Ctrl Pts',(-0.744409975919507,-0.833384416568187,
-0.279028283477932));
#25394=CARTESIAN_POINT('Ctrl Pts',(-0.797415126573322,-0.78306490151451,
-0.28419168642247));
#25395=CARTESIAN_POINT('Ctrl Pts',(-0.825746397084472,-0.752916952833451,
-0.287145498045552));
#25396=CARTESIAN_POINT('Ctrl Pts',(-0.906307501998842,-0.657079240397088,
-0.296161096764032));
#25397=CARTESIAN_POINT('Ctrl Pts',(-0.95309135752645,-0.586758490236072,
-0.302291570980455));
#25398=CARTESIAN_POINT('Ctrl Pts',(-1.01396989453065,-0.469115707118331,
-0.31187257893077));
#25399=CARTESIAN_POINT('Ctrl Pts',(-1.03355083743677,-0.424544687971698,
-0.315366605579132));
#25400=CARTESIAN_POINT('Ctrl Pts',(-1.0611465833909,-0.348799117113008,
-0.321085587964228));
#25401=CARTESIAN_POINT('Ctrl Pts',(-1.07083161179222,-0.318223021558651,
-0.323337980172478));
#25402=CARTESIAN_POINT('Ctrl Pts',(-1.09122343952725,-0.242564219693662,
-0.328779074897701));
#25403=CARTESIAN_POINT('Ctrl Pts',(-1.10048332412199,-0.197016748616113,
-0.331949207493977));
#25404=CARTESIAN_POINT('Ctrl Pts',(-1.110725571907,-0.121555091669843,-0.33727414443887));
#25405=CARTESIAN_POINT('Ctrl Pts',(-1.11349198406646,-0.0920543665529969,
-0.339368823000687));
#25406=CARTESIAN_POINT('Ctrl Pts',(-1.12012845133126,0.0327543760934407,
-0.348289261762931));
#25407=CARTESIAN_POINT('Ctrl Pts',(-1.1127994297416,0.128668562976753,-0.355293552486537));
#25408=CARTESIAN_POINT('Ctrl Pts',(-1.08655137401299,0.257792290211094,
-0.364878848852288));
#25409=CARTESIAN_POINT('Ctrl Pts',(-1.07759883804518,0.293116723581185,
-0.367517256533893));
#25410=CARTESIAN_POINT('Ctrl Pts',(-1.05805452229903,0.357178531877852,
-0.372327604097815));
#25411=CARTESIAN_POINT('Ctrl Pts',(-1.04795109721,0.386073149841699,-0.374507185489659));
#25412=CARTESIAN_POINT('Ctrl Pts',(-1.0175200545425,0.462895426666191,-0.380327548221617));
#25413=CARTESIAN_POINT('Ctrl Pts',(-0.994996800918248,0.509943087123585,
-0.383888402299322));
#25414=CARTESIAN_POINT('Ctrl Pts',(-0.957808633509514,0.575132092030043,
-0.389050136992139));
#25415=CARTESIAN_POINT('Ctrl Pts',(-0.945775473484694,0.594746751850922,
-0.390639417979559));
#25416=CARTESIAN_POINT('Ctrl Pts',(-0.918972123963961,0.635414431956283,
-0.394046456069751));
#25417=CARTESIAN_POINT('Ctrl Pts',(-0.904102140831624,0.656307674801286,
-0.395860186837375));
#25418=CARTESIAN_POINT('Ctrl Pts',(-0.864419170168452,0.708122030191015,
-0.400520097901616));
#25419=CARTESIAN_POINT('Ctrl Pts',(-0.838616852196583,0.738279114415411,
-0.403388573069705));
#25420=CARTESIAN_POINT('Ctrl Pts',(-0.766615948283921,0.81395937577478,
-0.410996633990166));
#25421=CARTESIAN_POINT('Ctrl Pts',(-0.717859140651418,0.857083532914942,
-0.415768526697806));
#25422=CARTESIAN_POINT('Ctrl Pts',(-0.642324639692028,0.913254617456444,
-0.422620821016675));
#25423=CARTESIAN_POINT('Ctrl Pts',(-0.618136110596605,0.929839550100437,
-0.424743759666412));
#25424=CARTESIAN_POINT('Ctrl Pts',(-0.571547575405974,0.959208007243405,
-0.428696605919632));
#25425=CARTESIAN_POINT('Ctrl Pts',(-0.549280650991451,0.972210891789697,
-0.430531230944641));
#25426=CARTESIAN_POINT('Ctrl Pts',(-0.501644505646967,0.99788130458919,
-0.434339845932671));
#25427=CARTESIAN_POINT('Ctrl Pts',(-0.476187622254524,1.01038588750128,
-0.436305190782293));
#25428=CARTESIAN_POINT('Ctrl Pts',(-0.406811798847217,1.04122235706574,
-0.441518550975112));
#25429=CARTESIAN_POINT('Ctrl Pts',(-0.362069063403444,1.0577586346472,-0.44474463696738));
#25430=CARTESIAN_POINT('Ctrl Pts',(-0.294776566884945,1.0776203242097,-0.449630402816247));
#25431=CARTESIAN_POINT('Ctrl Pts',(-0.272987925983213,1.08330968819,-0.451216618470544));
#25432=CARTESIAN_POINT('Ctrl Pts',(-0.223057022975575,1.09470834215462,
-0.454860393124103));
#25433=CARTESIAN_POINT('Ctrl Pts',(-0.194821349741637,1.09999085887876,
-0.456927201131256));
#25434=CARTESIAN_POINT('Ctrl Pts',(-0.0931781543481861,1.11496777184189,
-0.46438190893784));
#25435=CARTESIAN_POINT('Ctrl Pts',(-0.0188366922385358,1.11845687542912,
-0.469862803532103));
#25436=CARTESIAN_POINT('Ctrl Pts',(0.0943035999676855,1.11281577179903,
-0.478149447988595));
#25437=CARTESIAN_POINT('Ctrl Pts',(0.133409495312111,1.10884394569154,-0.481003024371444));
#25438=CARTESIAN_POINT('Ctrl Pts',(0.193849994240431,1.09953214938452,-0.485381356799469));
#25439=CARTESIAN_POINT('Ctrl Pts',(0.215403711020003,1.09557212007282,-0.486936282678626));
#25440=CARTESIAN_POINT('Ctrl Pts',(0.265430644698985,1.08486824357358,-0.490527020210655));
#25441=CARTESIAN_POINT('Ctrl Pts',(0.293797943223853,1.07763668945462,-0.492543598331562));
#25442=CARTESIAN_POINT('Ctrl Pts',(0.362926550960593,1.05707599620361,-0.497475075268599));
#25443=CARTESIAN_POINT('Ctrl Pts',(0.403299989728691,1.04247899272945,-0.500375401266443));
#25444=CARTESIAN_POINT('Ctrl Pts',(0.46237447012572,1.01703013432772,-0.50482221989358));
#25445=CARTESIAN_POINT('Ctrl Pts',(0.481763037883008,1.00797464499185,-0.50631873474349));
#25446=CARTESIAN_POINT('Ctrl Pts',(0.520940399942042,0.988240293911177,
-0.509423131274058));
#25447=CARTESIAN_POINT('Ctrl Pts',(0.540687957619948,0.977509607233441,
-0.511030894978789));
#25448=CARTESIAN_POINT('Ctrl Pts',(0.616055873729977,0.933519250921083,
-0.517328719525424));
#25449=CARTESIAN_POINT('Ctrl Pts',(0.669139138037821,0.895916512002932,
-0.52211865957522));
#25450=CARTESIAN_POINT('Ctrl Pts',(0.746534674753097,0.830544427725234,
-0.529584863943384));
#25451=CARTESIAN_POINT('Ctrl Pts',(0.773301769277264,0.805638507562068,
-0.532271589876185));
#25452=CARTESIAN_POINT('Ctrl Pts',(0.817732022702937,0.760144206774835,
-0.53690078853131));
#25453=CARTESIAN_POINT('Ctrl Pts',(0.835964059413658,0.740099905122851,
-0.538856517829673));
#25454=CARTESIAN_POINT('Ctrl Pts',(0.865813983208456,0.704835474509298,
-0.542151255585573));
#25455=CARTESIAN_POINT('Ctrl Pts',(0.877802803978707,0.689926363970315,
-0.543502813257041));
#25456=CARTESIAN_POINT('Ctrl Pts',(0.916735854119235,0.638912579792595,
-0.547986394647336));
#25457=CARTESIAN_POINT('Ctrl Pts',(0.941926713330494,0.601468666821261,
-0.5510414088158));
#25458=CARTESIAN_POINT('Ctrl Pts',(0.984605045342404,0.528772744682739,
-0.55677181495935));
#25459=CARTESIAN_POINT('Ctrl Pts',(1.00268914759296,0.493821064837415,-0.559449931570309));
#25460=CARTESIAN_POINT('Ctrl Pts',(1.02643518423323,0.440924121022262,-0.563510354774685));
#25461=CARTESIAN_POINT('Ctrl Pts',(1.03360688090292,0.423766066163042,-0.564827083396981));
#25462=CARTESIAN_POINT('Ctrl Pts',(1.04955405200274,0.382686262624412,-0.567976954224737));
#25463=CARTESIAN_POINT('Ctrl Pts',(1.05793864438942,0.358615900422101,-0.569820553652917));
#25464=CARTESIAN_POINT('Ctrl Pts',(1.08604334092431,0.268009456343316,-0.576741532772031));
#25465=CARTESIAN_POINT('Ctrl Pts',(1.10038794189382,0.199794477894304,-0.581916754293019));
#25466=CARTESIAN_POINT('Ctrl Pts',(1.11147624895963,0.105037384972042,-0.58893801844341));
#25467=CARTESIAN_POINT('Ctrl Pts',(1.11361798302232,0.0790931367382169,
-0.590843253297796));
#25468=CARTESIAN_POINT('Ctrl Pts',(1.11591391090523,0.031554393716092,-0.594293921700568));
#25469=CARTESIAN_POINT('Ctrl Pts',(1.11634499309645,0.00996997580722143,
-0.595845493874729));
#25470=CARTESIAN_POINT('Ctrl Pts',(1.11601678473683,-0.0289296677419575,
-0.598609699396986));
#25471=CARTESIAN_POINT('Ctrl Pts',(1.11547563051356,-0.046248246002881,
-0.599828705409154));
#25472=CARTESIAN_POINT('Ctrl Pts',(1.11033593676314,-0.141017182893811,
-0.606432256818337));
#25473=CARTESIAN_POINT('Ctrl Pts',(1.09817291136362,-0.218056107844839,
-0.611567396396193));
#25474=CARTESIAN_POINT('Ctrl Pts',(1.07317172150137,-0.310324277526315,
-0.6181942374858));
#25475=CARTESIAN_POINT('Ctrl Pts',(1.06803662014465,-0.327538716249082,
-0.619453491293131));
#25476=CARTESIAN_POINT('Ctrl Pts',(1.05655675853671,-0.362777251585735,
-0.622081615716259));
#25477=CARTESIAN_POINT('Ctrl Pts',(1.05016601531874,-0.380759737117483,
-0.623449716211376));
#25478=CARTESIAN_POINT('Ctrl Pts',(1.02910612085745,-0.43545019073186,-0.627688432807875));
#25479=CARTESIAN_POINT('Ctrl Pts',(1.0129078019094,-0.471564190764137,-0.630597635660525));
#25480=CARTESIAN_POINT('Ctrl Pts',(0.972516933914018,-0.550243442192709,
-0.637142859056502));
#25481=CARTESIAN_POINT('Ctrl Pts',(0.947333095146665,-0.592313600440566,
-0.640787985650376));
#25482=CARTESIAN_POINT('Ctrl Pts',(0.902593264720848,-0.657223094117165,
-0.646586869962779));
#25483=CARTESIAN_POINT('Ctrl Pts',(0.884646895429411,-0.681191198099769,
-0.648770402959629));
#25484=CARTESIAN_POINT('Ctrl Pts',(0.855043330245326,-0.717653674610126,
-0.652146488437597));
#25485=CARTESIAN_POINT('Ctrl Pts',(0.844000257524308,-0.730650131208104,
-0.65336144092369));
#25486=CARTESIAN_POINT('Ctrl Pts',(0.819356492875607,-0.758366983808924,
-0.65597513354726));
#25487=CARTESIAN_POINT('Ctrl Pts',(0.805647187522388,-0.772990003389014,
-0.657367195031824));
#25488=CARTESIAN_POINT('Ctrl Pts',(0.753852694203413,-0.825373614858682,
-0.662434857157094));
#25489=CARTESIAN_POINT('Ctrl Pts',(0.713431303888153,-0.860827044343055,
-0.666028251045876));
#25490=CARTESIAN_POINT('Ctrl Pts',(0.655237067121373,-0.904744358568907,
-0.671000732143755));
#25491=CARTESIAN_POINT('Ctrl Pts',(0.639543591515078,-0.915948263340018,
-0.672323771917992));
#25492=CARTESIAN_POINT('Ctrl Pts',(0.60962513922318,-0.93611487995497,-0.674829781695365));
#25493=CARTESIAN_POINT('Ctrl Pts',(0.595511643540952,-0.945152039884758,
-0.676006410644711));
#25494=CARTESIAN_POINT('Ctrl Pts',(0.565743394377794,-0.963244362873431,
-0.678480318310755));
#25495=CARTESIAN_POINT('Ctrl Pts',(0.550086783152038,-0.972229073801511,
-0.679776386992321));
#25496=CARTESIAN_POINT('Ctrl Pts',(0.468749092850581,-1.01626630305245,
-0.686476857345634));
#25497=CARTESIAN_POINT('Ctrl Pts',(0.399670594426793,-1.04501992354791,
-0.692064172993986));
#25498=CARTESIAN_POINT('Ctrl Pts',(0.303111884063254,-1.07454968136455,
-0.699548089161246));
#25499=CARTESIAN_POINT('Ctrl Pts',(0.277464427442118,-1.08142410479284,
-0.701505893230627));
#25500=CARTESIAN_POINT('Ctrl Pts',(0.23124017549895,-1.09210618607379,-0.704968192290077));
#25501=CARTESIAN_POINT('Ctrl Pts',(0.210739027718316,-1.09625570016186,
-0.706480952610665));
#25502=CARTESIAN_POINT('Ctrl Pts',(0.175084973374962,-1.10245927389464,
-0.709066607154982));
#25503=CARTESIAN_POINT('Ctrl Pts',(0.159976788452227,-1.10477692980497,
-0.71014815638368));
#25504=CARTESIAN_POINT('Ctrl Pts',(0.117068880774548,-1.11047804379366,
-0.713178529878514));
#25505=CARTESIAN_POINT('Ctrl Pts',(0.0891711334790336,-1.11314318565162,
-0.715102267228391));
#25506=CARTESIAN_POINT('Ctrl Pts',(0.0152811507985157,-1.11743175062111,
-0.720142872910414));
#25507=CARTESIAN_POINT('Ctrl Pts',(-0.0308137122952009,-1.11728414138088,
-0.723231670271439));
#25508=CARTESIAN_POINT('Ctrl Pts',(-0.0952192246255691,-1.11300919976543,
-0.72763937450432));
#25509=CARTESIAN_POINT('Ctrl Pts',(-0.113685215640747,-1.11131065463956,
-0.728913865262833));
#25510=CARTESIAN_POINT('Ctrl Pts',(-0.148023356154526,-1.10725480142821,
-0.731318768731457));
#25511=CARTESIAN_POINT('Ctrl Pts',(-0.163868256657507,-1.10502207506357,
-0.732443232159436));
#25512=CARTESIAN_POINT('Ctrl Pts',(-0.196621678780309,-1.0996540002806,
-0.734802925696262));
#25513=CARTESIAN_POINT('Ctrl Pts',(-0.213475544539095,-1.09647587733155,
-0.736035774793721));
#25514=CARTESIAN_POINT('Ctrl Pts',(-0.265221128464893,-1.08544898262041,
-0.739873197203898));
#25515=CARTESIAN_POINT('Ctrl Pts',(-0.299825399606563,-1.07627648889838,
-0.742513719077342));
#25516=CARTESIAN_POINT('Ctrl Pts',(-0.379743256694071,-1.05093994097453,
-0.748743352318556));
#25517=CARTESIAN_POINT('Ctrl Pts',(-0.424645943648842,-1.03345300238751,
-0.752346226165065));
#25518=CARTESIAN_POINT('Ctrl Pts',(-0.487214914516867,-1.00441802980982,
-0.75744306487192));
#25519=CARTESIAN_POINT('Ctrl Pts',(-0.505928609859782,-0.995101362044645,
-0.758977791885026));
#25520=CARTESIAN_POINT('Ctrl Pts',(-0.539953440105651,-0.976982756699067,
-0.761779872162063));
#25521=CARTESIAN_POINT('Ctrl Pts',(-0.555343172350867,-0.968324757444224,
-0.763051856284975));
#25522=CARTESIAN_POINT('Ctrl Pts',(-0.583668790471788,-0.951514077086158,
-0.765397339556922));
#25523=CARTESIAN_POINT('Ctrl Pts',(-0.596656575410486,-0.943449667964898,
-0.766473781057835));
#25524=CARTESIAN_POINT('Ctrl Pts',(-0.639460923839602,-0.915663473653058,
-0.770032511721639));
#25525=CARTESIAN_POINT('Ctrl Pts',(-0.668533444987986,-0.894786599671619,
-0.772469947624589));
#25526=CARTESIAN_POINT('Ctrl Pts',(-0.72803295391035,-0.847603619460765,
-0.777616303612912));
#25527=CARTESIAN_POINT('Ctrl Pts',(-0.758179997893041,-0.820945642382338,
-0.780321629381393));
#25528=CARTESIAN_POINT('Ctrl Pts',(-0.799468538679245,-0.780171380634711,
-0.784291725795911));
#25529=CARTESIAN_POINT('Ctrl Pts',(-0.811856990307968,-0.767323281669991,
-0.785521109365758));
#25530=CARTESIAN_POINT('Ctrl Pts',(-0.834363157369079,-0.742790458236818,
-0.787841049600906));
#25531=CARTESIAN_POINT('Ctrl Pts',(-0.844549838235625,-0.731194694447102,
-0.788927233214396));
#25532=CARTESIAN_POINT('Ctrl Pts',(-0.865180088529773,-0.706655790853523,
-0.791209916824488));
#25533=CARTESIAN_POINT('Ctrl Pts',(-0.875559603626039,-0.693711840905156,
-0.792404513977711));
#25534=CARTESIAN_POINT('Ctrl Pts',(-0.907300753515491,-0.652220064845121,
-0.796199979080816));
#25535=CARTESIAN_POINT('Ctrl Pts',(-0.927568629724395,-0.622842741494524,
-0.798838788211285));
#25536=CARTESIAN_POINT('Ctrl Pts',(-0.970743721155919,-0.55337615200648,
-0.804929873546265));
#25537=CARTESIAN_POINT('Ctrl Pts',(-0.992675550999678,-0.512673074309552,
-0.808393283270505));
#25538=CARTESIAN_POINT('Ctrl Pts',(-1.02358913443108,-0.445901531677113,
-0.813837743434644));
#25539=CARTESIAN_POINT('Ctrl Pts',(-1.03421911519682,-0.420583836526569,
-0.815850913095372));
#25540=CARTESIAN_POINT('Ctrl Pts',(-1.04914064218594,-0.381127643436842,
-0.818895300375298));
#25541=CARTESIAN_POINT('Ctrl Pts',(-1.05408962214885,-0.367235793244649,
-0.819949856985987));
#25542=CARTESIAN_POINT('Ctrl Pts',(-1.06457803559718,-0.335889589960992,
-0.82228820497776));
#25543=CARTESIAN_POINT('Ctrl Pts',(-1.06997115590549,-0.318385421864146,
-0.823566603718397));
#25544=CARTESIAN_POINT('Ctrl Pts',(-1.08406985225794,-0.26837260345258,
-0.827160118541158));
#25545=CARTESIAN_POINT('Ctrl Pts',(-1.09176652687607,-0.235575068707072,
-0.829446643500241));
#25546=CARTESIAN_POINT('Ctrl Pts',(-1.10501995603339,-0.164990729751102,
-0.834309246183183));
#25547=CARTESIAN_POINT('Ctrl Pts',(-1.11015166295162,-0.1271245486515,-0.836883249233791));
#25548=CARTESIAN_POINT('Ctrl Pts',(-1.11475710446898,-0.0714110531937625,
-0.840713226297503));
#25549=CARTESIAN_POINT('Ctrl Pts',(-1.11578889944405,-0.0536954246865552,
-0.841937373023348));
#25550=CARTESIAN_POINT('Ctrl Pts',(-1.11689520847532,-0.0207016552272614,
-0.844240747418634));
#25551=CARTESIAN_POINT('Ctrl Pts',(-1.1170830270095,-0.00542492262766989,
-0.845316790009298));
#25552=CARTESIAN_POINT('Ctrl Pts',(-1.11679315931087,0.0259477352854286,
-0.847553090895658));
#25553=CARTESIAN_POINT('Ctrl Pts',(-1.11628279693837,0.0420138989074261,
-0.848711802297192));
#25554=CARTESIAN_POINT('Ctrl Pts',(-1.11350619398124,0.093428780111666,
-0.852457326341894));
#25555=CARTESIAN_POINT('Ctrl Pts',(-1.1098659867498,0.128697038343365,-0.855083646008531));
#25556=CARTESIAN_POINT('Ctrl Pts',(-1.09788947947481,0.207695338285677,
-0.861044323243453));
#25557=CARTESIAN_POINT('Ctrl Pts',(-1.08858835282085,0.251284036045455,
-0.864387894854055));
#25558=CARTESIAN_POINT('Ctrl Pts',(-1.07162315027663,0.312878848488355,
-0.86912033721398));
#25559=CARTESIAN_POINT('Ctrl Pts',(-1.06599299429459,0.331452666862934,
-0.870548394892119));
#25560=CARTESIAN_POINT('Ctrl Pts',(-1.05476115668701,0.36537170990575,-0.873150600962024));
#25561=CARTESIAN_POINT('Ctrl Pts',(-1.0492958810119,0.380763467942627,-0.874329224331263));
#25562=CARTESIAN_POINT('Ctrl Pts',(-1.03800209829953,0.410533289165098,
-0.876600004545797));
#25563=CARTESIAN_POINT('Ctrl Pts',(-1.03220529608311,0.424924244767954,
-0.877693579640065));
#25564=CARTESIAN_POINT('Ctrl Pts',(-1.0114859159707,0.473484785214209,-0.881381794545307));
#25565=CARTESIAN_POINT('Ctrl Pts',(-0.995172662031445,0.507068747093084,
-0.88392887766051));
#25566=CARTESIAN_POINT('Ctrl Pts',(-0.945776378317264,0.59713296989077,
-0.89089990504806));
#25567=CARTESIAN_POINT('Ctrl Pts',(-0.90932877506683,0.651764236978487,
-0.895290318042283));
#25568=CARTESIAN_POINT('Ctrl Pts',(-0.85887825736663,0.714279352173068,
-0.900913351112112));
#25569=CARTESIAN_POINT('Ctrl Pts',(-0.84926873031843,0.725694991316666,
-0.901967408221818));
#25570=CARTESIAN_POINT('Ctrl Pts',(-0.828644309581112,0.749175524787077,
-0.904201003827353));
#25571=CARTESIAN_POINT('Ctrl Pts',(-0.817598489920929,0.761185321982524,
-0.905380784671543));
#25572=CARTESIAN_POINT('Ctrl Pts',(-0.793001387353391,0.786747534130122,
-0.907969371515655));
#25573=CARTESIAN_POINT('Ctrl Pts',(-0.779350493374864,0.800201952292473,
-0.90938208413594));
#25574=CARTESIAN_POINT('Ctrl Pts',(-0.734309167703067,0.842336807487848,
-0.9139580448811));
#25575=CARTESIAN_POINT('Ctrl Pts',(-0.70157997556205,0.869583934989602,
-0.917156130140118));
#25576=CARTESIAN_POINT('Ctrl Pts',(-0.639540477712964,0.915572785812997,
-0.922923184444654));
#25577=CARTESIAN_POINT('Ctrl Pts',(-0.610699011937772,0.934962526109273,
-0.925500197814225));
#25578=CARTESIAN_POINT('Ctrl Pts',(-0.567867741709528,0.9610074883144,-0.929146335576841));
#25579=CARTESIAN_POINT('Ctrl Pts',(-0.554536053336679,0.968749290570932,
-0.93025697426775));
#25580=CARTESIAN_POINT('Ctrl Pts',(-0.526474100248925,0.984295490819199,
-0.932542356286181));
#25581=CARTESIAN_POINT('Ctrl Pts',(-0.51171875207078,0.992053651878127,
-0.933715811422599));
#25582=CARTESIAN_POINT('Ctrl Pts',(-0.452990224509344,1.02131160693359,
-0.938293251144693));
#25583=CARTESIAN_POINT('Ctrl Pts',(-0.407765306240264,1.04033046095139,
-0.94161551976887));
#25584=CARTESIAN_POINT('Ctrl Pts',(-0.313037828080522,1.07308588823884,
-0.948410367454849));
#25585=CARTESIAN_POINT('Ctrl Pts',(-0.263433120774754,1.08652867895733,
-0.951883688628962));
#25586=CARTESIAN_POINT('Ctrl Pts',(-0.196979328012632,1.09957757647535,
-0.95661022891241));
#25587=CARTESIAN_POINT('Ctrl Pts',(-0.180765877016589,1.10238007628764,
-0.957769039559126));
#25588=CARTESIAN_POINT('Ctrl Pts',(-0.149645727930048,1.10702287798097,
-0.960012463254124));
#25589=CARTESIAN_POINT('Ctrl Pts',(-0.134770806361007,1.10892162563533,
-0.961093677413286));
#25590=CARTESIAN_POINT('Ctrl Pts',(-0.0820732731622451,1.11453682573504,
-0.964950381477751));
#25591=CARTESIAN_POINT('Ctrl Pts',(-0.0440722367273357,1.11656706895916,
-0.967779000956304));
#25592=CARTESIAN_POINT('Ctrl Pts',(0.0540305524033847,1.11677795949199,
-0.975117906286598));
#25593=CARTESIAN_POINT('Ctrl Pts',(0.114151155725786,1.11203507507255,-0.97965010173671));
#25594=CARTESIAN_POINT('Ctrl Pts',(0.188467982153772,1.100231277558,-0.985115587025778));
#25595=CARTESIAN_POINT('Ctrl Pts',(0.203374403245894,1.09755874827963,-0.986204153414178));
#25596=CARTESIAN_POINT('Ctrl Pts',(0.236063821038359,1.0910256528619,-0.988575982945092));
#25597=CARTESIAN_POINT('Ctrl Pts',(0.253821207080709,1.08703416613913,-0.9898550669114));
#25598=CARTESIAN_POINT('Ctrl Pts',(0.292298236793962,1.07741543574307,-0.992617716620507));
#25599=CARTESIAN_POINT('Ctrl Pts',(0.312978265295055,1.07162275221265,-0.994096826484634));
#25600=CARTESIAN_POINT('Ctrl Pts',(0.380956088887678,1.05049225879604,-0.998970509474916));
#25601=CARTESIAN_POINT('Ctrl Pts',(0.427476292869596,1.03262248510317,-1.00232444355582));
#25602=CARTESIAN_POINT('Ctrl Pts',(0.501777055710514,0.998212465206567,
-1.00791521430462));
#25603=CARTESIAN_POINT('Ctrl Pts',(0.53037224227781,0.983431809674303,-1.01012838908167));
#25604=CARTESIAN_POINT('Ctrl Pts',(0.572130309905694,0.959439684514594,
-1.01350534028038));
#25605=CARTESIAN_POINT('Ctrl Pts',(0.585826681947766,0.951162253494843,
-1.01463753009962));
#25606=CARTESIAN_POINT('Ctrl Pts',(0.612866734630896,0.933981118440412,
-1.0169308333167));
#25607=CARTESIAN_POINT('Ctrl Pts',(0.626186752566185,0.925089263853542,
-1.01809082693388));
#25608=CARTESIAN_POINT('Ctrl Pts',(0.654913887564356,0.904976207517935,
-1.02065482724021));
#25609=CARTESIAN_POINT('Ctrl Pts',(0.670241222410078,0.893628769797773,
-1.02206364946472));
#25610=CARTESIAN_POINT('Ctrl Pts',(0.721352459819767,0.853686784337798,
-1.0268863553142));
#25611=CARTESIAN_POINT('Ctrl Pts',(0.755674530592387,0.823225962826674,
-1.03034125113025));
#25612=CARTESIAN_POINT('Ctrl Pts',(0.807305122531451,0.771469794764212,
-1.03578513225715));
#25613=CARTESIAN_POINT('Ctrl Pts',(0.825889378543328,0.751438631054798,
-1.0378027422642));
#25614=CARTESIAN_POINT('Ctrl Pts',(0.85390525146924,0.718978765547925,-1.04091515493341));
#25615=CARTESIAN_POINT('Ctrl Pts',(0.863838296471794,0.706982031588233,
-1.04203324901225));
#25616=CARTESIAN_POINT('Ctrl Pts',(0.885842337257275,0.679273374591332,
-1.04454926651593));
#25617=CARTESIAN_POINT('Ctrl Pts',(0.897760308848472,0.663437812855681,
-1.04594089912198));
#25618=CARTESIAN_POINT('Ctrl Pts',(0.940529854645035,0.603426561316026,
-1.05107021135596));
#25619=CARTESIAN_POINT('Ctrl Pts',(0.968711315983671,0.557325272017379,
-1.05472760903283));
#25620=CARTESIAN_POINT('Ctrl Pts',(1.01459496700254,0.468543805603866,-1.06153069346646));
#25621=CARTESIAN_POINT('Ctrl Pts',(1.03322667884151,0.426336847146873,-1.06467456745001));
#25622=CARTESIAN_POINT('Ctrl Pts',(1.05530418605042,0.366318476561309,-1.0691470158903));
#25623=CARTESIAN_POINT('Ctrl Pts',(1.06107083620922,0.349365124742118,-1.07041052359689));
#25624=CARTESIAN_POINT('Ctrl Pts',(1.07103108937878,0.317492082608692,-1.07279569358009));
#25625=CARTESIAN_POINT('Ctrl Pts',(1.07531873931894,0.302647697696071,-1.07391112223302));
#25626=CARTESIAN_POINT('Ctrl Pts',(1.08372674491576,0.270983199444743,-1.07630039051983));
#25627=CARTESIAN_POINT('Ctrl Pts',(1.08775815030352,0.254178484810853,-1.07757346606282));
#25628=CARTESIAN_POINT('Ctrl Pts',(1.09920672432866,0.200911767862958,-1.08161386784057));
#25629=CARTESIAN_POINT('Ctrl Pts',(1.10516405878848,0.164140051615529,-1.08441071192921));
#25630=CARTESIAN_POINT('Ctrl Pts',(1.11313632206713,0.0925116321749409,
-1.08980025738597));
#25631=CARTESIAN_POINT('Ctrl Pts',(1.11537610008911,0.0576750688941246,
-1.09239483580262));
#25632=CARTESIAN_POINT('Ctrl Pts',(1.11631613577469,0.00624209603872625,
-1.09613888125271));
#25633=CARTESIAN_POINT('Ctrl Pts',(1.11625709653239,-0.0103330825248156,
-1.09733154747569));
#25634=CARTESIAN_POINT('Ctrl Pts',(1.11532332434456,-0.0472093011195721,
-1.09996059458416));
#25635=CARTESIAN_POINT('Ctrl Pts',(1.11426722420198,-0.067507546287733,
-1.10139141621481));
#25636=CARTESIAN_POINT('Ctrl Pts',(1.10868779994077,-0.138334923954908,
-1.10634987545962));
#25637=CARTESIAN_POINT('Ctrl Pts',(1.10133962030423,-0.188658275579207,
-1.10981111643529));
#25638=CARTESIAN_POINT('Ctrl Pts',(1.07959814478269,-0.289583901889022,
-1.1168539594144));
#25639=CARTESIAN_POINT('Ctrl Pts',(1.0649653301397,-0.340143841151782,-1.12043711273469));
#25640=CARTESIAN_POINT('Ctrl Pts',(1.0402539432014,-0.407092951957314,-1.12543456230341));
#25641=CARTESIAN_POINT('Ctrl Pts',(1.03326497189092,-0.424618550531358,
-1.12676739376517));
#25642=CARTESIAN_POINT('Ctrl Pts',(1.01941815551277,-0.45685260978153,-1.12927609230871));
#25643=CARTESIAN_POINT('Ctrl Pts',(1.01269198621406,-0.471581615429797,
-1.1304460690027));
#25644=CARTESIAN_POINT('Ctrl Pts',(0.989163829256111,-0.520147742837765,
-1.13438713833658));
#25645=CARTESIAN_POINT('Ctrl Pts',(0.970928209393707,-0.553228690762047,
-1.13720375937833));
#25646=CARTESIAN_POINT('Ctrl Pts',(0.92597884305988,-0.625749700867753,
-1.14358686699613));
#25647=CARTESIAN_POINT('Ctrl Pts',(0.898294594044716,-0.664591024295858,
-1.14715621217329));
#25648=CARTESIAN_POINT('Ctrl Pts',(0.857069697743663,-0.715361386315322,
-1.15191194064786));
#25649=CARTESIAN_POINT('Ctrl Pts',(0.845526245963272,-0.728914240577514,
-1.1531915450963));
#25650=CARTESIAN_POINT('Ctrl Pts',(0.818491764529182,-0.759191099177518,
-1.15608212328668));
#25651=CARTESIAN_POINT('Ctrl Pts',(0.802800657412089,-0.775739281332732,
-1.15768545012032));
#25652=CARTESIAN_POINT('Ctrl Pts',(0.76681968081965,-0.81148398151618,-1.16122157447671));
#25653=CARTESIAN_POINT('Ctrl Pts',(0.746286813137865,-0.830441180245557,
-1.16314758176595));
#25654=CARTESIAN_POINT('Ctrl Pts',(0.676991009179002,-0.889859141557608,
-1.16941324396116));
#25655=CARTESIAN_POINT('Ctrl Pts',(0.625446039688801,-0.927101619168428,
-1.17371624456519));
#25656=CARTESIAN_POINT('Ctrl Pts',(0.550169183105251,-0.972217481367136,
-1.17981804356229));
#25657=CARTESIAN_POINT('Ctrl Pts',(0.528818209110273,-0.984071076769615,
-1.18153021990509));
#25658=CARTESIAN_POINT('Ctrl Pts',(0.491984019956504,-1.00292332829553,
-1.18447220874538));
#25659=CARTESIAN_POINT('Ctrl Pts',(0.476696605684069,-1.01029998662431,
-1.18568991475916));
#25660=CARTESIAN_POINT('Ctrl Pts',(0.434145987134609,-1.0295958956179,-1.18908007359259));
#25661=CARTESIAN_POINT('Ctrl Pts',(0.406553200265277,-1.04074219244302,
-1.1912802804877));
#25662=CARTESIAN_POINT('Ctrl Pts',(0.333153415825322,-1.0669721778709,-1.1970858745644));
#25663=CARTESIAN_POINT('Ctrl Pts',(0.286674562829502,-1.08019795380544,
-1.20071533118248));
#25664=CARTESIAN_POINT('Ctrl Pts',(0.21977038433892,-1.09468524172238,-1.20574155087924));
#25665=CARTESIAN_POINT('Ctrl Pts',(0.199882874314479,-1.09843535550142,
-1.20720964347452));
#25666=CARTESIAN_POINT('Ctrl Pts',(0.158677184619967,-1.10507314265271,
-1.21020500880998));
#25667=CARTESIAN_POINT('Ctrl Pts',(0.137346315536213,-1.10789183987108,
-1.2117309138464));
#25668=CARTESIAN_POINT('Ctrl Pts',(0.0578253119596095,-1.11612516676388,
-1.21735301767836));
#25669=CARTESIAN_POINT('Ctrl Pts',(-0.0007897928477788,-1.11768935041499,
-1.22136509379683));
#25670=CARTESIAN_POINT('Ctrl Pts',(-0.11387500185164,-1.11198216449286,
-1.22913593826288));
#25671=CARTESIAN_POINT('Ctrl Pts',(-0.168393309681907,-1.10525704406103,
-1.23289715332687));
#25672=CARTESIAN_POINT('Ctrl Pts',(-0.242946202835828,-1.09034635843923,
-1.23824110058869));
#25673=CARTESIAN_POINT('Ctrl Pts',(-0.263661929028808,-1.08557424900894,
-1.23974792877966));
#25674=CARTESIAN_POINT('Ctrl Pts',(-0.302633547942523,-1.07537644070583,
-1.24263828990327));
#25675=CARTESIAN_POINT('Ctrl Pts',(-0.320895999817841,-1.0700772135446,
-1.24401724454367));
#25676=CARTESIAN_POINT('Ctrl Pts',(-0.388834444137772,-1.04837547248558,
-1.24924765976264));
#25677=CARTESIAN_POINT('Ctrl Pts',(-0.437431167749803,-1.02884834375456,
-1.25318179381202));
#25678=CARTESIAN_POINT('Ctrl Pts',(-0.508504613606336,-0.994333314151419,
-1.25903686345293));
#25679=CARTESIAN_POINT('Ctrl Pts',(-0.532158147116165,-0.981778355513795,
-1.26100023317393));
#25680=CARTESIAN_POINT('Ctrl Pts',(-0.574563300398608,-0.957307601219113,
-1.26453681636663));
#25681=CARTESIAN_POINT('Ctrl Pts',(-0.593461718938977,-0.945649094933868,
-1.2661219664867));
#25682=CARTESIAN_POINT('Ctrl Pts',(-0.644375275958978,-0.912151809271095,
-1.27043545555292));
#25683=CARTESIAN_POINT('Ctrl Pts',(-0.675668764426734,-0.889200370193944,
-1.27313514232132));
#25684=CARTESIAN_POINT('Ctrl Pts',(-0.760437520387496,-0.820144561142635,
-1.28069894045784));
#25685=CARTESIAN_POINT('Ctrl Pts',(-0.811055261632599,-0.770478713171644,
-1.28552266871189));
#25686=CARTESIAN_POINT('Ctrl Pts',(-0.874484451983752,-0.695153715383073,
-1.29239831682034));
#25687=CARTESIAN_POINT('Ctrl Pts',(-0.891646638926817,-0.673141212799298,
-1.29436235324845));
#25688=CARTESIAN_POINT('Ctrl Pts',(-0.919703712778341,-0.634150658299314,
-1.29778966744056));
#25689=CARTESIAN_POINT('Ctrl Pts',(-0.931013634384034,-0.617474950131453,
-1.29924029044429));
#25690=CARTESIAN_POINT('Ctrl Pts',(-0.951725734380025,-0.5849959600492,
-1.30204658206248));
#25691=CARTESIAN_POINT('Ctrl Pts',(-0.961201202874254,-0.569253958823924,
-1.30339893752634));
#25692=CARTESIAN_POINT('Ctrl Pts',(-0.994270057819556,-0.511019147880041,
-1.30835525083632));
#25693=CARTESIAN_POINT('Ctrl Pts',(-1.01542620382818,-0.467142941382244,
-1.31200158069852));
#25694=CARTESIAN_POINT('Ctrl Pts',(-1.04266204202624,-0.399818094214572,
-1.31731455804578));
#25695=CARTESIAN_POINT('Ctrl Pts',(-1.05095349258127,-0.37726796591669,
-1.31905021897796));
#25696=CARTESIAN_POINT('Ctrl Pts',(-1.06783378208471,-0.326436173938074,
-1.32288298987987));
#25697=CARTESIAN_POINT('Ctrl Pts',(-1.07605213671493,-0.29802774751781,
-1.32497147091931));
#25698=CARTESIAN_POINT('Ctrl Pts',(-1.09205113087124,-0.233450144132,-1.32963463265107));
#25699=CARTESIAN_POINT('Ctrl Pts',(-1.09920426871889,-0.197116915666788,
-1.33220014807258));
#25700=CARTESIAN_POINT('Ctrl Pts',(-1.11569139976872,-0.0848645490057636,
-1.34004888630328));
#25701=CARTESIAN_POINT('Ctrl Pts',(-1.11920391951796,-0.00806009617995092,
-1.34531246542237));
#25702=CARTESIAN_POINT('Ctrl Pts',(-1.11335269071756,0.0920233385725479,
-1.35241704957437));
#25703=CARTESIAN_POINT('Ctrl Pts',(-1.11119224195733,0.11572547805626,-1.35411777718821));
#25704=CARTESIAN_POINT('Ctrl Pts',(-1.10354318058673,0.177071879490257,
-1.35858901706502));
#25705=CARTESIAN_POINT('Ctrl Pts',(-1.0968474758073,0.214367326080166,-1.3613874522399));
#25706=CARTESIAN_POINT('Ctrl Pts',(-1.07873998266251,0.291897496557865,
-1.36728850096717));
#25707=CARTESIAN_POINT('Ctrl Pts',(-1.06690821471463,0.332037830586118,
-1.3703797243111));
#25708=CARTESIAN_POINT('Ctrl Pts',(-1.04332152760018,0.398232326867899,
-1.3754649079695));
#25709=CARTESIAN_POINT('Ctrl Pts',(-1.03274322803085,0.424698782517065,
-1.37750185784614));
#25710=CARTESIAN_POINT('Ctrl Pts',(-0.995494040347185,0.508618254227233,
-1.38401007855805));
#25711=CARTESIAN_POINT('Ctrl Pts',(-0.964956834095852,0.564390205958779,
-1.38841147648662));
#25712=CARTESIAN_POINT('Ctrl Pts',(-0.892967481706339,0.673298566929881,
-1.39747097352407));
#25713=CARTESIAN_POINT('Ctrl Pts',(-0.850937651780783,0.72610268365452,
-1.4021329463705));
#25714=CARTESIAN_POINT('Ctrl Pts',(-0.785667057548767,0.794283450457149,
-1.40882615327226));
#25715=CARTESIAN_POINT('Ctrl Pts',(-0.766143934832389,0.81322073125236,
-1.41077052091126));
#25716=CARTESIAN_POINT('Ctrl Pts',(-0.720375161308584,0.854369873452665,
-1.41522533430838));
#25717=CARTESIAN_POINT('Ctrl Pts',(-0.693838948060834,0.876001260804895,
-1.41774575192641));
#25718=CARTESIAN_POINT('Ctrl Pts',(-0.633258156945879,0.920815597145715,
-1.42330892229183));
#25719=CARTESIAN_POINT('Ctrl Pts',(-0.59879921827957,0.943411854228772,
-1.4263360361838));
#25720=CARTESIAN_POINT('Ctrl Pts',(-0.533064199397785,0.981527990020711,
-1.43182303736665));
#25721=CARTESIAN_POINT('Ctrl Pts',(-0.50211333730462,0.997600684576518,
-1.43430816934474));
#25722=CARTESIAN_POINT('Ctrl Pts',(-0.43346420760776,1.02934490598123,-1.43965775086329));
#25723=CARTESIAN_POINT('Ctrl Pts',(-0.395507335393598,1.04448215382306,
-1.44251517581157));
#25724=CARTESIAN_POINT('Ctrl Pts',(-0.26711867659718,1.08788950411197,-1.45197329338261));
#25725=CARTESIAN_POINT('Ctrl Pts',(-0.173552851448838,1.1071011125986,-1.45853692012621));
#25726=CARTESIAN_POINT('Ctrl Pts',(-0.0491969920609825,1.11625444550779,
-1.46743850887193));
#25727=CARTESIAN_POINT('Ctrl Pts',(-0.0192027323245962,1.11722754308489,
-1.46959886421849));
#25728=CARTESIAN_POINT('Ctrl Pts',(0.0390259210125597,1.11665977811538,
-1.47384454681893));
#25729=CARTESIAN_POINT('Ctrl Pts',(0.0672398127568702,1.11526531437875,
-1.47592461460744));
#25730=CARTESIAN_POINT('Ctrl Pts',(0.13566487510423,1.1092240533465,-1.48096698326874));
#25731=CARTESIAN_POINT('Ctrl Pts',(0.175770475157463,1.10343054811916,-1.48390680342966));
#25732=CARTESIAN_POINT('Ctrl Pts',(0.267046634661586,1.08517574510875,-1.49058741766001));
#25733=CARTESIAN_POINT('Ctrl Pts',(0.317931688778372,1.07123280478388,-1.49431106263498));
#25734=CARTESIAN_POINT('Ctrl Pts',(0.446961994983713,1.02612044323732,-1.50391787545689));
#25735=CARTESIAN_POINT('Ctrl Pts',(0.523316979042064,0.989605242025754,
-1.50976888528809));
#25736=CARTESIAN_POINT('Ctrl Pts',(0.632908523567412,0.921159089521382,
-1.51888437332726));
#25737=CARTESIAN_POINT('Ctrl Pts',(0.669748303379762,0.894927711381821,
-1.52209312747034));
#25738=CARTESIAN_POINT('Ctrl Pts',(0.730610405353075,0.845580443854341,
-1.52773785069793));
#25739=CARTESIAN_POINT('Ctrl Pts',(0.7552881057523,0.823599046260279,-1.5301467049352));
#25740=CARTESIAN_POINT('Ctrl Pts',(0.817218965948864,0.763098843103266,
-1.53647429966056));
#25741=CARTESIAN_POINT('Ctrl Pts',(0.852662889830548,0.722959726302608,
-1.54034188256599));
#25742=CARTESIAN_POINT('Ctrl Pts',(0.938211054001444,0.610963635981032,
-1.55041907671587));
#25743=CARTESIAN_POINT('Ctrl Pts',(0.983263737595165,0.535174401068512,
-1.55657154136733));
#25744=CARTESIAN_POINT('Ctrl Pts',(1.05355565231594,0.378547858674659,-1.56863732896307));
#25745=CARTESIAN_POINT('Ctrl Pts',(1.07952855842687,0.297931382092672,-1.5745601387804));
#25746=CARTESIAN_POINT('Ctrl Pts',(1.1050362391125,0.169640335255523,-1.58393561109276));
#25747=CARTESIAN_POINT('Ctrl Pts',(1.11111365921164,0.123684939102018,-1.58730302707212));
#25748=CARTESIAN_POINT('Ctrl Pts',(1.11964636245312,-0.00367233478476775,
-1.59655127403001));
#25749=CARTESIAN_POINT('Ctrl Pts',(1.11605101611499,-0.085101664783812,
-1.60233845571577));
#25750=CARTESIAN_POINT('Ctrl Pts',(1.0816505606552,-0.312274176175625,-1.61862620449722));
#25751=CARTESIAN_POINT('Ctrl Pts',(1.03056423362021,-0.45524871230428,-1.62905386459966));
#25752=CARTESIAN_POINT('Ctrl Pts',(0.922586007371914,-0.632513575792815,
-1.64395355031118));
#25753=CARTESIAN_POINT('Ctrl Pts',(0.888040527122837,-0.679871542158833,
-1.64818318901711));
#25754=CARTESIAN_POINT('Ctrl Pts',(0.764236840703511,-0.824202940541874,
-1.66181556537727));
#25755=CARTESIAN_POINT('Ctrl Pts',(0.660519067741824,-0.909040197336868,
-1.67115934543248));
#25756=CARTESIAN_POINT('Ctrl Pts',(0.463560083860833,-1.02011807088014,
-1.68719358718629));
#25757=CARTESIAN_POINT('Ctrl Pts',(0.375334948218811,-1.05637112684073,
-1.69392081615549));
#25758=CARTESIAN_POINT('Ctrl Pts',(0.191017799332561,-1.10461528968122,
-1.70755628210277));
#25759=CARTESIAN_POINT('Ctrl Pts',(0.0954959843605988,-1.1164612562587,
-1.71438524122992));
#25760=CARTESIAN_POINT('Ctrl Pts',(4.85215486032485E-6,-1.11628565924263,
-1.72119948076935));
#25761=CARTESIAN_POINT('',(3.48982020092455E-10,-1.11698717731251,-1.77886751164369));
#25762=CARTESIAN_POINT('',(0.,-1.116987298108,-1.721132486541));
#25763=CARTESIAN_POINT('Ctrl Pts',(-4.51646176117242E-5,1.11628556616826,
-0.028845753490975));
#25764=CARTESIAN_POINT('Ctrl Pts',(0.0945737663334262,1.11646371878452,
-0.0355870386379063));
#25765=CARTESIAN_POINT('Ctrl Pts',(0.189224370129108,1.10483896102052,-0.0423343546232623));
#25766=CARTESIAN_POINT('Ctrl Pts',(0.372906704517377,1.05724696582637,-0.0558777394065449));
#25767=CARTESIAN_POINT('Ctrl Pts',(0.461252181102166,1.02117700224735,-0.062629461743586));
#25768=CARTESIAN_POINT('Ctrl Pts',(0.668471432388766,0.904915646636026,
-0.0795557664982609));
#25769=CARTESIAN_POINT('Ctrl Pts',(0.780383055419209,0.811029500761427,
-0.0897649811840648));
#25770=CARTESIAN_POINT('Ctrl Pts',(0.977352549963107,0.567498199932401,
-0.112102790001303));
#25771=CARTESIAN_POINT('Ctrl Pts',(1.03703915589554,0.43114576827777,-0.122493806927422));
#25772=CARTESIAN_POINT('Ctrl Pts',(1.11066616674449,0.178042375581358,-0.141264319305712));
#25773=CARTESIAN_POINT('Ctrl Pts',(1.1250370353998,0.0352369170927906,-0.151306365748182));
#25774=CARTESIAN_POINT('Ctrl Pts',(1.09418460733438,-0.296790717289766,
-0.175096927046621));
#25775=CARTESIAN_POINT('Ctrl Pts',(1.02997735713433,-0.440477084842064,
-0.186018843166476));
#25776=CARTESIAN_POINT('Ctrl Pts',(0.925588908242817,-0.636392952388509,
-0.201824931705356));
#25777=CARTESIAN_POINT('Ctrl Pts',(0.840538191683154,-0.751460714065254,
-0.211837015280091));
#25778=CARTESIAN_POINT('Ctrl Pts',(0.611182247799738,-0.946513834085736,
-0.233319769585066));
#25779=CARTESIAN_POINT('Ctrl Pts',(0.478234529751117,-1.0191711099922,-0.243900801774971));
#25780=CARTESIAN_POINT('Ctrl Pts',(0.222597234321242,-1.1004636264182,-0.263002748092197));
#25781=CARTESIAN_POINT('Ctrl Pts',(0.0794663775051929,-1.12675755955542,
-0.273170746756787));
#25782=CARTESIAN_POINT('Ctrl Pts',(-0.232981315456763,-1.10176800386665,
-0.295527565272568));
#25783=CARTESIAN_POINT('Ctrl Pts',(-0.377700605109014,-1.06037143957915,
-0.306036970274604));
#25784=CARTESIAN_POINT('Ctrl Pts',(-0.604852724324526,-0.944731736167623,
-0.324194405506215));
#25785=CARTESIAN_POINT('Ctrl Pts',(-0.731331226988448,-0.863974006299954,
-0.33465639462854));
#25786=CARTESIAN_POINT('Ctrl Pts',(-0.943397907937856,-0.613934547621999,
-0.358026630171605));
#25787=CARTESIAN_POINT('Ctrl Pts',(-1.01607631574406,-0.484189787750187,
-0.368412151890716));
#25788=CARTESIAN_POINT('Ctrl Pts',(-1.11857306467121,-0.173002860562976,
-0.391764370126267));
#25789=CARTESIAN_POINT('Ctrl Pts',(-1.12165266273671,-0.0230529286473884,
-0.402222387376179));
#25790=CARTESIAN_POINT('Ctrl Pts',(-1.10179845703878,0.228016486144736,
-0.420164306092339));
#25791=CARTESIAN_POINT('Ctrl Pts',(-1.06324590215937,0.369253565391365,
-0.430395833792596));
#25792=CARTESIAN_POINT('Ctrl Pts',(-0.924464855646202,0.649976757040026,
-0.452728617062329));
#25793=CARTESIAN_POINT('Ctrl Pts',(-0.825915661788618,0.761161572818576,
-0.46310258159148));
#25794=CARTESIAN_POINT('Ctrl Pts',(-0.62621431634986,0.934430304671199,
-0.481930408255844));
#25795=CARTESIAN_POINT('Ctrl Pts',(-0.502214996937546,1.00732385711169,
-0.491992988167886));
#25796=CARTESIAN_POINT('Ctrl Pts',(-0.191201997533733,1.11682300306852,
-0.51551693664123));
#25797=CARTESIAN_POINT('Ctrl Pts',(-0.0349012702549832,1.12007370080308,
-0.526380158581428));
#25798=CARTESIAN_POINT('Ctrl Pts',(0.203851405860733,1.1061171885703,-0.543408695580735));
#25799=CARTESIAN_POINT('Ctrl Pts',(0.341786112597022,1.07261170247852,-0.553349115596787));
#25800=CARTESIAN_POINT('Ctrl Pts',(0.603413551668518,0.95156305246285,-0.573918159961364));
#25801=CARTESIAN_POINT('Ctrl Pts',(0.725113385898939,0.861211673415832,
-0.584504519828558));
#25802=CARTESIAN_POINT('Ctrl Pts',(0.905273423514477,0.663857977873337,
-0.603532452081928));
#25803=CARTESIAN_POINT('Ctrl Pts',(0.989304020610892,0.545163021076612,
-0.613692540952363));
#25804=CARTESIAN_POINT('Ctrl Pts',(1.09791444748826,0.250846118613206,-0.636070285825294));
#25805=CARTESIAN_POINT('Ctrl Pts',(1.12102369397598,0.101931202388124,-0.646591923275123));
#25806=CARTESIAN_POINT('Ctrl Pts',(1.11127472608704,-0.152382998725974,
-0.664720299224974));
#25807=CARTESIAN_POINT('Ctrl Pts',(1.09120934524513,-0.300938815206498,
-0.67517036237632));
#25808=CARTESIAN_POINT('Ctrl Pts',(0.953355092950195,-0.598483057720638,
-0.698547434541527));
#25809=CARTESIAN_POINT('Ctrl Pts',(0.865889506205134,-0.71909663240587,
-0.708951545171134));
#25810=CARTESIAN_POINT('Ctrl Pts',(0.630908211369362,-0.938430669099252,
-0.731860596310233));
#25811=CARTESIAN_POINT('Ctrl Pts',(0.499473987912849,-1.00559671816685,
-0.742165965145054));
#25812=CARTESIAN_POINT('Ctrl Pts',(0.254954649474663,-1.09592824110064,
-0.760737340530769));
#25813=CARTESIAN_POINT('Ctrl Pts',(0.110233508147554,-1.12012616746575,
-0.770990446786831));
#25814=CARTESIAN_POINT('Ctrl Pts',(-0.202625788977264,-1.11169037854405,
-0.793308777819729));
#25815=CARTESIAN_POINT('Ctrl Pts',(-0.344594062564993,-1.06910154094398,
-0.803660097358051));
#25816=CARTESIAN_POINT('Ctrl Pts',(-0.586363065095523,-0.959974916638414,
-0.822550244130425));
#25817=CARTESIAN_POINT('Ctrl Pts',(-0.704733656287598,-0.877644037487908,
-0.832635757158428));
#25818=CARTESIAN_POINT('Ctrl Pts',(-0.924445762809,-0.651144082671884,-0.855147894869199));
#25819=CARTESIAN_POINT('Ctrl Pts',(-0.99587830302718,-0.517818669122217,
-0.865692152173815));
#25820=CARTESIAN_POINT('Ctrl Pts',(-1.08982166380632,-0.277939862987315,
-0.884035045773487));
#25821=CARTESIAN_POINT('Ctrl Pts',(-1.1169872981078,-0.139044412854726,
-0.89394629670385));
#25822=CARTESIAN_POINT('Ctrl Pts',(-1.1169872981078,0.139044412854725,-0.91378873021515));
#25823=CARTESIAN_POINT('Ctrl Pts',(-1.08982166380632,0.277939862987314,
-0.9236999811454));
#25824=CARTESIAN_POINT('Ctrl Pts',(-0.995878303027182,0.517818669122212,
-0.942042874744956));
#25825=CARTESIAN_POINT('Ctrl Pts',(-0.924445762809003,0.651144082671879,
-0.952587132049651));
#25826=CARTESIAN_POINT('Ctrl Pts',(-0.704733656287602,0.877644037487905,
-0.975099269760432));
#25827=CARTESIAN_POINT('Ctrl Pts',(-0.586363065095528,0.959974916638411,
-0.985184782788548));
#25828=CARTESIAN_POINT('Ctrl Pts',(-0.344594062565002,1.06910154094397,
-1.00407492956102));
#25829=CARTESIAN_POINT('Ctrl Pts',(-0.202625788977273,1.11169037854405,
-1.01442624909947));
#25830=CARTESIAN_POINT('Ctrl Pts',(0.110233508147546,1.12012616746575,-1.0367445801323));
#25831=CARTESIAN_POINT('Ctrl Pts',(0.254954649474654,1.09592824110065,-1.04699768638824));
#25832=CARTESIAN_POINT('Ctrl Pts',(0.499473987912827,1.00559671816686,-1.06556906177382));
#25833=CARTESIAN_POINT('Ctrl Pts',(0.63090821136934,0.938430669099267,-1.07587443060856));
#25834=CARTESIAN_POINT('Ctrl Pts',(0.865889506205115,0.719096632405891,
-1.0987834817475));
#25835=CARTESIAN_POINT('Ctrl Pts',(0.953355092950176,0.598483057720668,
-1.10918759237701));
#25836=CARTESIAN_POINT('Ctrl Pts',(1.09120934524512,0.300938815206533,-1.13256466454209));
#25837=CARTESIAN_POINT('Ctrl Pts',(1.11127472608703,0.15238299872601,-1.14301472769363));
#25838=CARTESIAN_POINT('Ctrl Pts',(1.12102369397598,-0.101931202388078,
-1.16114310364356));
#25839=CARTESIAN_POINT('Ctrl Pts',(1.09791444748827,-0.250846118613163,
-1.17166474109357));
#25840=CARTESIAN_POINT('Ctrl Pts',(0.98930402061091,-0.54516302107658,-1.19404248596663));
#25841=CARTESIAN_POINT('Ctrl Pts',(0.905273423514496,-0.663857977873313,
-1.20420257483709));
#25842=CARTESIAN_POINT('Ctrl Pts',(0.725113385898957,-0.861211673415817,
-1.2232305070904));
#25843=CARTESIAN_POINT('Ctrl Pts',(0.603413551668539,-0.951563052462835,
-1.23381686695743));
#25844=CARTESIAN_POINT('Ctrl Pts',(0.341786112597045,-1.07261170247852,
-1.25438591132205));
#25845=CARTESIAN_POINT('Ctrl Pts',(0.203851405860754,-1.10611718857029,
-1.26432633133823));
#25846=CARTESIAN_POINT('Ctrl Pts',(-0.0349012702549558,-1.12007370080308,
-1.28135486833774));
#25847=CARTESIAN_POINT('Ctrl Pts',(-0.191201997533714,-1.11682300306852,
-1.29221809027823));
#25848=CARTESIAN_POINT('Ctrl Pts',(-0.502214996937538,-1.0073238571117,
-1.31574203875159));
#25849=CARTESIAN_POINT('Ctrl Pts',(-0.626214316349852,-0.934430304671204,
-1.32580461866347));
#25850=CARTESIAN_POINT('Ctrl Pts',(-0.825915661788611,-0.761161572818582,
-1.34463244532763));
#25851=CARTESIAN_POINT('Ctrl Pts',(-0.924464855646192,-0.649976757040037,
-1.35500640985656));
#25852=CARTESIAN_POINT('Ctrl Pts',(-1.06324590215937,-0.369253565391388,
-1.3773391931262));
#25853=CARTESIAN_POINT('Ctrl Pts',(-1.10179845703877,-0.228016486144762,
-1.38757072082651));
#25854=CARTESIAN_POINT('Ctrl Pts',(-1.1216526627367,0.0230529286473262,
-1.40551263954272));
#25855=CARTESIAN_POINT('Ctrl Pts',(-1.11857306467122,0.173002860562925,
-1.41597065679271));
#25856=CARTESIAN_POINT('Ctrl Pts',(-1.01607631574407,0.484189787750164,
-1.43932287502835));
#25857=CARTESIAN_POINT('Ctrl Pts',(-0.943397907937868,0.61393454762198,
-1.4497083967475));
#25858=CARTESIAN_POINT('Ctrl Pts',(-0.731331226988447,0.86397400629996,
-1.47307863229063));
#25859=CARTESIAN_POINT('Ctrl Pts',(-0.604852724324511,0.944731736167629,
-1.48354062141298));
#25860=CARTESIAN_POINT('Ctrl Pts',(-0.377700605109023,1.06037143957915,
-1.50169805664461));
#25861=CARTESIAN_POINT('Ctrl Pts',(-0.232981315456773,1.10176800386664,
-1.51220746164666));
#25862=CARTESIAN_POINT('Ctrl Pts',(0.0794663775051852,1.12675755955542,
-1.53456428016245));
#25863=CARTESIAN_POINT('Ctrl Pts',(0.222597234321235,1.1004636264182,-1.54473227882704));
#25864=CARTESIAN_POINT('Ctrl Pts',(0.478234529751102,1.0191711099922,-1.56383422514426));
#25865=CARTESIAN_POINT('Ctrl Pts',(0.611182247799714,0.946513834085742,
-1.57441525733418));
#25866=CARTESIAN_POINT('Ctrl Pts',(0.840538191683133,0.751460714065254,
-1.59589801163903));
#25867=CARTESIAN_POINT('Ctrl Pts',(0.925588908242788,0.636392952388505,
-1.60591009521362));
#25868=CARTESIAN_POINT('Ctrl Pts',(1.02997735713438,0.440477084841939,-1.62171618375237));
#25869=CARTESIAN_POINT('Ctrl Pts',(1.09418460733438,0.296790717289617,-1.632638099872));
#25870=CARTESIAN_POINT('Ctrl Pts',(1.1250370353998,-0.0352369170928104,
-1.65642866117049));
#25871=CARTESIAN_POINT('Ctrl Pts',(1.1106661667445,-0.17804237558137,-1.66647070761317));
#25872=CARTESIAN_POINT('Ctrl Pts',(1.03703915589556,-0.431145768277768,
-1.68524121999164));
#25873=CARTESIAN_POINT('Ctrl Pts',(0.977352549963126,-0.567498199932388,
-1.69563223691796));
#25874=CARTESIAN_POINT('Ctrl Pts',(0.780383055419231,-0.811029500761411,
-1.71797004573513));
#25875=CARTESIAN_POINT('Ctrl Pts',(0.668471432388786,-0.904915646636013,
-1.72817926042076));
#25876=CARTESIAN_POINT('Ctrl Pts',(0.461203748610871,-1.02120417552908,
-1.74510952128988));
#25877=CARTESIAN_POINT('Ctrl Pts',(0.372801878430357,-1.05728988862616,
-1.75186529968031));
#25878=CARTESIAN_POINT('Ctrl Pts',(0.189124507262833,-1.1048491526056,-1.76540775381491));
#25879=CARTESIAN_POINT('Ctrl Pts',(0.094547706959705,-1.1164597472411,-1.77214984360044));
#25880=CARTESIAN_POINT('Ctrl Pts',(2.02707199885784E-6,-1.11628565404413,
-1.77888591117587));
#25881=CARTESIAN_POINT('Ctrl Pts',(-0.4696881186261,0.9981380597272,0.01413543027923));
#25882=CARTESIAN_POINT('Ctrl Pts',(-0.2318942596183,1.110035356068,-0.004822903054108));
#25883=CARTESIAN_POINT('Ctrl Pts',(0.3258579542137,1.155927922117,-0.04273956972077));
#25884=CARTESIAN_POINT('Ctrl Pts',(1.003936318643,0.6594544137959,-0.09961456972077));
#25885=CARTESIAN_POINT('Ctrl Pts',(1.190400720751,-0.1598981886148,-0.1564895697208));
#25886=CARTESIAN_POINT('Ctrl Pts',(0.7943069665412,-0.9009591520544,-0.2133645697208));
#25887=CARTESIAN_POINT('Ctrl Pts',(0.009432467987834,-1.201066414053,-0.2702395697208));
#25888=CARTESIAN_POINT('Ctrl Pts',(-0.7800537946193,-0.9133258114035,-0.3271145697208));
#25889=CARTESIAN_POINT('Ctrl Pts',(-1.187754649245,-0.1785709428966,-0.3839895697208));
#25890=CARTESIAN_POINT('Ctrl Pts',(-1.014124826746,0.6435832038027,-0.4408645697208));
#25891=CARTESIAN_POINT('Ctrl Pts',(-0.3441455177085,1.150744276231,-0.4977395697208));
#25892=CARTESIAN_POINT('Ctrl Pts',(0.4942711510281,1.094689252768,-0.5546145697208));
#25893=CARTESIAN_POINT('Ctrl Pts',(1.090773532456,0.5028534860695,-0.6114895697208));
#25894=CARTESIAN_POINT('Ctrl Pts',(1.153411671532,-0.3350970673819,-0.6683645697208));
#25895=CARTESIAN_POINT('Ctrl Pts',(0.6515281822355,-1.009038926982,-0.7252395697208));
#25896=CARTESIAN_POINT('Ctrl Pts',(-0.169236898936,-1.189120431432,-0.7821145697208));
#25897=CARTESIAN_POINT('Ctrl Pts',(-0.9071712857378,-0.7872031419892,-0.8389895697208));
#25898=CARTESIAN_POINT('Ctrl Pts',(-1.201103046544,0.,-0.8958645697208));
#25899=CARTESIAN_POINT('Ctrl Pts',(-0.9071712857378,0.7872031419892,-0.9527395697208));
#25900=CARTESIAN_POINT('Ctrl Pts',(-0.169236898936,1.189120431432,-1.009614569721));
#25901=CARTESIAN_POINT('Ctrl Pts',(0.6515281822355,1.009038926982,-1.066489569721));
#25902=CARTESIAN_POINT('Ctrl Pts',(1.153411671532,0.3350970673819,-1.123364569721));
#25903=CARTESIAN_POINT('Ctrl Pts',(1.090773532456,-0.5028534860695,-1.180239569721));
#25904=CARTESIAN_POINT('Ctrl Pts',(0.4942711510281,-1.094689252768,-1.237114569721));
#25905=CARTESIAN_POINT('Ctrl Pts',(-0.3441455177085,-1.150744276231,-1.293989569721));
#25906=CARTESIAN_POINT('Ctrl Pts',(-1.014124826746,-0.6435832038027,-1.350864569721));
#25907=CARTESIAN_POINT('Ctrl Pts',(-1.187754649245,0.1785709428966,-1.407739569721));
#25908=CARTESIAN_POINT('Ctrl Pts',(-0.7800537946193,0.9133258114035,-1.464614569721));
#25909=CARTESIAN_POINT('Ctrl Pts',(0.009432467987832,1.201066414053,-1.521489569721));
#25910=CARTESIAN_POINT('Ctrl Pts',(0.7943069665412,0.9009591520544,-1.578364569721));
#25911=CARTESIAN_POINT('Ctrl Pts',(1.190400720751,0.1598981886148,-1.635239569721));
#25912=CARTESIAN_POINT('Ctrl Pts',(1.003936318643,-0.6594544137959,-1.692114569721));
#25913=CARTESIAN_POINT('Ctrl Pts',(0.3258579542138,-1.155927922117,-1.748989569721));
#25914=CARTESIAN_POINT('Ctrl Pts',(-0.2318942596183,-1.110035356068,-1.786906236387));
#25915=CARTESIAN_POINT('Ctrl Pts',(-0.4696881186261,-0.9981380597272,-1.805864569721));
#25916=CARTESIAN_POINT('Ctrl Pts',(-0.5279823721497,1.122019654338,-0.06491069439342));
#25917=CARTESIAN_POINT('Ctrl Pts',(-0.2606752788197,1.247804824574,-0.08386902772675));
#25918=CARTESIAN_POINT('Ctrl Pts',(0.3663010598456,1.299393240218,-0.1217856943934));
#25919=CARTESIAN_POINT('Ctrl Pts',(1.128537550737,0.7413010717389,-0.1786606943934));
#25920=CARTESIAN_POINT('Ctrl Pts',(1.33814455045,-0.1797435821333,-0.2355356943934));
#25921=CARTESIAN_POINT('Ctrl Pts',(0.892890536887,-1.012779611507,-0.2924106943934));
#25922=CARTESIAN_POINT('Ctrl Pts',(0.01060315691615,-1.350133991585,-0.3492856943934));
#25923=CARTESIAN_POINT('Ctrl Pts',(-0.8768683655278,-1.026681130153,-0.4061606943934));
#25924=CARTESIAN_POINT('Ctrl Pts',(-1.335170067905,-0.2007338620856,-0.4630356943934));
#25925=CARTESIAN_POINT('Ctrl Pts',(-1.139990581936,0.723460043259,-0.5199106943934));
#25926=CARTESIAN_POINT('Ctrl Pts',(-0.3868583419482,1.293566238123,-0.5767856943934));
#25927=CARTESIAN_POINT('Ctrl Pts',(0.555616470709,1.230554075189,-0.6336606943934));
#25928=CARTESIAN_POINT('Ctrl Pts',(1.226152364316,0.5652639823961,-0.6905356943934));
#25929=CARTESIAN_POINT('Ctrl Pts',(1.296564691016,-0.3766868641562,-0.7474106943934));
#25930=CARTESIAN_POINT('Ctrl Pts',(0.7323910942975,-1.134273457497,-0.8042856943934));
#25931=CARTESIAN_POINT('Ctrl Pts',(-0.190241344867,-1.336705360987,-0.8611606943934));
#25932=CARTESIAN_POINT('Ctrl Pts',(-1.019762749782,-0.8849050375959,-0.9180356943934));
#25933=CARTESIAN_POINT('Ctrl Pts',(-1.350175170634,0.,-0.9749106943934));
#25934=CARTESIAN_POINT('Ctrl Pts',(-1.019762749782,0.8849050375959,-1.031785694393));
#25935=CARTESIAN_POINT('Ctrl Pts',(-0.190241344867,1.336705360987,-1.088660694393));
#25936=CARTESIAN_POINT('Ctrl Pts',(0.7323910942975,1.134273457497,-1.145535694393));
#25937=CARTESIAN_POINT('Ctrl Pts',(1.296564691016,0.3766868641562,-1.202410694393));
#25938=CARTESIAN_POINT('Ctrl Pts',(1.226152364316,-0.5652639823961,-1.259285694393));
#25939=CARTESIAN_POINT('Ctrl Pts',(0.555616470709,-1.230554075189,-1.316160694393));
#25940=CARTESIAN_POINT('Ctrl Pts',(-0.3868583419482,-1.293566238123,-1.373035694393));
#25941=CARTESIAN_POINT('Ctrl Pts',(-1.139990581936,-0.723460043259,-1.429910694393));
#25942=CARTESIAN_POINT('Ctrl Pts',(-1.335170067905,0.2007338620856,-1.486785694393));
#25943=CARTESIAN_POINT('Ctrl Pts',(-0.8768683655278,1.026681130153,-1.543660694393));
#25944=CARTESIAN_POINT('Ctrl Pts',(0.01060315691615,1.350133991585,-1.600535694393));
#25945=CARTESIAN_POINT('Ctrl Pts',(0.892890536887,1.012779611507,-1.657410694393));
#25946=CARTESIAN_POINT('Ctrl Pts',(1.33814455045,0.1797435821333,-1.714285694393));
#25947=CARTESIAN_POINT('Ctrl Pts',(1.128537550737,-0.7413010717389,-1.771160694393));
#25948=CARTESIAN_POINT('Ctrl Pts',(0.3663010598456,-1.299393240218,-1.828035694393));
#25949=CARTESIAN_POINT('Ctrl Pts',(-0.2606752788197,-1.247804824574,-1.86595236106));
#25950=CARTESIAN_POINT('Ctrl Pts',(-0.5279823721497,-1.122019654338,-1.884910694393));
#25951=CARTESIAN_POINT('Ctrl Pts',(-0.5862766256734,1.24590124895,-0.1439568190661));
#25952=CARTESIAN_POINT('Ctrl Pts',(-0.2894562980212,1.38557429308,-0.1629151523994));
#25953=CARTESIAN_POINT('Ctrl Pts',(0.4067441654775,1.442858558319,-0.2008318190661));
#25954=CARTESIAN_POINT('Ctrl Pts',(1.253138782831,0.823147729682,-0.2577068190661));
#25955=CARTESIAN_POINT('Ctrl Pts',(1.48588838015,-0.1995889756518,-0.3145818190661));
#25956=CARTESIAN_POINT('Ctrl Pts',(0.9914741072328,-1.12460007096,-0.3714568190661));
#25957=CARTESIAN_POINT('Ctrl Pts',(0.01177384584446,-1.499201569118,-0.4283318190661));
#25958=CARTESIAN_POINT('Ctrl Pts',(-0.9736829364363,-1.140036448902,-0.4852068190661));
#25959=CARTESIAN_POINT('Ctrl Pts',(-1.482585486565,-0.2228967812747,-0.5420818190661));
#25960=CARTESIAN_POINT('Ctrl Pts',(-1.265856337127,0.8033368827153,-0.5989568190661));
#25961=CARTESIAN_POINT('Ctrl Pts',(-0.4295711661878,1.436388200015,-0.6558318190661));
#25962=CARTESIAN_POINT('Ctrl Pts',(0.61696179039,1.36641889761,-0.7127068190661));
#25963=CARTESIAN_POINT('Ctrl Pts',(1.361531196175,0.6276744787227,-0.7695818190661));
#25964=CARTESIAN_POINT('Ctrl Pts',(1.439717710501,-0.4182766609306,-0.8264568190661));
#25965=CARTESIAN_POINT('Ctrl Pts',(0.8132540063595,-1.259507988013,-0.8833318190661));
#25966=CARTESIAN_POINT('Ctrl Pts',(-0.211245790798,-1.484290290542,-0.9402068190661));
#25967=CARTESIAN_POINT('Ctrl Pts',(-1.132354213826,-0.9826069332027,-0.9970818190661));
#25968=CARTESIAN_POINT('Ctrl Pts',(-1.499247294724,0.,-1.053956819066));
#25969=CARTESIAN_POINT('Ctrl Pts',(-1.132354213826,0.9826069332027,-1.110831819066));
#25970=CARTESIAN_POINT('Ctrl Pts',(-0.211245790798,1.484290290542,-1.167706819066));
#25971=CARTESIAN_POINT('Ctrl Pts',(0.8132540063595,1.259507988012,-1.224581819066));
#25972=CARTESIAN_POINT('Ctrl Pts',(1.439717710501,0.4182766609306,-1.281456819066));
#25973=CARTESIAN_POINT('Ctrl Pts',(1.361531196175,-0.6276744787227,-1.338331819066));
#25974=CARTESIAN_POINT('Ctrl Pts',(0.61696179039,-1.36641889761,-1.395206819066));
#25975=CARTESIAN_POINT('Ctrl Pts',(-0.4295711661878,-1.436388200015,-1.452081819066));
#25976=CARTESIAN_POINT('Ctrl Pts',(-1.265856337127,-0.8033368827153,-1.508956819066));
#25977=CARTESIAN_POINT('Ctrl Pts',(-1.482585486565,0.2228967812747,-1.565831819066));
#25978=CARTESIAN_POINT('Ctrl Pts',(-0.9736829364363,1.140036448902,-1.622706819066));
#25979=CARTESIAN_POINT('Ctrl Pts',(0.01177384584446,1.499201569118,-1.679581819066));
#25980=CARTESIAN_POINT('Ctrl Pts',(0.9914741072328,1.12460007096,-1.736456819066));
#25981=CARTESIAN_POINT('Ctrl Pts',(1.48588838015,0.1995889756517,-1.793331819066));
#25982=CARTESIAN_POINT('Ctrl Pts',(1.253138782831,-0.823147729682,-1.850206819066));
#25983=CARTESIAN_POINT('Ctrl Pts',(0.4067441654775,-1.442858558319,-1.907081819066));
#25984=CARTESIAN_POINT('Ctrl Pts',(-0.2894562980212,-1.38557429308,-1.944998485733));
#25985=CARTESIAN_POINT('Ctrl Pts',(-0.5862766256734,-1.24590124895,-1.963956819066));
#25986=CARTESIAN_POINT('Ctrl Pts',(-0.644570879197,1.369782843561,-0.2230029437387));
#25987=CARTESIAN_POINT('Ctrl Pts',(-0.3182373172226,1.523343761587,-0.241961277072));
#25988=CARTESIAN_POINT('Ctrl Pts',(0.4471872711094,1.586323876419,-0.2798779437387));
#25989=CARTESIAN_POINT('Ctrl Pts',(1.377740014924,0.904994387625,-0.3367529437387));
#25990=CARTESIAN_POINT('Ctrl Pts',(1.633632209849,-0.2194343691702,-0.3936279437387));
#25991=CARTESIAN_POINT('Ctrl Pts',(1.090057677579,-1.236420530413,-0.4505029437387));
#25992=CARTESIAN_POINT('Ctrl Pts',(0.01294453477278,-1.648269146651,-0.5073779437387));
#25993=CARTESIAN_POINT('Ctrl Pts',(-1.070497507345,-1.253391767652,-0.5642529437387));
#25994=CARTESIAN_POINT('Ctrl Pts',(-1.630000905225,-0.2450597004638,-0.6211279437387));
#25995=CARTESIAN_POINT('Ctrl Pts',(-1.391722092318,0.8832137221716,-0.6780029437387));
#25996=CARTESIAN_POINT('Ctrl Pts',(-0.4722839904274,1.579210161907,-0.7348779437387));
#25997=CARTESIAN_POINT('Ctrl Pts',(0.6783071100709,1.502283720031,-0.7917529437387));
#25998=CARTESIAN_POINT('Ctrl Pts',(1.496910028035,0.6900849750494,-0.8486279437387));
#25999=CARTESIAN_POINT('Ctrl Pts',(1.582870729986,-0.4598664577049,-0.9055029437387));
#26000=CARTESIAN_POINT('Ctrl Pts',(0.8941169184215,-1.384742518528,-0.9623779437387));
#26001=CARTESIAN_POINT('Ctrl Pts',(-0.232250236729,-1.631875220096,-1.019252943739));
#26002=CARTESIAN_POINT('Ctrl Pts',(-1.24494567787,-1.080308828809,-1.076127943739));
#26003=CARTESIAN_POINT('Ctrl Pts',(-1.648319418813,0.,-1.133002943739));
#26004=CARTESIAN_POINT('Ctrl Pts',(-1.24494567787,1.080308828809,-1.189877943739));
#26005=CARTESIAN_POINT('Ctrl Pts',(-0.232250236729,1.631875220096,-1.246752943739));
#26006=CARTESIAN_POINT('Ctrl Pts',(0.8941169184216,1.384742518528,-1.303627943739));
#26007=CARTESIAN_POINT('Ctrl Pts',(1.582870729986,0.4598664577049,-1.360502943739));
#26008=CARTESIAN_POINT('Ctrl Pts',(1.496910028035,-0.6900849750494,-1.417377943739));
#26009=CARTESIAN_POINT('Ctrl Pts',(0.6783071100709,-1.502283720031,-1.474252943739));
#26010=CARTESIAN_POINT('Ctrl Pts',(-0.4722839904274,-1.579210161907,-1.531127943739));
#26011=CARTESIAN_POINT('Ctrl Pts',(-1.391722092318,-0.8832137221716,-1.588002943739));
#26012=CARTESIAN_POINT('Ctrl Pts',(-1.630000905225,0.2450597004637,-1.644877943739));
#26013=CARTESIAN_POINT('Ctrl Pts',(-1.070497507345,1.253391767652,-1.701752943739));
#26014=CARTESIAN_POINT('Ctrl Pts',(0.01294453477277,1.648269146651,-1.758627943739));
#26015=CARTESIAN_POINT('Ctrl Pts',(1.090057677579,1.236420530413,-1.815502943739));
#26016=CARTESIAN_POINT('Ctrl Pts',(1.633632209849,0.2194343691702,-1.872377943739));
#26017=CARTESIAN_POINT('Ctrl Pts',(1.377740014924,-0.904994387625,-1.929252943739));
#26018=CARTESIAN_POINT('Ctrl Pts',(0.4471872711094,-1.586323876419,-1.986127943739));
#26019=CARTESIAN_POINT('Ctrl Pts',(-0.3182373172226,-1.523343761587,-2.024044610405));
#26020=CARTESIAN_POINT('Ctrl Pts',(-0.644570879197,-1.369782843561,-2.043002943739));
#26021=CARTESIAN_POINT('',(2.6147125314471E-5,1.4994193789824,-0.249671053225285));
#26022=CARTESIAN_POINT('',(0.,1.5,-0.25));
#26023=CARTESIAN_POINT('',(1.98293436217802E-9,-1.49923261688451,-1.99955700104142));
#26024=CARTESIAN_POINT('',(0.,-1.116987298108,-1.778867513459));
#26025=CARTESIAN_POINT('',(-1.55320824700497E-8,-1.49924686572649,-1.50043442831647));
#26026=CARTESIAN_POINT('Ctrl Pts',(2.23097736337663E-5,-1.49898153286063,
-1.99997329818231));
#26027=CARTESIAN_POINT('Ctrl Pts',(0.134297962277318,-1.49921292007654,
-1.99284084598502));
#26028=CARTESIAN_POINT('Ctrl Pts',(0.268638523155257,-1.48177177551889,
-1.98571955970265));
#26029=CARTESIAN_POINT('Ctrl Pts',(0.528263194565878,-1.41043852051632,
-1.97148351049348));
#26030=CARTESIAN_POINT('Ctrl Pts',(0.652764590084534,-1.35640660493856,
-1.96435339623912));
#26031=CARTESIAN_POINT('Ctrl Pts',(0.931735103478781,-1.18914032301524,
-1.94707782151409));
#26032=CARTESIAN_POINT('Ctrl Pts',(1.07750845761536,-1.05993255468443,-1.93689193230597));
#26033=CARTESIAN_POINT('Ctrl Pts',(1.25254449437154,-0.831135567222865,
-1.92160665898308));
#26034=CARTESIAN_POINT('Ctrl Pts',(1.30304053657959,-0.749217456505738,
-1.91653952634601));
#26035=CARTESIAN_POINT('Ctrl Pts',(1.43181227758846,-0.485623244975981,
-1.90097008905635));
#26036=CARTESIAN_POINT('Ctrl Pts',(1.48316629283892,-0.291367104629342,
-1.89048350490497));
#26037=CARTESIAN_POINT('Ctrl Pts',(1.50934594974658,0.102298044287199,-1.8695359424923));
#26038=CARTESIAN_POINT('Ctrl Pts',(1.48352325672049,0.297075466163154,-1.85935213742399));
#26039=CARTESIAN_POINT('Ctrl Pts',(1.35557807886251,0.667978310212381,-1.83851893537112));
#26040=CARTESIAN_POINT('Ctrl Pts',(1.25672313739978,0.83970672062861,-1.82816969083531));
#26041=CARTESIAN_POINT('Ctrl Pts',(1.06762979706196,1.05767316039942,-1.81285467637234));
#26042=CARTESIAN_POINT('Ctrl Pts',(0.999123065546441,1.12299746696215,-1.80786874916872));
#26043=CARTESIAN_POINT('Ctrl Pts',(0.767476069975274,1.30345302823293,-1.79230752936234));
#26044=CARTESIAN_POINT('Ctrl Pts',(0.585984240279098,1.39346679007975,-1.78173766448593));
#26045=CARTESIAN_POINT('Ctrl Pts',(0.300277913889601,1.47207216422033,-1.7659960136364));
#26046=CARTESIAN_POINT('Ctrl Pts',(0.203413602327542,1.48897911420525,-1.76079851833577));
#26047=CARTESIAN_POINT('Ctrl Pts',(0.0102967612380773,1.50310836043465,
-1.75053281932962));
#26048=CARTESIAN_POINT('Ctrl Pts',(-0.0847305214639188,1.50057827069591,
-1.7455288363176));
#26049=CARTESIAN_POINT('Ctrl Pts',(-0.371065612297978,1.46518487578872,
-1.7302202765876));
#26050=CARTESIAN_POINT('Ctrl Pts',(-0.55852855100465,1.40403962788438,-1.71992087466587));
#26051=CARTESIAN_POINT('Ctrl Pts',(-0.901532722071179,1.21492385002722,
-1.69911972638573));
#26052=CARTESIAN_POINT('Ctrl Pts',(-1.05210324466703,1.08744435980206,-1.68889367702815));
#26053=CARTESIAN_POINT('Ctrl Pts',(-1.29645230872772,0.777009626499769,
-1.66791552392223));
#26054=CARTESIAN_POINT('Ctrl Pts',(-1.38796566499361,0.59897654274782,-1.65746396444275));
#26055=CARTESIAN_POINT('Ctrl Pts',(-1.49653067286123,0.222284704147848,
-1.63665964848054));
#26056=CARTESIAN_POINT('Ctrl Pts',(-1.51209522503029,0.030383734062011,
-1.62667625208365));
#26057=CARTESIAN_POINT('Ctrl Pts',(-1.46756788059896,-0.362285500545997,
-1.60568821925797));
#26058=CARTESIAN_POINT('Ctrl Pts',(-1.40686745038182,-0.555204034967444,
-1.59513614417251));
#26059=CARTESIAN_POINT('Ctrl Pts',(-1.26475548289951,-0.812299601436654,
-1.57955746641289));
#26060=CARTESIAN_POINT('Ctrl Pts',(-1.21076632254199,-0.890422548519847,
-1.57455459690986));
#26061=CARTESIAN_POINT('Ctrl Pts',(-1.0247982663024,-1.11092223632562,-1.5592371921963));
#26062=CARTESIAN_POINT('Ctrl Pts',(-0.871086221419003,-1.23469578181935,
-1.54892247495095));
#26063=CARTESIAN_POINT('Ctrl Pts',(-0.593557655491734,-1.38241748281778,
-1.53223369317102));
#26064=CARTESIAN_POINT('Ctrl Pts',(-0.479696532132474,-1.4266223627924,
-1.52581914810394));
#26065=CARTESIAN_POINT('Ctrl Pts',(-0.242997175564243,-1.48494069752041,
-1.51292148769707));
#26066=CARTESIAN_POINT('Ctrl Pts',(-0.12147955209144,-1.49919084530293,
-1.50647826589496));
#26067=CARTESIAN_POINT('Ctrl Pts',(-2.21303979701729E-5,-1.49898153255151,
-1.50002669228961));
#26068=CARTESIAN_POINT('',(-5.94856812453578E-6,-1.49980089084043,-0.499887533576674));
#26069=CARTESIAN_POINT('Ctrl Pts',(-1.99648916368068E-5,-1.49907115383004,
-1.50007835931766));
#26070=CARTESIAN_POINT('Ctrl Pts',(0.100010792179548,-1.49907329786687,
-1.49486616364447));
#26071=CARTESIAN_POINT('Ctrl Pts',(0.200069985078629,-1.48925441345302,
-1.48963801729206));
#26072=CARTESIAN_POINT('Ctrl Pts',(0.390249520322464,-1.45111632655054,
-1.47928869001663));
#26073=CARTESIAN_POINT('Ctrl Pts',(0.479780074262229,-1.42412384089412,
-1.47417772966106));
#26074=CARTESIAN_POINT('Ctrl Pts',(0.743202348689664,-1.31644836894232,
-1.45869240472173));
#26075=CARTESIAN_POINT('Ctrl Pts',(0.890131060916161,-1.21634961998574,
-1.44967981979634));
#26076=CARTESIAN_POINT('Ctrl Pts',(1.09461260844504,-1.03108060982117,-1.43533626589644));
#26077=CARTESIAN_POINT('Ctrl Pts',(1.1729008973174,-0.941745915552239,-1.42915580900288));
#26078=CARTESIAN_POINT('Ctrl Pts',(1.30586262347788,-0.74705652125546,-1.41637434299397));
#26079=CARTESIAN_POINT('Ctrl Pts',(1.36019807409692,-0.642744360951115,
-1.40991938178315));
#26080=CARTESIAN_POINT('Ctrl Pts',(1.43684888869537,-0.439512380455255,
-1.39841603094486));
#26081=CARTESIAN_POINT('Ctrl Pts',(1.46258240871579,-0.343438435407343,
-1.39329338565573));
#26082=CARTESIAN_POINT('Ctrl Pts',(1.4955073700359,-0.145370938819839,-1.38288605729537));
#26083=CARTESIAN_POINT('Ctrl Pts',(1.50215165440464,-0.0432317669545728,
-1.37759510159625));
#26084=CARTESIAN_POINT('Ctrl Pts',(1.49493265746611,0.150815175439314,-1.36722522754921));
#26085=CARTESIAN_POINT('Ctrl Pts',(1.48294425990366,0.241996318482833,-1.36217498793555));
#26086=CARTESIAN_POINT('Ctrl Pts',(1.4171223673639,0.531784006300281,-1.34595372867182));
#26087=CARTESIAN_POINT('Ctrl Pts',(1.33544689557698,0.699314133729542,-1.33659896396809));
#26088=CARTESIAN_POINT('Ctrl Pts',(1.19973229083852,0.903152679566719,-1.32390070890711));
#26089=CARTESIAN_POINT('Ctrl Pts',(1.14617866632872,0.970503721518277,-1.31941772892764));
#26090=CARTESIAN_POINT('Ctrl Pts',(1.02308385799108,1.10045192315476,-1.309800909446));
#26091=CARTESIAN_POINT('Ctrl Pts',(0.952612668514966,1.16201288551934,-1.30463751792554));
#26092=CARTESIAN_POINT('Ctrl Pts',(0.749672622361954,1.30821426838173,-1.2910095866553));
#26093=CARTESIAN_POINT('Ctrl Pts',(0.608352109295587,1.37900069556785,-1.28295864515549));
#26094=CARTESIAN_POINT('Ctrl Pts',(0.377206086272509,1.45358015351625,-1.27041671486279));
#26095=CARTESIAN_POINT('Ctrl Pts',(0.292097969799569,1.47319097101559,-1.26590263694807));
#26096=CARTESIAN_POINT('Ctrl Pts',(0.0898567471207522,1.50150376362953,
-1.25501677461679));
#26097=CARTESIAN_POINT('Ctrl Pts',(-0.0272253993977831,1.5039278197908,
-1.24853630947231));
#26098=CARTESIAN_POINT('Ctrl Pts',(-0.298527879387531,1.4777809042739,-1.23372098560702));
#26099=CARTESIAN_POINT('Ctrl Pts',(-0.45044657350189,1.4382619968281,-1.2257758523679));
#26100=CARTESIAN_POINT('Ctrl Pts',(-0.691046340416202,1.33481966129264,
-1.21226172515724));
#26101=CARTESIAN_POINT('Ctrl Pts',(-0.78505272569885,1.28205564623737,-1.20666418776859));
#26102=CARTESIAN_POINT('Ctrl Pts',(-0.953191872890371,1.16185980252796,
-1.1954464713411));
#26103=CARTESIAN_POINT('Ctrl Pts',(-1.02802544796662,1.09622974031063,-1.18994188269062));
#26104=CARTESIAN_POINT('Ctrl Pts',(-1.19354290531248,0.919019881447236,
-1.17681353188812));
#26105=CARTESIAN_POINT('Ctrl Pts',(-1.27570185142782,0.800404022341491,
-1.16951178509106));
#26106=CARTESIAN_POINT('Ctrl Pts',(-1.38768122665806,0.577628143130332,
-1.15666830613508));
#26107=CARTESIAN_POINT('Ctrl Pts',(-1.42556288709254,0.477113380022469,
-1.15109714816553));
#26108=CARTESIAN_POINT('Ctrl Pts',(-1.47781991767828,0.273941629700634,
-1.1397165799079));
#26109=CARTESIAN_POINT('Ctrl Pts',(-1.49313607998845,0.172070011743343,
-1.13401960730222));
#26110=CARTESIAN_POINT('Ctrl Pts',(-1.50371664120506,-0.0551323601073528,
-1.12170116965879));
#26111=CARTESIAN_POINT('Ctrl Pts',(-1.49366873901588,-0.180040504057676,
-1.11529369189568));
#26112=CARTESIAN_POINT('Ctrl Pts',(-1.44320719446622,-0.425509966378713,
-1.10242124470283));
#26113=CARTESIAN_POINT('Ctrl Pts',(-1.40223811657279,-0.546093269237912,
-1.09587535154167));
#26114=CARTESIAN_POINT('Ctrl Pts',(-1.26881799908278,-0.818122243168699,
-1.07941603801019));
#26115=CARTESIAN_POINT('Ctrl Pts',(-1.15460642284242,-0.981022106197246,
-1.06857417798349));
#26116=CARTESIAN_POINT('Ctrl Pts',(-0.897625310307818,-1.20753212352388,
-1.05094200853052));
#26117=CARTESIAN_POINT('Ctrl Pts',(-0.763406902307776,-1.30530337522424,
-1.04266849888574));
#26118=CARTESIAN_POINT('Ctrl Pts',(-0.432379286030744,-1.44495334384168,
-1.02310454786419));
#26119=CARTESIAN_POINT('Ctrl Pts',(-0.24768634626944,-1.494071802094,-1.0126836955935));
#26120=CARTESIAN_POINT('Ctrl Pts',(0.123993311035133,-1.50277099843374,
-0.99354665852439));
#26121=CARTESIAN_POINT('Ctrl Pts',(0.282789316550348,-1.48127209667292,
-0.985466284213652));
#26122=CARTESIAN_POINT('Ctrl Pts',(0.592840947756912,-1.38675471981538,
-0.967848554952269));
#26123=CARTESIAN_POINT('Ctrl Pts',(0.770188299195702,-1.30499820912315,
-0.957173992091056));
#26124=CARTESIAN_POINT('Ctrl Pts',(1.0091683764049,-1.11261880737999,-0.941380104211402));
#26125=CARTESIAN_POINT('Ctrl Pts',(1.073317430635,-1.05086531321477,-0.936872292770045));
#26126=CARTESIAN_POINT('Ctrl Pts',(1.20700755932124,-0.897034516416044,
-0.926243466813761));
#26127=CARTESIAN_POINT('Ctrl Pts',(1.2720596868803,-0.801725608748136,-0.919992081713298));
#26128=CARTESIAN_POINT('Ctrl Pts',(1.38574003033754,-0.586690589800353,
-0.906675857250465));
#26129=CARTESIAN_POINT('Ctrl Pts',(1.43150828147209,-0.464980700073504,
-0.899643953226378));
#26130=CARTESIAN_POINT('Ctrl Pts',(1.49753073591719,-0.180369835395416,
-0.88448612623695));
#26131=CARTESIAN_POINT('Ctrl Pts',(1.51285058584363,0.00247071549351316,
-0.875399835205175));
#26132=CARTESIAN_POINT('Ctrl Pts',(1.46230301349907,0.37267475367652,-0.855108229566284));
#26133=CARTESIAN_POINT('Ctrl Pts',(1.40593455773014,0.56796265523729,-0.844074579384696));
#26134=CARTESIAN_POINT('Ctrl Pts',(1.25251289572464,0.828285671734061,-0.828546501939329));
#26135=CARTESIAN_POINT('Ctrl Pts',(1.2078958083307,0.892061281596229,-0.824591589989435));
#26136=CARTESIAN_POINT('Ctrl Pts',(1.100827212269,1.02212890624593,-0.815794818911729));
#26137=CARTESIAN_POINT('Ctrl Pts',(1.03673876444052,1.08680447019536,-0.810902511090885));
#26138=CARTESIAN_POINT('Ctrl Pts',(0.860982719771297,1.23511568589174,-0.798382479495188));
#26139=CARTESIAN_POINT('Ctrl Pts',(0.718891117909026,1.3301263352465,-0.7890640585549));
#26140=CARTESIAN_POINT('Ctrl Pts',(0.422477786378846,1.44432400663123,-0.772644215476221));
#26141=CARTESIAN_POINT('Ctrl Pts',(0.301546629055091,1.47430348317788,-0.766383304558125));
#26142=CARTESIAN_POINT('Ctrl Pts',(0.0782712966722918,1.50050526795073,
-0.754410942138888));
#26143=CARTESIAN_POINT('Ctrl Pts',(-0.0218966802260001,1.50224799260922,
-0.748964773344174));
#26144=CARTESIAN_POINT('Ctrl Pts',(-0.248676328306329,1.48397607588603,
-0.736574336211773));
#26145=CARTESIAN_POINT('Ctrl Pts',(-0.375095119546514,1.45763411426832,
-0.729656514606377));
#26146=CARTESIAN_POINT('Ctrl Pts',(-0.612077379531005,1.37463449545206,
-0.716662996105306));
#26147=CARTESIAN_POINT('Ctrl Pts',(-0.721807835821291,1.32025327114755,
-0.710491973297748));
#26148=CARTESIAN_POINT('Ctrl Pts',(-0.915055210225513,1.19249631921147,
-0.698160760775035));
#26149=CARTESIAN_POINT('Ctrl Pts',(-0.999168138085294,1.12275051159727,
-0.692229347781927));
#26150=CARTESIAN_POINT('Ctrl Pts',(-1.1444484769929,0.973558823158012,-0.680918157030638));
#26151=CARTESIAN_POINT('Ctrl Pts',(-1.20700328585692,0.895307349521417,
-0.67553121744527));
#26152=CARTESIAN_POINT('Ctrl Pts',(-1.30668967310925,0.740930549865537,
-0.665897403655337));
#26153=CARTESIAN_POINT('Ctrl Pts',(-1.3461972124217,0.666466136868907,-0.661616642075847));
#26154=CARTESIAN_POINT('Ctrl Pts',(-1.45276490927942,0.416369341677812,
-0.647558516382313));
#26155=CARTESIAN_POINT('Ctrl Pts',(-1.4864222724122,0.246339841458581,-0.638220784166622));
#26156=CARTESIAN_POINT('Ctrl Pts',(-1.50250622978574,-0.00547396038538936,
-0.624547403106134));
#26157=CARTESIAN_POINT('Ctrl Pts',(-1.49910504162675,-0.105679094128752,
-0.619168655697039));
#26158=CARTESIAN_POINT('Ctrl Pts',(-1.47323337206388,-0.296077263212728,
-0.609090188545362));
#26159=CARTESIAN_POINT('Ctrl Pts',(-1.45224759160403,-0.386023362816676,
-0.604409926631516));
#26160=CARTESIAN_POINT('Ctrl Pts',(-1.38664469068925,-0.582199052059527,
-0.593640518279727));
#26161=CARTESIAN_POINT('Ctrl Pts',(-1.33755993494745,-0.686611593605869,
-0.587483783524372));
#26162=CARTESIAN_POINT('Ctrl Pts',(-1.19157954730198,-0.924069523552559,
-0.572418827905029));
#26163=CARTESIAN_POINT('Ctrl Pts',(-1.06921617363583,-1.07274929497444,
-0.562131028343388));
#26164=CARTESIAN_POINT('Ctrl Pts',(-0.838007112048112,-1.24636184039802,
-0.547178757121285));
#26165=CARTESIAN_POINT('Ctrl Pts',(-0.772275043899146,-1.2879809690239,
-0.543168246187858));
#26166=CARTESIAN_POINT('Ctrl Pts',(-0.595357994137584,-1.38133873895422,
-0.532596315569934));
#26167=CARTESIAN_POINT('Ctrl Pts',(-0.48049307141643,-1.42505352361137,
-0.52599765545279));
#26168=CARTESIAN_POINT('Ctrl Pts',(-0.243880376027954,-1.48416071365803,
-0.512837224887416));
#26169=CARTESIAN_POINT('Ctrl Pts',(-0.121966173250744,-1.49959078914017,
-0.506272370752933));
#26170=CARTESIAN_POINT('Ctrl Pts',(-5.94856812308198E-6,-1.49980089084043,
-0.499887533576674));
#26171=CARTESIAN_POINT('Ctrl Pts',(-5.45381040766187E-5,1.49913119745383,
-0.2500210497538));
#26172=CARTESIAN_POINT('Ctrl Pts',(0.0780741250135448,1.49929196137212,
-0.25417399022211));
#26173=CARTESIAN_POINT('Ctrl Pts',(0.156227279223828,1.49345098065259,-0.258324060294719));
#26174=CARTESIAN_POINT('Ctrl Pts',(0.310596746515901,1.46954678065932,-0.266598905901088));
#26175=CARTESIAN_POINT('Ctrl Pts',(0.386430580339945,1.45155040788365,-0.270688784714035));
#26176=CARTESIAN_POINT('Ctrl Pts',(0.510597996972894,1.41116401327425,-0.277603709312788));
#26177=CARTESIAN_POINT('Ctrl Pts',(0.559335006167078,1.39237630444979,-0.280375865718772));
#26178=CARTESIAN_POINT('Ctrl Pts',(0.784703042495158,1.29174833012765,-0.293517915139593));
#26179=CARTESIAN_POINT('Ctrl Pts',(0.947356094247462,1.17771675062754,-0.303973591508499));
#26180=CARTESIAN_POINT('Ctrl Pts',(1.14601025373637,0.97177688005302,-0.319123070038468));
#26181=CARTESIAN_POINT('Ctrl Pts',(1.20336533402626,0.900260866186981,-0.323904926989636));
#26182=CARTESIAN_POINT('Ctrl Pts',(1.3074220891629,0.74150612948606,-0.333871860552341));
#26183=CARTESIAN_POINT('Ctrl Pts',(1.35281468784255,0.654104018334678,-0.339082925501949));
#26184=CARTESIAN_POINT('Ctrl Pts',(1.46110290740528,0.385005677589548,-0.354573723739613));
#26185=CARTESIAN_POINT('Ctrl Pts',(1.49917179657801,0.192899123978207,-0.364932563984502));
#26186=CARTESIAN_POINT('Ctrl Pts',(1.50005395314928,-0.0935609344680583,
-0.380019105219707));
#26187=CARTESIAN_POINT('Ctrl Pts',(1.49128205669311,-0.187011148649471,
-0.384858146033504));
#26188=CARTESIAN_POINT('Ctrl Pts',(1.43858978421221,-0.46077828414352,-0.399586610860885));
#26189=CARTESIAN_POINT('Ctrl Pts',(1.36981503131428,-0.6354752183641,-0.409586106317029));
#26190=CARTESIAN_POINT('Ctrl Pts',(1.19399261033596,-0.919357485746789,
-0.427422853750231));
#26191=CARTESIAN_POINT('Ctrl Pts',(1.07023831968133,-1.07945897176414,-0.437570713370438));
#26192=CARTESIAN_POINT('Ctrl Pts',(0.745231599973944,-1.30969751346691,
-0.458761834351435));
#26193=CARTESIAN_POINT('Ctrl Pts',(0.60647008903889,-1.37919810936771,-0.467088487340002));
#26194=CARTESIAN_POINT('Ctrl Pts',(0.386357124185273,-1.4508074407617,-0.479477250885268));
#26195=CARTESIAN_POINT('Ctrl Pts',(0.310096596107869,-1.46927193141189,
-0.483634056530725));
#26196=CARTESIAN_POINT('Ctrl Pts',(0.155734301255375,-1.49385305411899,
-0.491814027433449));
#26197=CARTESIAN_POINT('Ctrl Pts',(0.0779900951438741,-1.49993525515011,
-0.495804300368557));
#26198=CARTESIAN_POINT('Ctrl Pts',(-5.94856812385146E-6,-1.49980089084043,
-0.499887533576674));
#26199=CARTESIAN_POINT('Origin',(0.,0.,-0.1394337567297));
#26200=CARTESIAN_POINT('Ctrl Pts',(0.744968168489605,0.832275826917867,
-0.0288675134594948));
#26201=CARTESIAN_POINT('Ctrl Pts',(0.820536075581119,0.772694075545469,
-0.0323343597996823));
#26202=CARTESIAN_POINT('Ctrl Pts',(0.888319065033549,0.703527584149935,
-0.0358520130386424));
#26203=CARTESIAN_POINT('Ctrl Pts',(1.00420116625598,0.549722060754537,-0.0426018521374664));
#26204=CARTESIAN_POINT('Ctrl Pts',(1.05194671393374,0.46548854388906,-0.0458014910649413));
#26205=CARTESIAN_POINT('Ctrl Pts',(1.14548142269179,0.238999221444348,-0.054093189900224));
#26206=CARTESIAN_POINT('Ctrl Pts',(1.17559157541332,0.0910515767618189,
-0.0593081637429571));
#26207=CARTESIAN_POINT('Ctrl Pts',(1.17898019787369,-0.232090382779026,
-0.0704113096782213));
#26208=CARTESIAN_POINT('Ctrl Pts',(1.14154010388872,-0.385690419769286,
-0.0752717872232544));
#26209=CARTESIAN_POINT('Ctrl Pts',(1.03572750735375,-0.649696928154135,
-0.0845969547332541));
#26210=CARTESIAN_POINT('Ctrl Pts',(0.951156135418845,-0.787109400527422,
-0.0900526791622705));
#26211=CARTESIAN_POINT('Ctrl Pts',(0.721634288848172,-1.02225749613246,
-0.100562262399528));
#26212=CARTESIAN_POINT('Ctrl Pts',(0.588532898986576,-1.11363889948885,
-0.105377071715436));
#26213=CARTESIAN_POINT('Ctrl Pts',(0.315871721161606,-1.23373464302002,
-0.114890369640727));
#26214=CARTESIAN_POINT('Ctrl Pts',(0.151790440261885,-1.28133896397508,
-0.120398971070755));
#26215=CARTESIAN_POINT('Ctrl Pts',(-0.207688164228471,-1.28803319903162,
-0.131225510153154));
#26216=CARTESIAN_POINT('Ctrl Pts',(-0.372096471593029,-1.25929311503737,
-0.136137657132471));
#26217=CARTESIAN_POINT('Ctrl Pts',(-0.606449248409185,-1.17134130497118,
-0.143909249049979));
#26218=CARTESIAN_POINT('Ctrl Pts',(-0.683635266369702,-1.13344733995681,
-0.146588319384348));
#26219=CARTESIAN_POINT('Ctrl Pts',(-0.898762753693144,-0.999992061462493,
-0.154209401247211));
#26220=CARTESIAN_POINT('Ctrl Pts',(-1.023045689868,-0.884666880895479,-0.158861114127343));
#26221=CARTESIAN_POINT('Ctrl Pts',(-1.21499816253587,-0.62701520519118,
-0.168345093070664));
#26222=CARTESIAN_POINT('Ctrl Pts',(-1.30322421937978,-0.465133468706287,
-0.173954548293179));
#26223=CARTESIAN_POINT('Ctrl Pts',(-1.396098871979,-0.0890189253362162,
-0.184883028428706));
#26224=CARTESIAN_POINT('Ctrl Pts',(-1.40428952685201,0.094383696364421,
-0.189840736254647));
#26225=CARTESIAN_POINT('Ctrl Pts',(-1.36457053643431,0.36492990957595,-0.197751935705949));
#26226=CARTESIAN_POINT('Ctrl Pts',(-1.34218706524158,0.454984701466365,
-0.200460993435208));
#26227=CARTESIAN_POINT('Ctrl Pts',(-1.24640900146056,0.72334716682606,-0.208556259828602));
#26228=CARTESIAN_POINT('Ctrl Pts',(-1.14970150719883,0.875992371981236,
-0.213147597428451));
#26229=CARTESIAN_POINT('Ctrl Pts',(-0.927851456015851,1.13067058341069,
-0.222414304614733));
#26230=CARTESIAN_POINT('Ctrl Pts',(-0.777605907604323,1.25562501836106,
-0.228009361355914));
#26231=CARTESIAN_POINT('Ctrl Pts',(-0.499086218409759,1.39290411763667,
-0.236270142180347));
#26232=CARTESIAN_POINT('Ctrl Pts',(-0.404620071502844,1.42784380035548,
-0.238844364349628));
#26233=CARTESIAN_POINT('Ctrl Pts',(-0.206951338718649,1.479122751139,-0.244181282610545));
#26234=CARTESIAN_POINT('Ctrl Pts',(-0.103809416887393,1.49470151933882,
-0.246943115301072));
#26235=CARTESIAN_POINT('Ctrl Pts',(-5.49227227915165E-5,1.49958368796161,
-0.249759642713153));
#26236=CARTESIAN_POINT('Ctrl Pts',(0.4476762729852,1.446154421709,0.2341132162814));
#26237=CARTESIAN_POINT('Ctrl Pts',(0.780837923908,1.343019815924,0.2157803457397));
#26238=CARTESIAN_POINT('Ctrl Pts',(1.371452992187,0.8976671939028,0.1791146046562));
#26239=CARTESIAN_POINT('Ctrl Pts',(1.629094976531,-0.1827030763265,0.1241159930311));
#26240=CARTESIAN_POINT('Ctrl Pts',(1.138753746462,-1.179126191151,0.06911738140596));
#26241=CARTESIAN_POINT('Ctrl Pts',(0.1258625640595,-1.634413387851,0.01411876978083));
#26242=CARTESIAN_POINT('Ctrl Pts',(-0.9448155158217,-1.339577634668,-0.0408798418443));
#26243=CARTESIAN_POINT('Ctrl Pts',(-1.581863387021,-0.4299428555337,-0.09587845346944));
#26244=CARTESIAN_POINT('Ctrl Pts',(-1.492914631311,0.6770152357909,-0.1508770650946));
#26245=CARTESIAN_POINT('Ctrl Pts',(-0.7187903802255,1.47325619137,-0.2058756767197));
#26246=CARTESIAN_POINT('Ctrl Pts',(0.385223516623,1.593344378308,-0.2608742883448));
#26247=CARTESIAN_POINT('Ctrl Pts',(1.312438620817,0.9821651256391,-0.31587289997));
#26248=CARTESIAN_POINT('Ctrl Pts',(1.637308341563,-0.07978005883413,-0.3708715115951));
#26249=CARTESIAN_POINT('Ctrl Pts',(1.210733317465,-1.105110084454,-0.4258701232202));
#26250=CARTESIAN_POINT('Ctrl Pts',(0.2284906959225,-1.623248430244,-0.4808687348454));
#26251=CARTESIAN_POINT('Ctrl Pts',(-0.858618021139,-1.396394843238,-0.5358673464705));
#26252=CARTESIAN_POINT('Ctrl Pts',(-1.551662904744,-0.5286640658313,-0.5908659580956));
#26253=CARTESIAN_POINT('Ctrl Pts',(-1.532570123523,0.5816977573753,-0.6458645697208));
#26254=CARTESIAN_POINT('Ctrl Pts',(-0.8101023337328,1.425088654555,-0.7008631813459));
#26255=CARTESIAN_POINT('Ctrl Pts',(0.2841629530904,1.614433300121,-0.755861792971));
#26256=CARTESIAN_POINT('Ctrl Pts',(1.24801129092,1.062831728049,-0.8108604045962));
#26257=CARTESIAN_POINT('Ctrl Pts',(1.639083258684,0.02344218173783,-0.8658590162213));
#26258=CARTESIAN_POINT('Ctrl Pts',(1.27789587838,-1.026706183462,-0.9208576278464));
#26259=CARTESIAN_POINT('Ctrl Pts',(0.3302165605045,-1.605646440099,-0.9758562394716));
#26260=CARTESIAN_POINT('Ctrl Pts',(-0.7690160758597,-1.447673216135,-1.030854851097));
#26261=CARTESIAN_POINT('Ctrl Pts',(-1.515307776415,-0.6252885404762,-1.085853462722));
#26262=CARTESIAN_POINT('Ctrl Pts',(-1.566147153266,0.4840731558256,-1.140852074347));
#26263=CARTESIAN_POINT('Ctrl Pts',(-0.8982008953502,1.371268677471,-1.195850685972));
#26264=CARTESIAN_POINT('Ctrl Pts',(0.1819742926137,1.629119380239,-1.250849297597));
#26265=CARTESIAN_POINT('Ctrl Pts',(1.178637797514,1.139281110916,-1.305847909222));
#26266=CARTESIAN_POINT('Ctrl Pts',(1.634342898764,0.1265778772082,-1.360846520848));
#26267=CARTESIAN_POINT('Ctrl Pts',(1.340042942684,-0.9442540804366,-1.415845132473));
#26268=CARTESIAN_POINT('Ctrl Pts',(0.4304348753708,-1.581586393104,-1.470843744098));
#26269=CARTESIAN_POINT('Ctrl Pts',(-0.3069388631827,-1.522891533776,-1.507509485181));
#26270=CARTESIAN_POINT('Ctrl Pts',(-0.624627630162,-1.37899129093,-1.525842355723));
#26271=CARTESIAN_POINT('Ctrl Pts',(0.4071889425826,1.315365868868,0.1550670916087));
#26272=CARTESIAN_POINT('Ctrl Pts',(0.7102198346237,1.22155863894,0.136734221067));
#26273=CARTESIAN_POINT('Ctrl Pts',(1.247420351243,0.8164831989845,0.1000684799836));
#26274=CARTESIAN_POINT('Ctrl Pts',(1.481761489027,-0.1661796189463,0.04506986835845));
#26275=CARTESIAN_POINT('Ctrl Pts',(1.03576615931,-1.072487366249,-0.00992874326668));
#26276=CARTESIAN_POINT('Ctrl Pts',(0.1144796976359,-1.486598909306,-0.06492735489181));
#26277=CARTESIAN_POINT('Ctrl Pts',(-0.859367480563,-1.218427764623,-0.1199259665169));
#26278=CARTESIAN_POINT('Ctrl Pts',(-1.438801470482,-0.3910593151348,-0.1749245781421));
#26279=CARTESIAN_POINT('Ctrl Pts',(-1.357897138564,0.6157867517431,-0.2299231897672));
#26280=CARTESIAN_POINT('Ctrl Pts',(-0.653783799867,1.340016585461,-0.2849218013923));
#26281=CARTESIAN_POINT('Ctrl Pts',(0.3503843421178,1.449244134041,-0.3399204130175));
#26282=CARTESIAN_POINT('Ctrl Pts',(1.193743172162,0.8933392343618,-0.3949190246426));
#26283=CARTESIAN_POINT('Ctrl Pts',(1.489232046713,-0.07256484150752,-0.4499176362677));
#26284=CARTESIAN_POINT('Ctrl Pts',(1.101235980189,-1.005165191637,-0.5049162478929));
#26285=CARTESIAN_POINT('Ctrl Pts',(0.2078262585646,-1.476443697703,-0.559914859518));
#26286=CARTESIAN_POINT('Ctrl Pts',(-0.7809655887694,-1.270106489796,-0.6149134711432));
#26287=CARTESIAN_POINT('Ctrl Pts',(-1.411332285301,-0.4808522920186,-0.6699120827683));
#26288=CARTESIAN_POINT('Ctrl Pts',(-1.393966233389,0.5290896771207,-0.7249106943934));
#26289=CARTESIAN_POINT('Ctrl Pts',(-0.7368376046753,1.296205265616,-0.7799093060186));
#26290=CARTESIAN_POINT('Ctrl Pts',(0.2584635804317,1.468425797871,-0.8349079176437));
#26291=CARTESIAN_POINT('Ctrl Pts',(1.135142576336,0.9667104414579,-0.8899065292688));
#26292=CARTESIAN_POINT('Ctrl Pts',(1.490846442359,0.02132209761756,-0.944905140894));
#26293=CARTESIAN_POINT('Ctrl Pts',(1.162324435866,-0.9338520498285,-0.9999037525191));
#26294=CARTESIAN_POINT('Ctrl Pts',(0.3003521522337,-1.460433611426,-1.054902364144));
#26295=CARTESIAN_POINT('Ctrl Pts',(-0.6994671409997,-1.316747305262,-1.109900975769));
#26296=CARTESIAN_POINT('Ctrl Pts',(-1.378265073222,-0.5687381596254,-1.164899587394));
#26297=CARTESIAN_POINT('Ctrl Pts',(-1.424506594944,0.4402941329432,-1.21989819902));
#26298=CARTESIAN_POINT('Ctrl Pts',(-0.816968633083,1.247252705739,-1.274896810645));
#26299=CARTESIAN_POINT('Ctrl Pts',(0.1655167455995,1.481783685691,-1.32989542227));
#26300=CARTESIAN_POINT('Ctrl Pts',(1.072043142374,1.036245829525,-1.384894033895));
#26301=CARTESIAN_POINT('Ctrl Pts',(1.486534795172,0.1151303186811,-1.43989264552));
#26302=CARTESIAN_POINT('Ctrl Pts',(1.218850990713,-0.8588568207524,-1.494891257145));
#26303=CARTESIAN_POINT('Ctrl Pts',(0.3915068372603,-1.438549527579,-1.54988986877));
#26304=CARTESIAN_POINT('Ctrl Pts',(-0.2791796632497,-1.385162964236,-1.586555609854));
#26305=CARTESIAN_POINT('Ctrl Pts',(-0.5681370212845,-1.254276894864,-1.604888480396));
#26306=CARTESIAN_POINT('Ctrl Pts',(0.3667016121801,1.184577316028,0.07602096693608));
#26307=CARTESIAN_POINT('Ctrl Pts',(0.6396017453395,1.100097461957,0.05768809639437));
#26308=CARTESIAN_POINT('Ctrl Pts',(1.1233877103,0.7352992040661,0.02102235531094));
#26309=CARTESIAN_POINT('Ctrl Pts',(1.334428001522,-0.1496561615661,-0.03397625631419));
#26310=CARTESIAN_POINT('Ctrl Pts',(0.9327785721571,-0.9658485413479,-0.08897486793932));
#26311=CARTESIAN_POINT('Ctrl Pts',(0.1030968312124,-1.338784430761,-0.1439734795645));
#26312=CARTESIAN_POINT('Ctrl Pts',(-0.7739194453042,-1.097277894577,-0.1989720911896));
#26313=CARTESIAN_POINT('Ctrl Pts',(-1.295739553944,-0.352175774736,-0.2539707028147));
#26314=CARTESIAN_POINT('Ctrl Pts',(-1.222879645817,0.5545582676954,-0.3089693144399));
#26315=CARTESIAN_POINT('Ctrl Pts',(-0.5887772195086,1.206776979551,-0.363967926065));
#26316=CARTESIAN_POINT('Ctrl Pts',(0.3155451676127,1.305143889774,-0.4189665376901));
#26317=CARTESIAN_POINT('Ctrl Pts',(1.075047723507,0.8045133430845,-0.4739651493153));
#26318=CARTESIAN_POINT('Ctrl Pts',(1.341155751864,-0.06534962418092,-0.5289637609404));
#26319=CARTESIAN_POINT('Ctrl Pts',(0.9917386429129,-0.9052202988191,-0.5839623725655));
#26320=CARTESIAN_POINT('Ctrl Pts',(0.1871618212067,-1.329638965161,-0.6389609841907));
#26321=CARTESIAN_POINT('Ctrl Pts',(-0.7033131563998,-1.143818136353,-0.6939595958158));
#26322=CARTESIAN_POINT('Ctrl Pts',(-1.271001665859,-0.433040518206,-0.7489582074409));
#26323=CARTESIAN_POINT('Ctrl Pts',(-1.255362343256,0.4764815968661,-0.8039568190661));
#26324=CARTESIAN_POINT('Ctrl Pts',(-0.6635728756178,1.167321876677,-0.8589554306912));
#26325=CARTESIAN_POINT('Ctrl Pts',(0.2327642077729,1.322418295622,-0.9139540423163));
#26326=CARTESIAN_POINT('Ctrl Pts',(1.022273861752,0.8705891548663,-0.9689526539415));
#26327=CARTESIAN_POINT('Ctrl Pts',(1.342609626034,0.01920201349729,-1.023951265567));
#26328=CARTESIAN_POINT('Ctrl Pts',(1.046752993353,-0.8409979161953,-1.078949877192));
#26329=CARTESIAN_POINT('Ctrl Pts',(0.270487743963,-1.315220782753,-1.133948488817));
#26330=CARTESIAN_POINT('Ctrl Pts',(-0.6299182061397,-1.18582139439,-1.188947100442));
#26331=CARTESIAN_POINT('Ctrl Pts',(-1.241222370029,-0.5121877787746,-1.243945712067));
#26332=CARTESIAN_POINT('Ctrl Pts',(-1.282866036621,0.3965151100608,-1.298944323692));
#26333=CARTESIAN_POINT('Ctrl Pts',(-0.7357363708159,1.123236734008,-1.353942935317));
#26334=CARTESIAN_POINT('Ctrl Pts',(0.1490591985852,1.334447991143,-1.408941546943));
#26335=CARTESIAN_POINT('Ctrl Pts',(0.9654484872351,0.933210548134,-1.463940158568));
#26336=CARTESIAN_POINT('Ctrl Pts',(1.338726691579,0.103682760154,-1.518938770193));
#26337=CARTESIAN_POINT('Ctrl Pts',(1.097659038743,-0.7734595610681,-1.573937381818));
#26338=CARTESIAN_POINT('Ctrl Pts',(0.3525787991498,-1.295512662054,-1.628935993443));
#26339=CARTESIAN_POINT('Ctrl Pts',(-0.2514204633167,-1.247434394696,-1.665601734526));
#26340=CARTESIAN_POINT('Ctrl Pts',(-0.5116464124071,-1.129562498799,-1.683934605068));
#26341=CARTESIAN_POINT('Ctrl Pts',(0.3262142817775,1.053788763187,-0.003025157736566));
#26342=CARTESIAN_POINT('Ctrl Pts',(0.5689836560552,0.9786362849728,-0.02135802827828));
#26343=CARTESIAN_POINT('Ctrl Pts',(0.9993550693557,0.6541152091478,-0.0580237693617));
#26344=CARTESIAN_POINT('Ctrl Pts',(1.187094514017,-0.1331327041859,-0.1130223809868));
#26345=CARTESIAN_POINT('Ctrl Pts',(0.8297909850046,-0.8592097164464,-0.168020992612));
#26346=CARTESIAN_POINT('Ctrl Pts',(0.09171396478879,-1.190969952216,-0.2230196042371));
#26347=CARTESIAN_POINT('Ctrl Pts',(-0.6884714100455,-0.9761280245314,-0.2780182158622));
#26348=CARTESIAN_POINT('Ctrl Pts',(-1.152677637406,-0.3132922343372,-0.3330168274874));
#26349=CARTESIAN_POINT('Ctrl Pts',(-1.08786215307,0.4933297836476,-0.3880154391125));
#26350=CARTESIAN_POINT('Ctrl Pts',(-0.5237706391502,1.073537373642,-0.4430140507376));
#26351=CARTESIAN_POINT('Ctrl Pts',(0.2807059931075,1.161043645508,-0.4980126623628));
#26352=CARTESIAN_POINT('Ctrl Pts',(0.9563522748523,0.7156874518072,-0.5530112739879));
#26353=CARTESIAN_POINT('Ctrl Pts',(1.193079457014,-0.05813440685431,-0.608009885613));
#26354=CARTESIAN_POINT('Ctrl Pts',(0.8822413056368,-0.8052754060015,-0.6630084972382));
#26355=CARTESIAN_POINT('Ctrl Pts',(0.1664973838488,-1.18283423262,-0.7180071088633));
#26356=CARTESIAN_POINT('Ctrl Pts',(-0.6256607240303,-1.017529782911,-0.7730057204884));
#26357=CARTESIAN_POINT('Ctrl Pts',(-1.130671046416,-0.3852287443933,-0.8280043321136));
#26358=CARTESIAN_POINT('Ctrl Pts',(-1.116758453123,0.4238735166115,-0.8830029437387));
#26359=CARTESIAN_POINT('Ctrl Pts',(-0.5903081465603,1.038438487738,-0.9380015553638));
#26360=CARTESIAN_POINT('Ctrl Pts',(0.2070648351141,1.176410793373,-0.993000166989));
#26361=CARTESIAN_POINT('Ctrl Pts',(0.909405147168,0.7744678682747,-1.047998778614));
#26362=CARTESIAN_POINT('Ctrl Pts',(1.194372809709,0.01708192937703,-1.102997390239));
#26363=CARTESIAN_POINT('Ctrl Pts',(0.9311815508389,-0.7481437825621,-1.157996001864));
#26364=CARTESIAN_POINT('Ctrl Pts',(0.2406233356923,-1.17000795408,-1.21299461349));
#26365=CARTESIAN_POINT('Ctrl Pts',(-0.5603692712797,-1.054895483517,-1.267993225115));
#26366=CARTESIAN_POINT('Ctrl Pts',(-1.104179666836,-0.4556373979237,-1.32299183674));
#26367=CARTESIAN_POINT('Ctrl Pts',(-1.141225478299,0.3527360871784,-1.377990448365));
#26368=CARTESIAN_POINT('Ctrl Pts',(-0.6545041085487,0.9992207622761,-1.43298905999));
#26369=CARTESIAN_POINT('Ctrl Pts',(0.1326016515709,1.187112296595,-1.487987671615));
#26370=CARTESIAN_POINT('Ctrl Pts',(0.8588538320959,0.8301752667432,-1.54298628324));
#26371=CARTESIAN_POINT('Ctrl Pts',(1.190918587986,0.09223520162696,-1.597984894865));
#26372=CARTESIAN_POINT('Ctrl Pts',(0.9764670867718,-0.6880623013838,-1.652983506491));
#26373=CARTESIAN_POINT('Ctrl Pts',(0.3136507610394,-1.152475796529,-1.707982118116));
#26374=CARTESIAN_POINT('Ctrl Pts',(-0.2236612633837,-1.109705825156,-1.744647859199));
#26375=CARTESIAN_POINT('Ctrl Pts',(-0.4551558035296,-1.004848102734,-1.762980729741));
#26376=CARTESIAN_POINT('',(0.,-1.5,-1.5));
#26377=CARTESIAN_POINT('Ctrl Pts',(0.644570879197,-1.369782843561,-1.456997056261));
#26378=CARTESIAN_POINT('Ctrl Pts',(0.3182373172226,-1.523343761587,-1.475955389595));
#26379=CARTESIAN_POINT('Ctrl Pts',(-0.4471872711094,-1.586323876419,-1.513872056261));
#26380=CARTESIAN_POINT('Ctrl Pts',(-1.377740014924,-0.904994387625,-1.570747056261));
#26381=CARTESIAN_POINT('Ctrl Pts',(-1.633632209849,0.2194343691702,-1.627622056261));
#26382=CARTESIAN_POINT('Ctrl Pts',(-1.090057677579,1.236420530413,-1.684497056261));
#26383=CARTESIAN_POINT('Ctrl Pts',(-0.01294453477278,1.648269146651,-1.741372056261));
#26384=CARTESIAN_POINT('Ctrl Pts',(1.070497507345,1.253391767652,-1.798247056261));
#26385=CARTESIAN_POINT('Ctrl Pts',(1.630000905225,0.2450597004638,-1.855122056261));
#26386=CARTESIAN_POINT('Ctrl Pts',(1.391722092318,-0.8832137221716,-1.911997056261));
#26387=CARTESIAN_POINT('Ctrl Pts',(0.4722839904274,-1.579210161907,-1.968872056261));
#26388=CARTESIAN_POINT('Ctrl Pts',(-0.6783071100709,-1.502283720031,-2.025747056261));
#26389=CARTESIAN_POINT('Ctrl Pts',(-1.496910028035,-0.6900849750494,-2.082622056261));
#26390=CARTESIAN_POINT('Ctrl Pts',(-1.582870729986,0.4598664577049,-2.139497056261));
#26391=CARTESIAN_POINT('Ctrl Pts',(-0.8941169184215,1.384742518528,-2.196372056261));
#26392=CARTESIAN_POINT('Ctrl Pts',(0.232250236729,1.631875220096,-2.253247056261));
#26393=CARTESIAN_POINT('Ctrl Pts',(1.24494567787,1.080308828809,-2.310122056261));
#26394=CARTESIAN_POINT('Ctrl Pts',(1.648319418813,0.,-2.366997056261));
#26395=CARTESIAN_POINT('Ctrl Pts',(1.24494567787,-1.080308828809,-2.423872056261));
#26396=CARTESIAN_POINT('Ctrl Pts',(0.232250236729,-1.631875220096,-2.480747056261));
#26397=CARTESIAN_POINT('Ctrl Pts',(-0.8941169184215,-1.384742518528,-2.537622056261));
#26398=CARTESIAN_POINT('Ctrl Pts',(-1.582870729986,-0.4598664577049,-2.594497056261));
#26399=CARTESIAN_POINT('Ctrl Pts',(-1.496910028035,0.6900849750494,-2.651372056261));
#26400=CARTESIAN_POINT('Ctrl Pts',(-0.6783071100709,1.502283720031,-2.708247056261));
#26401=CARTESIAN_POINT('Ctrl Pts',(0.4722839904274,1.579210161907,-2.765122056261));
#26402=CARTESIAN_POINT('Ctrl Pts',(1.391722092317,0.8832137221716,-2.821997056261));
#26403=CARTESIAN_POINT('Ctrl Pts',(1.630000905225,-0.2450597004637,-2.878872056261));
#26404=CARTESIAN_POINT('Ctrl Pts',(1.070497507345,-1.253391767652,-2.935747056261));
#26405=CARTESIAN_POINT('Ctrl Pts',(-0.01294453477277,-1.648269146651,-2.992622056261));
#26406=CARTESIAN_POINT('Ctrl Pts',(-1.090057677579,-1.236420530413,-3.049497056261));
#26407=CARTESIAN_POINT('Ctrl Pts',(-1.633632209849,-0.2194343691702,-3.106372056261));
#26408=CARTESIAN_POINT('Ctrl Pts',(-1.377740014924,0.904994387625,-3.163247056261));
#26409=CARTESIAN_POINT('Ctrl Pts',(-0.4471872711094,1.586323876419,-3.220122056261));
#26410=CARTESIAN_POINT('Ctrl Pts',(0.3182373172226,1.523343761587,-3.258038722928));
#26411=CARTESIAN_POINT('Ctrl Pts',(0.644570879197,1.369782843561,-3.276997056261));
#26412=CARTESIAN_POINT('Ctrl Pts',(0.5862766256734,-1.24590124895,-1.536043180934));
#26413=CARTESIAN_POINT('Ctrl Pts',(0.2894562980212,-1.38557429308,-1.555001514267));
#26414=CARTESIAN_POINT('Ctrl Pts',(-0.4067441654775,-1.442858558319,-1.592918180934));
#26415=CARTESIAN_POINT('Ctrl Pts',(-1.253138782831,-0.823147729682,-1.649793180934));
#26416=CARTESIAN_POINT('Ctrl Pts',(-1.48588838015,0.1995889756518,-1.706668180934));
#26417=CARTESIAN_POINT('Ctrl Pts',(-0.9914741072328,1.12460007096,-1.763543180934));
#26418=CARTESIAN_POINT('Ctrl Pts',(-0.01177384584446,1.499201569118,-1.820418180934));
#26419=CARTESIAN_POINT('Ctrl Pts',(0.9736829364363,1.140036448902,-1.877293180934));
#26420=CARTESIAN_POINT('Ctrl Pts',(1.482585486565,0.2228967812747,-1.934168180934));
#26421=CARTESIAN_POINT('Ctrl Pts',(1.265856337127,-0.8033368827153,-1.991043180934));
#26422=CARTESIAN_POINT('Ctrl Pts',(0.4295711661878,-1.436388200015,-2.047918180934));
#26423=CARTESIAN_POINT('Ctrl Pts',(-0.61696179039,-1.36641889761,-2.104793180934));
#26424=CARTESIAN_POINT('Ctrl Pts',(-1.361531196175,-0.6276744787227,-2.161668180934));
#26425=CARTESIAN_POINT('Ctrl Pts',(-1.439717710501,0.4182766609306,-2.218543180934));
#26426=CARTESIAN_POINT('Ctrl Pts',(-0.8132540063595,1.259507988013,-2.275418180934));
#26427=CARTESIAN_POINT('Ctrl Pts',(0.211245790798,1.484290290542,-2.332293180934));
#26428=CARTESIAN_POINT('Ctrl Pts',(1.132354213826,0.9826069332027,-2.389168180934));
#26429=CARTESIAN_POINT('Ctrl Pts',(1.499247294724,0.,-2.446043180934));
#26430=CARTESIAN_POINT('Ctrl Pts',(1.132354213826,-0.9826069332027,-2.502918180934));
#26431=CARTESIAN_POINT('Ctrl Pts',(0.211245790798,-1.484290290542,-2.559793180934));
#26432=CARTESIAN_POINT('Ctrl Pts',(-0.8132540063595,-1.259507988013,-2.616668180934));
#26433=CARTESIAN_POINT('Ctrl Pts',(-1.439717710501,-0.4182766609306,-2.673543180934));
#26434=CARTESIAN_POINT('Ctrl Pts',(-1.361531196175,0.6276744787227,-2.730418180934));
#26435=CARTESIAN_POINT('Ctrl Pts',(-0.61696179039,1.36641889761,-2.787293180934));
#26436=CARTESIAN_POINT('Ctrl Pts',(0.4295711661878,1.436388200015,-2.844168180934));
#26437=CARTESIAN_POINT('Ctrl Pts',(1.265856337127,0.8033368827153,-2.901043180934));
#26438=CARTESIAN_POINT('Ctrl Pts',(1.482585486565,-0.2228967812747,-2.957918180934));
#26439=CARTESIAN_POINT('Ctrl Pts',(0.9736829364363,-1.140036448902,-3.014793180934));
#26440=CARTESIAN_POINT('Ctrl Pts',(-0.01177384584446,-1.499201569118,-3.071668180934));
#26441=CARTESIAN_POINT('Ctrl Pts',(-0.9914741072328,-1.12460007096,-3.128543180934));
#26442=CARTESIAN_POINT('Ctrl Pts',(-1.48588838015,-0.1995889756517,-3.185418180934));
#26443=CARTESIAN_POINT('Ctrl Pts',(-1.253138782831,0.823147729682,-3.242293180934));
#26444=CARTESIAN_POINT('Ctrl Pts',(-0.4067441654775,1.442858558319,-3.299168180934));
#26445=CARTESIAN_POINT('Ctrl Pts',(0.2894562980212,1.38557429308,-3.337084847601));
#26446=CARTESIAN_POINT('Ctrl Pts',(0.5862766256734,1.24590124895,-3.356043180934));
#26447=CARTESIAN_POINT('Ctrl Pts',(0.5279823721497,-1.122019654338,-1.615089305607));
#26448=CARTESIAN_POINT('Ctrl Pts',(0.2606752788197,-1.247804824574,-1.63404763894));
#26449=CARTESIAN_POINT('Ctrl Pts',(-0.3663010598456,-1.299393240218,-1.671964305607));
#26450=CARTESIAN_POINT('Ctrl Pts',(-1.128537550737,-0.7413010717389,-1.728839305607));
#26451=CARTESIAN_POINT('Ctrl Pts',(-1.33814455045,0.1797435821333,-1.785714305607));
#26452=CARTESIAN_POINT('Ctrl Pts',(-0.892890536887,1.012779611507,-1.842589305607));
#26453=CARTESIAN_POINT('Ctrl Pts',(-0.01060315691615,1.350133991585,-1.899464305607));
#26454=CARTESIAN_POINT('Ctrl Pts',(0.8768683655278,1.026681130153,-1.956339305607));
#26455=CARTESIAN_POINT('Ctrl Pts',(1.335170067905,0.2007338620856,-2.013214305607));
#26456=CARTESIAN_POINT('Ctrl Pts',(1.139990581936,-0.723460043259,-2.070089305607));
#26457=CARTESIAN_POINT('Ctrl Pts',(0.3868583419482,-1.293566238123,-2.126964305607));
#26458=CARTESIAN_POINT('Ctrl Pts',(-0.555616470709,-1.230554075189,-2.183839305607));
#26459=CARTESIAN_POINT('Ctrl Pts',(-1.226152364316,-0.5652639823961,-2.240714305607));
#26460=CARTESIAN_POINT('Ctrl Pts',(-1.296564691016,0.3766868641562,-2.297589305607));
#26461=CARTESIAN_POINT('Ctrl Pts',(-0.7323910942975,1.134273457497,-2.354464305607));
#26462=CARTESIAN_POINT('Ctrl Pts',(0.190241344867,1.336705360987,-2.411339305607));
#26463=CARTESIAN_POINT('Ctrl Pts',(1.019762749782,0.8849050375959,-2.468214305607));
#26464=CARTESIAN_POINT('Ctrl Pts',(1.350175170634,0.,-2.525089305607));
#26465=CARTESIAN_POINT('Ctrl Pts',(1.019762749782,-0.8849050375959,-2.581964305607));
#26466=CARTESIAN_POINT('Ctrl Pts',(0.190241344867,-1.336705360987,-2.638839305607));
#26467=CARTESIAN_POINT('Ctrl Pts',(-0.7323910942975,-1.134273457497,-2.695714305607));
#26468=CARTESIAN_POINT('Ctrl Pts',(-1.296564691016,-0.3766868641562,-2.752589305607));
#26469=CARTESIAN_POINT('Ctrl Pts',(-1.226152364316,0.5652639823961,-2.809464305607));
#26470=CARTESIAN_POINT('Ctrl Pts',(-0.555616470709,1.230554075189,-2.866339305607));
#26471=CARTESIAN_POINT('Ctrl Pts',(0.3868583419482,1.293566238123,-2.923214305607));
#26472=CARTESIAN_POINT('Ctrl Pts',(1.139990581936,0.723460043259,-2.980089305607));
#26473=CARTESIAN_POINT('Ctrl Pts',(1.335170067905,-0.2007338620856,-3.036964305607));
#26474=CARTESIAN_POINT('Ctrl Pts',(0.8768683655278,-1.026681130153,-3.093839305607));
#26475=CARTESIAN_POINT('Ctrl Pts',(-0.01060315691615,-1.350133991585,-3.150714305607));
#26476=CARTESIAN_POINT('Ctrl Pts',(-0.892890536887,-1.012779611507,-3.207589305607));
#26477=CARTESIAN_POINT('Ctrl Pts',(-1.33814455045,-0.1797435821333,-3.264464305607));
#26478=CARTESIAN_POINT('Ctrl Pts',(-1.128537550737,0.7413010717389,-3.321339305607));
#26479=CARTESIAN_POINT('Ctrl Pts',(-0.3663010598456,1.299393240218,-3.378214305607));
#26480=CARTESIAN_POINT('Ctrl Pts',(0.2606752788197,1.247804824574,-3.416130972273));
#26481=CARTESIAN_POINT('Ctrl Pts',(0.5279823721497,1.122019654338,-3.435089305607));
#26482=CARTESIAN_POINT('Ctrl Pts',(0.4696881186261,-0.9981380597272,-1.694135430279));
#26483=CARTESIAN_POINT('Ctrl Pts',(0.2318942596183,-1.110035356068,-1.713093763613));
#26484=CARTESIAN_POINT('Ctrl Pts',(-0.3258579542137,-1.155927922117,-1.751010430279));
#26485=CARTESIAN_POINT('Ctrl Pts',(-1.003936318643,-0.6594544137959,-1.807885430279));
#26486=CARTESIAN_POINT('Ctrl Pts',(-1.190400720751,0.1598981886148,-1.864760430279));
#26487=CARTESIAN_POINT('Ctrl Pts',(-0.7943069665412,0.9009591520544,-1.921635430279));
#26488=CARTESIAN_POINT('Ctrl Pts',(-0.009432467987834,1.201066414053,-1.978510430279));
#26489=CARTESIAN_POINT('Ctrl Pts',(0.7800537946193,0.9133258114035,-2.035385430279));
#26490=CARTESIAN_POINT('Ctrl Pts',(1.187754649245,0.1785709428966,-2.092260430279));
#26491=CARTESIAN_POINT('Ctrl Pts',(1.014124826746,-0.6435832038027,-2.149135430279));
#26492=CARTESIAN_POINT('Ctrl Pts',(0.3441455177085,-1.150744276231,-2.206010430279));
#26493=CARTESIAN_POINT('Ctrl Pts',(-0.4942711510281,-1.094689252768,-2.262885430279));
#26494=CARTESIAN_POINT('Ctrl Pts',(-1.090773532456,-0.5028534860695,-2.319760430279));
#26495=CARTESIAN_POINT('Ctrl Pts',(-1.153411671532,0.3350970673819,-2.376635430279));
#26496=CARTESIAN_POINT('Ctrl Pts',(-0.6515281822355,1.009038926982,-2.433510430279));
#26497=CARTESIAN_POINT('Ctrl Pts',(0.169236898936,1.189120431432,-2.490385430279));
#26498=CARTESIAN_POINT('Ctrl Pts',(0.9071712857378,0.7872031419892,-2.547260430279));
#26499=CARTESIAN_POINT('Ctrl Pts',(1.201103046544,0.,-2.604135430279));
#26500=CARTESIAN_POINT('Ctrl Pts',(0.9071712857378,-0.7872031419892,-2.661010430279));
#26501=CARTESIAN_POINT('Ctrl Pts',(0.169236898936,-1.189120431432,-2.717885430279));
#26502=CARTESIAN_POINT('Ctrl Pts',(-0.6515281822355,-1.009038926982,-2.774760430279));
#26503=CARTESIAN_POINT('Ctrl Pts',(-1.153411671532,-0.3350970673819,-2.831635430279));
#26504=CARTESIAN_POINT('Ctrl Pts',(-1.090773532456,0.5028534860695,-2.888510430279));
#26505=CARTESIAN_POINT('Ctrl Pts',(-0.4942711510281,1.094689252768,-2.945385430279));
#26506=CARTESIAN_POINT('Ctrl Pts',(0.3441455177085,1.150744276231,-3.002260430279));
#26507=CARTESIAN_POINT('Ctrl Pts',(1.014124826746,0.6435832038027,-3.059135430279));
#26508=CARTESIAN_POINT('Ctrl Pts',(1.187754649245,-0.1785709428966,-3.116010430279));
#26509=CARTESIAN_POINT('Ctrl Pts',(0.7800537946193,-0.9133258114035,-3.172885430279));
#26510=CARTESIAN_POINT('Ctrl Pts',(-0.009432467987832,-1.201066414053,-3.229760430279));
#26511=CARTESIAN_POINT('Ctrl Pts',(-0.7943069665412,-0.9009591520544,-3.286635430279));
#26512=CARTESIAN_POINT('Ctrl Pts',(-1.190400720751,-0.1598981886148,-3.343510430279));
#26513=CARTESIAN_POINT('Ctrl Pts',(-1.003936318643,0.6594544137959,-3.400385430279));
#26514=CARTESIAN_POINT('Ctrl Pts',(-0.3258579542138,1.155927922117,-3.457260430279));
#26515=CARTESIAN_POINT('Ctrl Pts',(0.2318942596183,1.110035356068,-3.495177096946));
#26516=CARTESIAN_POINT('Ctrl Pts',(0.4696881186261,0.9981380597272,-3.514135430279));
#26517=CARTESIAN_POINT('',(1.98293436067666E-9,1.49923261688425,-3.25044299895813));
#26518=CARTESIAN_POINT('Ctrl Pts',(2.06854461059408E-5,-1.49901358627223,
-1.99995486355702));
#26519=CARTESIAN_POINT('Ctrl Pts',(-0.0953214838110155,-1.49902491199573,
-2.00491761318046));
#26520=CARTESIAN_POINT('Ctrl Pts',(-0.190691030216163,-1.49011947635382,
-2.0098913899261));
#26521=CARTESIAN_POINT('Ctrl Pts',(-0.37249893387041,-1.45546670386657,
-2.0197305237836));
#26522=CARTESIAN_POINT('Ctrl Pts',(-0.458525227544424,-1.43085386099099,
-2.02459116547238));
#26523=CARTESIAN_POINT('Ctrl Pts',(-0.722446426617393,-1.32838383657233,
-2.04004693335259));
#26524=CARTESIAN_POINT('Ctrl Pts',(-0.86645493380528,-1.23164641754706,
-2.04893369151967));
#26525=CARTESIAN_POINT('Ctrl Pts',(-1.06600265467772,-1.06039735381172,
-2.0626050331301));
#26526=CARTESIAN_POINT('Ctrl Pts',(-1.1468383556571,-0.972980331374049,
-2.06875630933358));
#26527=CARTESIAN_POINT('Ctrl Pts',(-1.29967423550166,-0.762168700625944,
-2.08268102999226));
#26528=CARTESIAN_POINT('Ctrl Pts',(-1.36539620478645,-0.636646697395617,
-2.09046986466724));
#26529=CARTESIAN_POINT('Ctrl Pts',(-1.44568091735312,-0.409137312958668,
-2.10325803431831));
#26530=CARTESIAN_POINT('Ctrl Pts',(-1.46940771045106,-0.31232155032306,
-2.10841762364369));
#26531=CARTESIAN_POINT('Ctrl Pts',(-1.50054215939577,-0.0968012311816991,
-2.11974762234642));
#26532=CARTESIAN_POINT('Ctrl Pts',(-1.50386336583337,0.0225864242432771,
-2.1259279009948));
#26533=CARTESIAN_POINT('Ctrl Pts',(-1.48028992278847,0.279075253883525,
-2.13972651028424));
#26534=CARTESIAN_POINT('Ctrl Pts',(-1.44824876150154,0.4138678742304,-2.14734526453954));
#26535=CARTESIAN_POINT('Ctrl Pts',(-1.36138274914138,0.635627037820876,
-2.15997498794209));
#26536=CARTESIAN_POINT('Ctrl Pts',(-1.31601337842939,0.724432162573865,
-2.16513698024779));
#26537=CARTESIAN_POINT('Ctrl Pts',(-1.19858130700141,0.907957044093622,
-2.17647071223724));
#26538=CARTESIAN_POINT('Ctrl Pts',(-1.12297157880735,1.00051622230357,-2.18265174258831));
#26539=CARTESIAN_POINT('Ctrl Pts',(-0.935510734630244,1.18096930350524,
-2.19658311814016));
#26540=CARTESIAN_POINT('Ctrl Pts',(-0.820853703812189,1.26317291479198,
-2.2043395207105));
#26541=CARTESIAN_POINT('Ctrl Pts',(-0.607361198665937,1.3742110709498,-2.21709317469487));
#26542=CARTESIAN_POINT('Ctrl Pts',(-0.51481950301746,1.41125178892119,-2.22225152016787));
#26543=CARTESIAN_POINT('Ctrl Pts',(-0.306211258634909,1.47211310867909,
-2.23355595013963));
#26544=CARTESIAN_POINT('Ctrl Pts',(-0.188926596877854,1.49208312971459,
-2.23971190758978));
#26545=CARTESIAN_POINT('Ctrl Pts',(0.0670817760636266,1.50479893204463,
-2.25344188021204));
#26546=CARTESIAN_POINT('Ctrl Pts',(0.204264061836362,1.49224160547224,-2.26101759022915));
#26547=CARTESIAN_POINT('Ctrl Pts',(0.435383240177761,1.43800305381027,-2.27361014831976));
#26548=CARTESIAN_POINT('Ctrl Pts',(0.529759724211701,1.40572556203723,-2.27877412817635));
#26549=CARTESIAN_POINT('Ctrl Pts',(0.728440094304206,1.31545684930317,-2.29012620086494));
#26550=CARTESIAN_POINT('Ctrl Pts',(0.831081185798915,1.25358147405109,-2.29632332229973));
#26551=CARTESIAN_POINT('Ctrl Pts',(1.03747315158837,1.09264013452201,-2.31033406844491));
#26552=CARTESIAN_POINT('Ctrl Pts',(1.13578892642221,0.989806391524517,-2.31815505599114));
#26553=CARTESIAN_POINT('Ctrl Pts',(1.27616339680962,0.792923500200331,-2.33096631701669));
#26554=CARTESIAN_POINT('Ctrl Pts',(1.32572981587352,0.706468967378648,-2.33612261921326));
#26555=CARTESIAN_POINT('Ctrl Pts',(1.41494914035029,0.508669815652517,-2.34741077045875));
#26556=CARTESIAN_POINT('Ctrl Pts',(1.45101571447836,0.395608673694945,-2.35355276851213));
#26557=CARTESIAN_POINT('Ctrl Pts',(1.49905455000177,0.145868247220176,-2.36717831536221));
#26558=CARTESIAN_POINT('Ctrl Pts',(1.50597375104993,0.00999053376861738,
-2.37466154019217));
#26559=CARTESIAN_POINT('Ctrl Pts',(1.48555860957949,-0.224860674032068,
-2.38717178661232));
#26560=CARTESIAN_POINT('Ctrl Pts',(1.46712396673904,-0.322920215350939,
-2.39233879547481));
#26561=CARTESIAN_POINT('Ctrl Pts',(1.40609716643204,-0.532947437374544,
-2.40371621536761));
#26562=CARTESIAN_POINT('Ctrl Pts',(1.35932684529135,-0.643798827201405,
-2.40993516379191));
#26563=CARTESIAN_POINT('Ctrl Pts',(1.22813604202715,-0.873215485968569,
-2.42407803827426));
#26564=CARTESIAN_POINT('Ctrl Pts',(1.13881445511511,-0.986617888171145,
-2.43201228151042));
#26565=CARTESIAN_POINT('Ctrl Pts',(0.961751173064136,-1.15426033407159,
-2.44492489192123));
#26566=CARTESIAN_POINT('Ctrl Pts',(0.883016083173381,-1.21528568040111,
-2.45007785607501));
#26567=CARTESIAN_POINT('Ctrl Pts',(0.699907663242089,-1.33073761999768,
-2.46133910588146));
#26568=CARTESIAN_POINT('Ctrl Pts',(0.593394360759729,-1.38193694102506,
-2.46745797747925));
#26569=CARTESIAN_POINT('Ctrl Pts',(0.356452332247631,-1.46302840729839,
-2.48088037938892));
#26570=CARTESIAN_POINT('Ctrl Pts',(0.226267156171132,-1.48861703792701,
-2.48817998771775));
#26571=CARTESIAN_POINT('Ctrl Pts',(-0.00575573259439318,-1.5024942239878,
-2.50052727259265));
#26572=CARTESIAN_POINT('Ctrl Pts',(-0.105522727995198,-1.49854594605227,
-2.50570057131398));
#26573=CARTESIAN_POINT('Ctrl Pts',(-0.323231911345657,-1.46862568093801,
-2.51713232860667));
#26574=CARTESIAN_POINT('Ctrl Pts',(-0.440651133511134,-1.43814338966285,
-2.52339821195141));
#26575=CARTESIAN_POINT('Ctrl Pts',(-0.691202779825589,-1.33949753157959,
-2.53779882845232));
#26576=CARTESIAN_POINT('Ctrl Pts',(-0.819432220536387,-1.26490268988018,
-2.54594988333623));
#26577=CARTESIAN_POINT('Ctrl Pts',(-1.01263927792284,-1.10985318182195,
-2.55905699989568));
#26578=CARTESIAN_POINT('Ctrl Pts',(-1.08376671442087,-1.0402156578075,-2.56420386152162));
#26579=CARTESIAN_POINT('Ctrl Pts',(-1.22248539198468,-0.875270661351363,
-2.57541672165905));
#26580=CARTESIAN_POINT('Ctrl Pts',(-1.28731113077471,-0.777524084483589,
-2.58149402763003));
#26581=CARTESIAN_POINT('Ctrl Pts',(-1.39385162402236,-0.566766273385554,
-2.59415987802189));
#26582=CARTESIAN_POINT('Ctrl Pts',(-1.43435322287458,-0.454479793904059,
-2.60073445227219));
#26583=CARTESIAN_POINT('Ctrl Pts',(-1.5015812723815,-0.160350362470448,
-2.61683902084733));
#26584=CARTESIAN_POINT('Ctrl Pts',(-1.50960418346396,0.0246008456484675,
-2.62616861592989));
#26585=CARTESIAN_POINT('Ctrl Pts',(-1.45976216021801,0.392156499871173,
-2.64565249615838));
#26586=CARTESIAN_POINT('Ctrl Pts',(-1.399761565596,0.571423312151105,-2.65599198974553));
#26587=CARTESIAN_POINT('Ctrl Pts',(-1.23961818549049,0.853752427289747,
-2.67322630593744));
#26588=CARTESIAN_POINT('Ctrl Pts',(-1.15716102202243,0.962143722011475,
-2.68020040010219));
#26589=CARTESIAN_POINT('Ctrl Pts',(-0.992056672740698,1.12835719182904,
-2.6924177652927));
#26590=CARTESIAN_POINT('Ctrl Pts',(-0.915130850074121,1.19202945755895,
-2.69763968365057));
#26591=CARTESIAN_POINT('Ctrl Pts',(-0.75101558780099,1.30203114848037,-2.70828226418718));
#26592=CARTESIAN_POINT('Ctrl Pts',(-0.664441333703433,1.34825382201765,
-2.71368412404045));
#26593=CARTESIAN_POINT('Ctrl Pts',(-0.46986663112808,1.42827884858882,-2.72497345546366));
#26594=CARTESIAN_POINT('Ctrl Pts',(-0.361429859064508,1.45911306464794,
-2.73082613074596));
#26595=CARTESIAN_POINT('Ctrl Pts',(-0.0868762359938478,1.50558560899306,
-2.74531699283014));
#26596=CARTESIAN_POINT('Ctrl Pts',(0.108524317627118,1.51122808336332,-2.75529891943664));
#26597=CARTESIAN_POINT('Ctrl Pts',(0.523722674688482,1.42104336270279,-2.77848372599165));
#26598=CARTESIAN_POINT('Ctrl Pts',(0.694234730116656,1.33806699529441,-2.78820584741986));
#26599=CARTESIAN_POINT('Ctrl Pts',(0.910861496243455,1.19466783524342,-2.80172096811971));
#26600=CARTESIAN_POINT('Ctrl Pts',(0.988671361944147,1.13146867146216,-2.80691876599564));
#26601=CARTESIAN_POINT('Ctrl Pts',(1.15071022630635,0.970526548957071,-2.81906886004611));
#26602=CARTESIAN_POINT('Ctrl Pts',(1.22919775430357,0.869129945757312,-2.8261266012726));
#26603=CARTESIAN_POINT('Ctrl Pts',(1.35102651289315,0.660088788782457,-2.83909822282311));
#26604=CARTESIAN_POINT('Ctrl Pts',(1.39685081727246,0.555601837988471,-2.84501522777272));
#26605=CARTESIAN_POINT('Ctrl Pts',(1.46023242591464,0.352631180147119,-2.85607893598742));
#26606=CARTESIAN_POINT('Ctrl Pts',(1.48061440505275,0.254942345668339,-2.86123656160737));
#26607=CARTESIAN_POINT('Ctrl Pts',(1.5071026689533,0.00828580751352354,
-2.87435255893675));
#26608=CARTESIAN_POINT('Ctrl Pts',(1.50081675130931,-0.140074127300878,
-2.88250645615547));
#26609=CARTESIAN_POINT('Ctrl Pts',(1.44962171173141,-0.400100283558441,
-2.89669155693413));
#26610=CARTESIAN_POINT('Ctrl Pts',(1.41383856372191,-0.511332352467065,
-2.90273927950043));
#26611=CARTESIAN_POINT('Ctrl Pts',(1.32508034510813,-0.707735304781241,
-2.91395129249664));
#26612=CARTESIAN_POINT('Ctrl Pts',(1.275257993154,-0.794428647626848,-2.91912511463628));
#26613=CARTESIAN_POINT('Ctrl Pts',(1.13603749864269,-0.989120951294424,
-2.93180966008441));
#26614=CARTESIAN_POINT('Ctrl Pts',(1.03978372917173,-1.09007739184633,-2.93947685530409));
#26615=CARTESIAN_POINT('Ctrl Pts',(0.83999292081546,-1.24722356599987,-2.9530967536497));
#26616=CARTESIAN_POINT('Ctrl Pts',(0.742007099482862,-1.30747183339931,
-2.95905803429899));
#26617=CARTESIAN_POINT('Ctrl Pts',(0.548714342580016,-1.39841818028193,
-2.97017198315474));
#26618=CARTESIAN_POINT('Ctrl Pts',(0.454659915573889,-1.43197845453193,
-2.97533518699447));
#26619=CARTESIAN_POINT('Ctrl Pts',(0.216974120279951,-1.49111903235992,
-2.98829538417047));
#26620=CARTESIAN_POINT('Ctrl Pts',(0.0724161569396505,-1.50527557455147,
-2.99627396486514));
#26621=CARTESIAN_POINT('Ctrl Pts',(-0.188277504892063,-1.49194501788374,
-3.01025172537403));
#26622=CARTESIAN_POINT('Ctrl Pts',(-0.30276292806724,-1.47261448509982,
-3.01626424532904));
#26623=CARTESIAN_POINT('Ctrl Pts',(-0.509166190941301,-1.41331142809819,
-3.02743639057836));
#26624=CARTESIAN_POINT('Ctrl Pts',(-0.602092049119227,-1.37653010346475,
-3.03260599265011));
#26625=CARTESIAN_POINT('Ctrl Pts',(-0.816798907961732,-1.26585681258326,
-3.04539924148289));
#26626=CARTESIAN_POINT('Ctrl Pts',(-0.932266966021383,-1.18361839848064,
-3.05318933375495));
#26627=CARTESIAN_POINT('Ctrl Pts',(-1.1176717611952,-1.00598881418804,-3.06694380600407));
#26628=CARTESIAN_POINT('Ctrl Pts',(-1.1911992232032,-0.917143963823157,
-3.07291881283867));
#26629=CARTESIAN_POINT('Ctrl Pts',(-1.30836409219534,-0.738141596012679,
-3.08404861925295));
#26630=CARTESIAN_POINT('Ctrl Pts',(-1.35471182572544,-0.649655711805248,
-3.08921376341646));
#26631=CARTESIAN_POINT('Ctrl Pts',(-1.44584034292854,-0.42384252583581,
-3.10210234042886));
#26632=CARTESIAN_POINT('Ctrl Pts',(-1.47984174077635,-0.284133317596366,
-3.11000165399304));
#26633=CARTESIAN_POINT('Ctrl Pts',(-1.50356071468369,-0.0257340761398541,
-3.12390253859812));
#26634=CARTESIAN_POINT('Ctrl Pts',(-1.500706949238,0.0902601036655123,-3.12991376788401));
#26635=CARTESIAN_POINT('Ctrl Pts',(-1.4713835756108,0.302890057303145,-3.14108242947861));
#26636=CARTESIAN_POINT('Ctrl Pts',(-1.44820663630739,0.400068083833837,
-3.14625016146593));
#26637=CARTESIAN_POINT('Ctrl Pts',(-1.36846871474809,0.630511787657366,
-3.15916112595278));
#26638=CARTESIAN_POINT('Ctrl Pts',(-1.30213290035678,0.758432227761769,
-3.16707761328715));
#26639=CARTESIAN_POINT('Ctrl Pts',(-1.15014464600899,0.968689653569568,
-3.18095602028395));
#26640=CARTESIAN_POINT('Ctrl Pts',(-1.07203283432336,1.05396027144467,-3.18693871001679));
#26641=CARTESIAN_POINT('Ctrl Pts',(-0.872606659870649,1.22786655368525,
-3.2006960890497));
#26642=CARTESIAN_POINT('Ctrl Pts',(-0.726903650726398,1.32597814557258,
-3.20968126963886));
#26643=CARTESIAN_POINT('Ctrl Pts',(-0.462343408398025,1.42967442692924,
-3.22519006837585));
#26644=CARTESIAN_POINT('Ctrl Pts',(-0.375674252658106,1.45470533198749,
-3.23009449424634));
#26645=CARTESIAN_POINT('Ctrl Pts',(-0.192359458101488,1.48996300799368,
-3.24002156504885));
#26646=CARTESIAN_POINT('Ctrl Pts',(-0.0961554125704673,1.49902501105836,
-3.24503897916825));
#26647=CARTESIAN_POINT('Ctrl Pts',(2.06854460825176E-5,1.49901358627223,
-3.25004513644298));
#26648=CARTESIAN_POINT('',(-3.24550813896681E-10,1.11698717744401,-3.47113249718027));
#26649=CARTESIAN_POINT('',(0.,1.5,-3.25));
#26650=CARTESIAN_POINT('Ctrl Pts',(-2.52570946139784E-6,-1.11628565496219,
-1.7211141243504));
#26651=CARTESIAN_POINT('Ctrl Pts',(-0.0945479806554323,-1.1164597063096,
-1.72785017591353));
#26652=CARTESIAN_POINT('Ctrl Pts',(-0.189124550454961,-1.10484912539831,
-1.73459224965733));
#26653=CARTESIAN_POINT('Ctrl Pts',(-0.372801771216836,-1.05728993252109,
-1.74813469212525));
#26654=CARTESIAN_POINT('Ctrl Pts',(-0.46120369907326,-1.02120420332243,
-1.75489047466375));
#26655=CARTESIAN_POINT('Ctrl Pts',(-0.668471432388855,-0.904915646636004,
-1.77182073957925));
#26656=CARTESIAN_POINT('Ctrl Pts',(-0.780383055419264,-0.811029500761429,
-1.78202995426488));
#26657=CARTESIAN_POINT('Ctrl Pts',(-0.977352549963127,-0.567498199932436,
-1.80436776308206));
#26658=CARTESIAN_POINT('Ctrl Pts',(-1.03703915589555,-0.431145768277802,
-1.8147587800084));
#26659=CARTESIAN_POINT('Ctrl Pts',(-1.11066616674449,-0.178042375581388,
-1.83352929238689));
#26660=CARTESIAN_POINT('Ctrl Pts',(-1.1250370353998,-0.0352369170927978,
-1.84357133882956));
#26661=CARTESIAN_POINT('Ctrl Pts',(-1.09418460733438,0.296790717289756,
-1.86736190012804));
#26662=CARTESIAN_POINT('Ctrl Pts',(-1.02997735713434,0.440477084842055,
-1.87828381624767));
#26663=CARTESIAN_POINT('Ctrl Pts',(-0.925588908242799,0.636392952388536,
-1.89408990478641));
#26664=CARTESIAN_POINT('Ctrl Pts',(-0.840538191683134,0.751460714065274,
-1.90410198836101));
#26665=CARTESIAN_POINT('Ctrl Pts',(-0.61118224779972,0.946513834085747,
-1.92558474266587));
#26666=CARTESIAN_POINT('Ctrl Pts',(-0.4782345297511,1.0191711099922,-1.93616577485579));
#26667=CARTESIAN_POINT('Ctrl Pts',(-0.222597234321223,1.1004636264182,-1.955267721173));
#26668=CARTESIAN_POINT('Ctrl Pts',(-0.0794663775051731,1.12675755955542,
-1.96543571983759));
#26669=CARTESIAN_POINT('Ctrl Pts',(0.232981315456785,1.10176800386664,-1.98779253835339));
#26670=CARTESIAN_POINT('Ctrl Pts',(0.377700605109035,1.06037143957914,-1.99830194335543));
#26671=CARTESIAN_POINT('Ctrl Pts',(0.60485272432455,0.944731736167608,-2.01645937858707));
#26672=CARTESIAN_POINT('Ctrl Pts',(0.731331226988472,0.863974006299934,
-2.02692136770941));
#26673=CARTESIAN_POINT('Ctrl Pts',(0.943397907937875,0.61393454762197,-2.05029160325254));
#26674=CARTESIAN_POINT('Ctrl Pts',(1.01607631574408,0.484189787750154,-2.06067712497169));
#26675=CARTESIAN_POINT('Ctrl Pts',(1.11857306467123,0.173002860562897,-2.08402934320733));
#26676=CARTESIAN_POINT('Ctrl Pts',(1.1216526627367,0.0230529286472913,-2.09448736045733));
#26677=CARTESIAN_POINT('Ctrl Pts',(1.10179845703877,-0.228016486144775,
-2.11242927917354));
#26678=CARTESIAN_POINT('Ctrl Pts',(1.06324590215936,-0.369253565391399,
-2.12266080687385));
#26679=CARTESIAN_POINT('Ctrl Pts',(0.924464855646186,-0.649976757040046,
-2.14499359014349));
#26680=CARTESIAN_POINT('Ctrl Pts',(0.825915661788604,-0.761161572818591,
-2.15536755467241));
#26681=CARTESIAN_POINT('Ctrl Pts',(0.626214316349842,-0.934430304671211,
-2.17419538133658));
#26682=CARTESIAN_POINT('Ctrl Pts',(0.502214996937528,-1.0073238571117,-2.18425796124846));
#26683=CARTESIAN_POINT('Ctrl Pts',(0.19120199753371,-1.11682300306852,-2.20778190972181));
#26684=CARTESIAN_POINT('Ctrl Pts',(0.0349012702549543,-1.12007370080308,
-2.21864513166231));
#26685=CARTESIAN_POINT('Ctrl Pts',(-0.203851405860762,-1.10611718857029,
-2.23567366866181));
#26686=CARTESIAN_POINT('Ctrl Pts',(-0.341786112597053,-1.07261170247851,
-2.245614088678));
#26687=CARTESIAN_POINT('Ctrl Pts',(-0.603413551668547,-0.95156305246283,
-2.26618313304261));
#26688=CARTESIAN_POINT('Ctrl Pts',(-0.725113385898963,-0.861211673415812,
-2.27676949290965));
#26689=CARTESIAN_POINT('Ctrl Pts',(-0.905273423514502,-0.663857977873306,
-2.29579742516296));
#26690=CARTESIAN_POINT('Ctrl Pts',(-0.989304020610915,-0.545163021076572,
-2.30595751403342));
#26691=CARTESIAN_POINT('Ctrl Pts',(-1.09791444748827,-0.250846118613153,
-2.32833525890648));
#26692=CARTESIAN_POINT('Ctrl Pts',(-1.12102369397598,-0.101931202388067,
-2.33885689635648));
#26693=CARTESIAN_POINT('Ctrl Pts',(-1.11127472608703,0.152382998726041,
-2.35698527230642));
#26694=CARTESIAN_POINT('Ctrl Pts',(-1.09120934524511,0.300938815206558,
-2.36743533545796));
#26695=CARTESIAN_POINT('Ctrl Pts',(-0.953355092950169,0.598483057720678,
-2.39081240762303));
#26696=CARTESIAN_POINT('Ctrl Pts',(-0.865889506205107,0.719096632405901,
-2.40121651825254));
#26697=CARTESIAN_POINT('Ctrl Pts',(-0.630908211369321,0.938430669099282,
-2.42412556939149));
#26698=CARTESIAN_POINT('Ctrl Pts',(-0.499473987912807,1.00559671816687,
-2.43443093822623));
#26699=CARTESIAN_POINT('Ctrl Pts',(-0.254954649474644,1.09592824110065,
-2.45300231361181));
#26700=CARTESIAN_POINT('Ctrl Pts',(-0.110233508147538,1.12012616746575,
-2.46325541986775));
#26701=CARTESIAN_POINT('Ctrl Pts',(0.202625788977277,1.11169037854405,-2.48557375090056));
#26702=CARTESIAN_POINT('Ctrl Pts',(0.344594062565005,1.06910154094397,-2.49592507043897));
#26703=CARTESIAN_POINT('Ctrl Pts',(0.586363065095529,0.95997491663841,-2.5148152172114));
#26704=CARTESIAN_POINT('Ctrl Pts',(0.704733656287602,0.877644037487904,
-2.52490073023948));
#26705=CARTESIAN_POINT('Ctrl Pts',(0.924445762809004,0.651144082671878,
-2.54741286795022));
#26706=CARTESIAN_POINT('Ctrl Pts',(0.995878303027182,0.517818669122211,
-2.55795712525469));
#26707=CARTESIAN_POINT('Ctrl Pts',(1.08982166380632,0.277939862987314,-2.57630001885425));
#26708=CARTESIAN_POINT('Ctrl Pts',(1.1169872981078,0.139044412854724,-2.58621126978535));
#26709=CARTESIAN_POINT('Ctrl Pts',(1.1169872981078,-0.139044412854727,-2.60605370329665));
#26710=CARTESIAN_POINT('Ctrl Pts',(1.08982166380632,-0.277939862987316,
-2.61596495422619));
#26711=CARTESIAN_POINT('Ctrl Pts',(0.99587830302718,-0.517818669122218,
-2.63430784782586));
#26712=CARTESIAN_POINT('Ctrl Pts',(0.924445762808999,-0.651144082671885,
-2.64485210513048));
#26713=CARTESIAN_POINT('Ctrl Pts',(0.704733656287598,-0.877644037487907,
-2.66736424284125));
#26714=CARTESIAN_POINT('Ctrl Pts',(0.586363065095524,-0.959974916638413,
-2.67744975586925));
#26715=CARTESIAN_POINT('Ctrl Pts',(0.344594062564994,-1.06910154094398,
-2.69633990264163));
#26716=CARTESIAN_POINT('Ctrl Pts',(0.202625788977266,-1.11169037854405,
-2.70669122217995));
#26717=CARTESIAN_POINT('Ctrl Pts',(-0.110233508147553,-1.12012616746575,
-2.72900955321284));
#26718=CARTESIAN_POINT('Ctrl Pts',(-0.254954649474663,-1.09592824110064,
-2.73926265946891));
#26719=CARTESIAN_POINT('Ctrl Pts',(-0.499473987912819,-1.00559671816686,
-2.75783403485462));
#26720=CARTESIAN_POINT('Ctrl Pts',(-0.63090821136934,-0.938430669099273,
-2.76813940368944));
#26721=CARTESIAN_POINT('Ctrl Pts',(-0.865889506205136,-0.719096632405868,
-2.79104845482854));
#26722=CARTESIAN_POINT('Ctrl Pts',(-0.953355092950196,-0.598483057720636,
-2.80145256545815));
#26723=CARTESIAN_POINT('Ctrl Pts',(-1.09120934524513,-0.300938815206489,
-2.82482963762336));
#26724=CARTESIAN_POINT('Ctrl Pts',(-1.11127472608704,-0.152382998725963,
-2.83527970077493));
#26725=CARTESIAN_POINT('Ctrl Pts',(-1.12102369397598,0.101931202388125,
-2.85340807672478));
#26726=CARTESIAN_POINT('Ctrl Pts',(-1.09791444748826,0.250846118613208,
-2.86392971417461));
#26727=CARTESIAN_POINT('Ctrl Pts',(-0.989304020610891,0.545163021076614,
-2.88630745904754));
#26728=CARTESIAN_POINT('Ctrl Pts',(-0.905273423514476,0.663857977873339,
-2.89646754791798));
#26729=CARTESIAN_POINT('Ctrl Pts',(-0.725113385898938,0.861211673415833,
-2.91549548017135));
#26730=CARTESIAN_POINT('Ctrl Pts',(-0.603413551668517,0.951563052462851,
-2.92608184003854));
#26731=CARTESIAN_POINT('Ctrl Pts',(-0.341786112597021,1.07261170247852,
-2.94665088440312));
#26732=CARTESIAN_POINT('Ctrl Pts',(-0.203851405860732,1.1061171885703,-2.95659130441917));
#26733=CARTESIAN_POINT('Ctrl Pts',(0.0349012702549755,1.12007370080307,
-2.97361984141848));
#26734=CARTESIAN_POINT('Ctrl Pts',(0.191201997533727,1.11682300306852,-2.98448306335867));
#26735=CARTESIAN_POINT('Ctrl Pts',(0.502214996937547,1.00732385711169,-3.00800701183202));
#26736=CARTESIAN_POINT('Ctrl Pts',(0.626214316349863,0.934430304671194,
-3.01806959174406));
#26737=CARTESIAN_POINT('Ctrl Pts',(0.825915661788622,0.761161572818569,
-3.03689741840843));
#26738=CARTESIAN_POINT('Ctrl Pts',(0.924464855646206,0.649976757040018,
-3.04727138293758));
#26739=CARTESIAN_POINT('Ctrl Pts',(1.06324590215938,0.369253565391358,-3.06960416620731));
#26740=CARTESIAN_POINT('Ctrl Pts',(1.10179845703878,0.22801648614473,-3.07983569390757));
#26741=CARTESIAN_POINT('Ctrl Pts',(1.12165266273671,-0.023052928647412,
-3.09777761262373));
#26742=CARTESIAN_POINT('Ctrl Pts',(1.11857306467121,-0.173002860562994,
-3.10823562987364));
#26743=CARTESIAN_POINT('Ctrl Pts',(1.01607631574406,-0.484189787750188,
-3.13158784810919));
#26744=CARTESIAN_POINT('Ctrl Pts',(0.943397907937855,-0.613934547622001,
-3.1419733698283));
#26745=CARTESIAN_POINT('Ctrl Pts',(0.731331226988425,-0.863974006299982,
-3.16534360537137));
#26746=CARTESIAN_POINT('Ctrl Pts',(0.604852724324483,-0.944731736167644,
-3.17580559449369));
#26747=CARTESIAN_POINT('Ctrl Pts',(0.37770060510901,-1.06037143957915,-3.1939630297253));
#26748=CARTESIAN_POINT('Ctrl Pts',(0.232981315456759,-1.10176800386665,
-3.20447243472734));
#26749=CARTESIAN_POINT('Ctrl Pts',(-0.0794663775051969,-1.12675755955542,
-3.22682925324312));
#26750=CARTESIAN_POINT('Ctrl Pts',(-0.222597234321245,-1.1004636264182,
-3.23699725190771));
#26751=CARTESIAN_POINT('Ctrl Pts',(-0.47823452975112,-1.0191711099922,-3.25609919822493));
#26752=CARTESIAN_POINT('Ctrl Pts',(-0.611182247799739,-0.946513834085735,
-3.26668023041484));
#26753=CARTESIAN_POINT('Ctrl Pts',(-0.840538191683138,-0.751460714065267,
-3.28816298471981));
#26754=CARTESIAN_POINT('Ctrl Pts',(-0.925588908242806,-0.636392952388529,
-3.29817506829455));
#26755=CARTESIAN_POINT('Ctrl Pts',(-1.02997735713432,-0.440477084842082,
-3.31398115683343));
#26756=CARTESIAN_POINT('Ctrl Pts',(-1.09418460733438,-0.296790717289784,
-3.32490307295328));
#26757=CARTESIAN_POINT('Ctrl Pts',(-1.1250370353998,0.0352369170927936,
-3.34869363425172));
#26758=CARTESIAN_POINT('Ctrl Pts',(-1.11066616674449,0.178042375581363,
-3.35873568069418));
#26759=CARTESIAN_POINT('Ctrl Pts',(-1.03703915589554,0.431145768277777,
-3.37750619307247));
#26760=CARTESIAN_POINT('Ctrl Pts',(-0.977352549963106,0.567498199932408,
-3.38789720999858));
#26761=CARTESIAN_POINT('Ctrl Pts',(-0.780383055419209,0.811029500761431,
-3.41023501881582));
#26762=CARTESIAN_POINT('Ctrl Pts',(-0.668471432388769,0.904915646636028,
-3.42044423350163));
#26763=CARTESIAN_POINT('Ctrl Pts',(-0.461203748610638,1.02120417552921,
-3.43737449437096));
#26764=CARTESIAN_POINT('Ctrl Pts',(-0.372801878429867,1.05728988862637,
-3.4441302727615));
#26765=CARTESIAN_POINT('Ctrl Pts',(-0.18912446213411,1.10484916429063,-3.45767273022351));
#26766=CARTESIAN_POINT('Ctrl Pts',(-0.0945476136912702,1.11645975869105,
-3.46441482333082));
#26767=CARTESIAN_POINT('Ctrl Pts',(-1.88721575744071E-6,1.11628565378659,
-3.47115089422152));
#26768=CARTESIAN_POINT('Ctrl Pts',(0.4755900604755,-1.010680324589,-1.670126599063));
#26769=CARTESIAN_POINT('Ctrl Pts',(0.2348081643589,-1.123983684464,-1.689084932396));
#26770=CARTESIAN_POINT('Ctrl Pts',(-0.329952574922,-1.170452920957,-1.727001599063));
#26771=CARTESIAN_POINT('Ctrl Pts',(-1.016551442463,-0.6677408946504,-1.783876599063));
#26772=CARTESIAN_POINT('Ctrl Pts',(-1.205358893105,0.1619074151071,-1.840751599063));
#26773=CARTESIAN_POINT('Ctrl Pts',(-0.8042879589087,0.9122802996697,-1.897626599063));
#26774=CARTESIAN_POINT('Ctrl Pts',(-0.009550993186477,1.216158607898,-1.954501599063));
#26775=CARTESIAN_POINT('Ctrl Pts',(0.7898556864549,0.9248023542725,-2.011376599063));
#26776=CARTESIAN_POINT('Ctrl Pts',(1.202679571961,0.180814804896,-2.068251599063));
#26777=CARTESIAN_POINT('Ctrl Pts',(1.026867975908,-0.6516702524068,-2.125126599063));
#26778=CARTESIAN_POINT('Ctrl Pts',(0.348469933747,-1.165204139133,-2.182001599063));
#26779=CARTESIAN_POINT('Ctrl Pts',(-0.5004819949382,-1.108444747226,-2.238876599063));
#26780=CARTESIAN_POINT('Ctrl Pts',(-1.104479823299,-0.5091721726955,-2.295751599063));
#26781=CARTESIAN_POINT('Ctrl Pts',(-1.167905052019,0.3393077836576,-2.352626599063));
#26782=CARTESIAN_POINT('Ctrl Pts',(-0.6597150647482,1.02171816845,-2.409501599063));
#26783=CARTESIAN_POINT('Ctrl Pts',(0.1713634724997,1.204062516105,-2.466376599063));
#26784=CARTESIAN_POINT('Ctrl Pts',(0.9185704929214,0.7970948701029,-2.523251599063));
#26785=CARTESIAN_POINT('Ctrl Pts',(1.216195700701,0.,-2.580126599063));
#26786=CARTESIAN_POINT('Ctrl Pts',(0.9185704929214,-0.7970948701029,-2.637001599063));
#26787=CARTESIAN_POINT('Ctrl Pts',(0.1713634724997,-1.204062516105,-2.693876599063));
#26788=CARTESIAN_POINT('Ctrl Pts',(-0.6597150647482,-1.02171816845,-2.750751599063));
#26789=CARTESIAN_POINT('Ctrl Pts',(-1.167905052019,-0.3393077836576,-2.807626599063));
#26790=CARTESIAN_POINT('Ctrl Pts',(-1.104479823299,0.5091721726955,-2.864501599063));
#26791=CARTESIAN_POINT('Ctrl Pts',(-0.5004819949382,1.108444747226,-2.921376599063));
#26792=CARTESIAN_POINT('Ctrl Pts',(0.348469933747,1.165204139133,-2.978251599063));
#26793=CARTESIAN_POINT('Ctrl Pts',(1.026867975908,0.6516702524068,-3.035126599063));
#26794=CARTESIAN_POINT('Ctrl Pts',(1.202679571961,-0.180814804896,-3.092001599063));
#26795=CARTESIAN_POINT('Ctrl Pts',(0.7898556864549,-0.9248023542725,-3.148876599063));
#26796=CARTESIAN_POINT('Ctrl Pts',(-0.009550993186476,-1.216158607898,-3.205751599063));
#26797=CARTESIAN_POINT('Ctrl Pts',(-0.8042879589087,-0.9122802996697,-3.262626599063));
#26798=CARTESIAN_POINT('Ctrl Pts',(-1.205358893105,-0.1619074151071,-3.319501599063));
#26799=CARTESIAN_POINT('Ctrl Pts',(-1.016551442463,0.6677408946503,-3.376376599063));
#26800=CARTESIAN_POINT('Ctrl Pts',(-0.329952574922,1.170452920957,-3.433251599063));
#26801=CARTESIAN_POINT('Ctrl Pts',(0.2348081643589,1.123983684464,-3.47116826573));
#26802=CARTESIAN_POINT('Ctrl Pts',(0.4755900604755,1.010680324589,-3.490126599063));
#26803=CARTESIAN_POINT('Ctrl Pts',(0.4755900604755,-1.010680324589,-1.700042199688));
#26804=CARTESIAN_POINT('Ctrl Pts',(0.2348081643589,-1.123983684464,-1.719000533021));
#26805=CARTESIAN_POINT('Ctrl Pts',(-0.329952574922,-1.170452920957,-1.756917199688));
#26806=CARTESIAN_POINT('Ctrl Pts',(-1.016551442463,-0.6677408946504,-1.813792199688));
#26807=CARTESIAN_POINT('Ctrl Pts',(-1.205358893105,0.1619074151071,-1.870667199688));
#26808=CARTESIAN_POINT('Ctrl Pts',(-0.8042879589087,0.9122802996697,-1.927542199688));
#26809=CARTESIAN_POINT('Ctrl Pts',(-0.009550993186477,1.216158607898,-1.984417199688));
#26810=CARTESIAN_POINT('Ctrl Pts',(0.7898556864549,0.9248023542725,-2.041292199688));
#26811=CARTESIAN_POINT('Ctrl Pts',(1.202679571961,0.180814804896,-2.098167199688));
#26812=CARTESIAN_POINT('Ctrl Pts',(1.026867975908,-0.6516702524068,-2.155042199688));
#26813=CARTESIAN_POINT('Ctrl Pts',(0.348469933747,-1.165204139133,-2.211917199688));
#26814=CARTESIAN_POINT('Ctrl Pts',(-0.5004819949382,-1.108444747226,-2.268792199688));
#26815=CARTESIAN_POINT('Ctrl Pts',(-1.104479823299,-0.5091721726955,-2.325667199688));
#26816=CARTESIAN_POINT('Ctrl Pts',(-1.167905052019,0.3393077836576,-2.382542199688));
#26817=CARTESIAN_POINT('Ctrl Pts',(-0.6597150647482,1.02171816845,-2.439417199688));
#26818=CARTESIAN_POINT('Ctrl Pts',(0.1713634724997,1.204062516105,-2.496292199688));
#26819=CARTESIAN_POINT('Ctrl Pts',(0.9185704929214,0.7970948701029,-2.553167199688));
#26820=CARTESIAN_POINT('Ctrl Pts',(1.216195700701,0.,-2.610042199688));
#26821=CARTESIAN_POINT('Ctrl Pts',(0.9185704929214,-0.7970948701029,-2.666917199688));
#26822=CARTESIAN_POINT('Ctrl Pts',(0.1713634724997,-1.204062516105,-2.723792199688));
#26823=CARTESIAN_POINT('Ctrl Pts',(-0.6597150647482,-1.02171816845,-2.780667199688));
#26824=CARTESIAN_POINT('Ctrl Pts',(-1.167905052019,-0.3393077836576,-2.837542199688));
#26825=CARTESIAN_POINT('Ctrl Pts',(-1.104479823299,0.5091721726955,-2.894417199688));
#26826=CARTESIAN_POINT('Ctrl Pts',(-0.5004819949382,1.108444747226,-2.951292199688));
#26827=CARTESIAN_POINT('Ctrl Pts',(0.348469933747,1.165204139133,-3.008167199688));
#26828=CARTESIAN_POINT('Ctrl Pts',(1.026867975908,0.6516702524068,-3.065042199688));
#26829=CARTESIAN_POINT('Ctrl Pts',(1.202679571961,-0.180814804896,-3.121917199688));
#26830=CARTESIAN_POINT('Ctrl Pts',(0.7898556864549,-0.9248023542725,-3.178792199688));
#26831=CARTESIAN_POINT('Ctrl Pts',(-0.009550993186476,-1.216158607898,-3.235667199688));
#26832=CARTESIAN_POINT('Ctrl Pts',(-0.8042879589087,-0.9122802996697,-3.292542199688));
#26833=CARTESIAN_POINT('Ctrl Pts',(-1.205358893105,-0.1619074151071,-3.349417199688));
#26834=CARTESIAN_POINT('Ctrl Pts',(-1.016551442463,0.6677408946503,-3.406292199688));
#26835=CARTESIAN_POINT('Ctrl Pts',(-0.329952574922,1.170452920957,-3.463167199688));
#26836=CARTESIAN_POINT('Ctrl Pts',(0.2348081643589,1.123983684464,-3.501083866354));
#26837=CARTESIAN_POINT('Ctrl Pts',(0.4755900604755,1.010680324589,-3.520042199688));
#26838=CARTESIAN_POINT('Ctrl Pts',(0.4755900604755,-1.010680324589,-1.729957800312));
#26839=CARTESIAN_POINT('Ctrl Pts',(0.2348081643589,-1.123983684464,-1.748916133646));
#26840=CARTESIAN_POINT('Ctrl Pts',(-0.329952574922,-1.170452920957,-1.786832800312));
#26841=CARTESIAN_POINT('Ctrl Pts',(-1.016551442463,-0.6677408946504,-1.843707800312));
#26842=CARTESIAN_POINT('Ctrl Pts',(-1.205358893105,0.1619074151071,-1.900582800312));
#26843=CARTESIAN_POINT('Ctrl Pts',(-0.8042879589087,0.9122802996697,-1.957457800312));
#26844=CARTESIAN_POINT('Ctrl Pts',(-0.009550993186478,1.216158607898,-2.014332800312));
#26845=CARTESIAN_POINT('Ctrl Pts',(0.7898556864549,0.9248023542725,-2.071207800312));
#26846=CARTESIAN_POINT('Ctrl Pts',(1.202679571961,0.180814804896,-2.128082800312));
#26847=CARTESIAN_POINT('Ctrl Pts',(1.026867975908,-0.6516702524068,-2.184957800312));
#26848=CARTESIAN_POINT('Ctrl Pts',(0.348469933747,-1.165204139133,-2.241832800312));
#26849=CARTESIAN_POINT('Ctrl Pts',(-0.5004819949382,-1.108444747226,-2.298707800312));
#26850=CARTESIAN_POINT('Ctrl Pts',(-1.104479823299,-0.5091721726955,-2.355582800312));
#26851=CARTESIAN_POINT('Ctrl Pts',(-1.167905052019,0.3393077836576,-2.412457800312));
#26852=CARTESIAN_POINT('Ctrl Pts',(-0.6597150647482,1.02171816845,-2.469332800312));
#26853=CARTESIAN_POINT('Ctrl Pts',(0.1713634724997,1.204062516105,-2.526207800312));
#26854=CARTESIAN_POINT('Ctrl Pts',(0.9185704929214,0.7970948701029,-2.583082800312));
#26855=CARTESIAN_POINT('Ctrl Pts',(1.216195700701,0.,-2.639957800312));
#26856=CARTESIAN_POINT('Ctrl Pts',(0.9185704929214,-0.7970948701029,-2.696832800312));
#26857=CARTESIAN_POINT('Ctrl Pts',(0.1713634724997,-1.204062516105,-2.753707800312));
#26858=CARTESIAN_POINT('Ctrl Pts',(-0.6597150647482,-1.02171816845,-2.810582800312));
#26859=CARTESIAN_POINT('Ctrl Pts',(-1.167905052019,-0.3393077836576,-2.867457800312));
#26860=CARTESIAN_POINT('Ctrl Pts',(-1.104479823299,0.5091721726955,-2.924332800312));
#26861=CARTESIAN_POINT('Ctrl Pts',(-0.5004819949382,1.108444747226,-2.981207800312));
#26862=CARTESIAN_POINT('Ctrl Pts',(0.3484699337469,1.165204139133,-3.038082800312));
#26863=CARTESIAN_POINT('Ctrl Pts',(1.026867975908,0.6516702524068,-3.094957800312));
#26864=CARTESIAN_POINT('Ctrl Pts',(1.202679571961,-0.180814804896,-3.151832800312));
#26865=CARTESIAN_POINT('Ctrl Pts',(0.7898556864549,-0.9248023542725,-3.208707800312));
#26866=CARTESIAN_POINT('Ctrl Pts',(-0.009550993186476,-1.216158607898,-3.265582800312));
#26867=CARTESIAN_POINT('Ctrl Pts',(-0.8042879589087,-0.9122802996697,-3.322457800312));
#26868=CARTESIAN_POINT('Ctrl Pts',(-1.205358893105,-0.1619074151071,-3.379332800312));
#26869=CARTESIAN_POINT('Ctrl Pts',(-1.016551442463,0.6677408946504,-3.436207800312));
#26870=CARTESIAN_POINT('Ctrl Pts',(-0.329952574922,1.170452920957,-3.493082800312));
#26871=CARTESIAN_POINT('Ctrl Pts',(0.2348081643589,1.123983684464,-3.530999466979));
#26872=CARTESIAN_POINT('Ctrl Pts',(0.4755900604755,1.010680324589,-3.549957800312));
#26873=CARTESIAN_POINT('Ctrl Pts',(0.4755900604755,-1.010680324589,-1.759873400937));
#26874=CARTESIAN_POINT('Ctrl Pts',(0.2348081643589,-1.123983684464,-1.77883173427));
#26875=CARTESIAN_POINT('Ctrl Pts',(-0.329952574922,-1.170452920957,-1.816748400937));
#26876=CARTESIAN_POINT('Ctrl Pts',(-1.016551442463,-0.6677408946504,-1.873623400937));
#26877=CARTESIAN_POINT('Ctrl Pts',(-1.205358893105,0.1619074151071,-1.930498400937));
#26878=CARTESIAN_POINT('Ctrl Pts',(-0.8042879589087,0.9122802996697,-1.987373400937));
#26879=CARTESIAN_POINT('Ctrl Pts',(-0.009550993186478,1.216158607898,-2.044248400937));
#26880=CARTESIAN_POINT('Ctrl Pts',(0.7898556864549,0.9248023542725,-2.101123400937));
#26881=CARTESIAN_POINT('Ctrl Pts',(1.202679571961,0.180814804896,-2.157998400937));
#26882=CARTESIAN_POINT('Ctrl Pts',(1.026867975908,-0.6516702524068,-2.214873400937));
#26883=CARTESIAN_POINT('Ctrl Pts',(0.348469933747,-1.165204139133,-2.271748400937));
#26884=CARTESIAN_POINT('Ctrl Pts',(-0.5004819949382,-1.108444747226,-2.328623400937));
#26885=CARTESIAN_POINT('Ctrl Pts',(-1.104479823299,-0.5091721726955,-2.385498400937));
#26886=CARTESIAN_POINT('Ctrl Pts',(-1.167905052019,0.3393077836576,-2.442373400937));
#26887=CARTESIAN_POINT('Ctrl Pts',(-0.6597150647482,1.02171816845,-2.499248400937));
#26888=CARTESIAN_POINT('Ctrl Pts',(0.1713634724997,1.204062516105,-2.556123400937));
#26889=CARTESIAN_POINT('Ctrl Pts',(0.9185704929214,0.7970948701029,-2.612998400937));
#26890=CARTESIAN_POINT('Ctrl Pts',(1.216195700701,0.,-2.669873400937));
#26891=CARTESIAN_POINT('Ctrl Pts',(0.9185704929214,-0.7970948701029,-2.726748400937));
#26892=CARTESIAN_POINT('Ctrl Pts',(0.1713634724997,-1.204062516105,-2.783623400937));
#26893=CARTESIAN_POINT('Ctrl Pts',(-0.6597150647482,-1.02171816845,-2.840498400937));
#26894=CARTESIAN_POINT('Ctrl Pts',(-1.167905052019,-0.3393077836576,-2.897373400937));
#26895=CARTESIAN_POINT('Ctrl Pts',(-1.104479823299,0.5091721726955,-2.954248400937));
#26896=CARTESIAN_POINT('Ctrl Pts',(-0.5004819949382,1.108444747226,-3.011123400937));
#26897=CARTESIAN_POINT('Ctrl Pts',(0.3484699337469,1.165204139133,-3.067998400937));
#26898=CARTESIAN_POINT('Ctrl Pts',(1.026867975908,0.6516702524068,-3.124873400937));
#26899=CARTESIAN_POINT('Ctrl Pts',(1.202679571961,-0.180814804896,-3.181748400937));
#26900=CARTESIAN_POINT('Ctrl Pts',(0.7898556864549,-0.9248023542725,-3.238623400937));
#26901=CARTESIAN_POINT('Ctrl Pts',(-0.009550993186476,-1.216158607898,-3.295498400937));
#26902=CARTESIAN_POINT('Ctrl Pts',(-0.8042879589087,-0.9122802996697,-3.352373400937));
#26903=CARTESIAN_POINT('Ctrl Pts',(-1.205358893105,-0.1619074151071,-3.409248400937));
#26904=CARTESIAN_POINT('Ctrl Pts',(-1.016551442463,0.6677408946504,-3.466123400937));
#26905=CARTESIAN_POINT('Ctrl Pts',(-0.329952574922,1.170452920957,-3.522998400937));
#26906=CARTESIAN_POINT('Ctrl Pts',(0.2348081643589,1.123983684464,-3.560915067604));
#26907=CARTESIAN_POINT('Ctrl Pts',(0.4755900604755,1.010680324589,-3.579873400937));
#26908=CARTESIAN_POINT('',(-3.4898201487235E-10,1.11698717731251,-3.52886751164369));
#26909=CARTESIAN_POINT('',(0.,1.116987298108,-3.471132486541));
#26910=CARTESIAN_POINT('Ctrl Pts',(-1.8872157446454E-6,-1.11628565378659,
-1.77884910577848));
#26911=CARTESIAN_POINT('Ctrl Pts',(-0.0945476136912763,-1.11645975869106,
-1.78558517666919));
#26912=CARTESIAN_POINT('Ctrl Pts',(-0.189124462134139,-1.10484916429063,
-1.79232726977651));
#26913=CARTESIAN_POINT('Ctrl Pts',(-0.372801878429928,-1.05728988862637,
-1.80586972723853));
#26914=CARTESIAN_POINT('Ctrl Pts',(-0.461203748610714,-1.0212041755292,
-1.81262550562908));
#26915=CARTESIAN_POINT('Ctrl Pts',(-0.668471432388827,-0.904915646636025,
-1.82955576649842));
#26916=CARTESIAN_POINT('Ctrl Pts',(-0.780383055419241,-0.811029500761452,
-1.83976498118422));
#26917=CARTESIAN_POINT('Ctrl Pts',(-0.977352549963109,-0.567498199932465,
-1.86210279000144));
#26918=CARTESIAN_POINT('Ctrl Pts',(-1.03703915589554,-0.431145768277838,
-1.87249380692754));
#26919=CARTESIAN_POINT('Ctrl Pts',(-1.11066616674449,-0.178042375581421,
-1.89126431930581));
#26920=CARTESIAN_POINT('Ctrl Pts',(-1.1250370353998,-0.0352369170928321,
-1.90130636574828));
#26921=CARTESIAN_POINT('Ctrl Pts',(-1.09418460733438,0.296790717289773,
-1.92509692704671));
#26922=CARTESIAN_POINT('Ctrl Pts',(-1.02997735713432,0.440477084842074,
-1.93601884316657));
#26923=CARTESIAN_POINT('Ctrl Pts',(-0.925588908242807,0.636392952388529,
-1.95182493170545));
#26924=CARTESIAN_POINT('Ctrl Pts',(-0.840538191683139,0.751460714065266,
-1.96183701528019));
#26925=CARTESIAN_POINT('Ctrl Pts',(-0.61118224779974,0.946513834085734,
-1.98331976958516));
#26926=CARTESIAN_POINT('Ctrl Pts',(-0.478234529751121,1.0191711099922,-1.99390080177507));
#26927=CARTESIAN_POINT('Ctrl Pts',(-0.222597234321247,1.1004636264182,-2.01300274809229));
#26928=CARTESIAN_POINT('Ctrl Pts',(-0.0794663775051977,1.12675755955542,
-2.02317074675688));
#26929=CARTESIAN_POINT('Ctrl Pts',(0.232981315456759,1.10176800386665,-2.04552756527266));
#26930=CARTESIAN_POINT('Ctrl Pts',(0.37770060510901,1.06037143957915,-2.0560369702747));
#26931=CARTESIAN_POINT('Ctrl Pts',(0.604852724324514,0.944731736167629,
-2.07419440550631));
#26932=CARTESIAN_POINT('Ctrl Pts',(0.73133122698844,0.863974006299962,-2.08465639462863));
#26933=CARTESIAN_POINT('Ctrl Pts',(0.943397907937853,0.613934547622003,
-2.1080266301717));
#26934=CARTESIAN_POINT('Ctrl Pts',(1.01607631574406,0.484189787750191,-2.11841215189081));
#26935=CARTESIAN_POINT('Ctrl Pts',(1.11857306467121,0.173002860562993,-2.14176437012636));
#26936=CARTESIAN_POINT('Ctrl Pts',(1.12165266273671,0.0230529286474099,
-2.15222238737627));
#26937=CARTESIAN_POINT('Ctrl Pts',(1.10179845703878,-0.228016486144731,
-2.17016430609243));
#26938=CARTESIAN_POINT('Ctrl Pts',(1.06324590215938,-0.369253565391361,
-2.18039583379269));
#26939=CARTESIAN_POINT('Ctrl Pts',(0.924464855646204,-0.649976757040022,
-2.20272861706242));
#26940=CARTESIAN_POINT('Ctrl Pts',(0.825915661788621,-0.761161572818573,
-2.21310258159157));
#26941=CARTESIAN_POINT('Ctrl Pts',(0.626214316349864,-0.934430304671196,
-2.23193040825594));
#26942=CARTESIAN_POINT('Ctrl Pts',(0.50221499693755,-1.00732385711169,-2.24199298816798));
#26943=CARTESIAN_POINT('Ctrl Pts',(0.191201997533729,-1.11682300306852,
-2.26551693664132));
#26944=CARTESIAN_POINT('Ctrl Pts',(0.0349012702549763,-1.12007370080307,
-2.27638015858152));
#26945=CARTESIAN_POINT('Ctrl Pts',(-0.203851405860729,-1.1061171885703,
-2.29340869558083));
#26946=CARTESIAN_POINT('Ctrl Pts',(-0.341786112597017,-1.07261170247852,
-2.30334911559688));
#26947=CARTESIAN_POINT('Ctrl Pts',(-0.603413551668513,-0.951563052462853,
-2.32391815996146));
#26948=CARTESIAN_POINT('Ctrl Pts',(-0.725113385898934,-0.861211673415836,
-2.33450451982865));
#26949=CARTESIAN_POINT('Ctrl Pts',(-0.905273423514474,-0.663857977873341,
-2.35353245208202));
#26950=CARTESIAN_POINT('Ctrl Pts',(-0.989304020610889,-0.545163021076617,
-2.36369254095246));
#26951=CARTESIAN_POINT('Ctrl Pts',(-1.09791444748826,-0.250846118613211,
-2.38607028582539));
#26952=CARTESIAN_POINT('Ctrl Pts',(-1.12102369397598,-0.101931202388129,
-2.39659192327522));
#26953=CARTESIAN_POINT('Ctrl Pts',(-1.11127472608704,0.152382998725973,
-2.41472029922507));
#26954=CARTESIAN_POINT('Ctrl Pts',(-1.09120934524513,0.300938815206496,
-2.42517036237664));
#26955=CARTESIAN_POINT('Ctrl Pts',(-0.953355092950197,0.598483057720635,
-2.44854743454185));
#26956=CARTESIAN_POINT('Ctrl Pts',(-0.865889506205137,0.719096632405866,
-2.45895154517146));
#26957=CARTESIAN_POINT('Ctrl Pts',(-0.630908211369345,0.938430669099268,
-2.48186059631056));
#26958=CARTESIAN_POINT('Ctrl Pts',(-0.499473987912825,1.00559671816686,
-2.49216596514538));
#26959=CARTESIAN_POINT('Ctrl Pts',(-0.254954649474666,1.09592824110064,
-2.51073734053109));
#26960=CARTESIAN_POINT('Ctrl Pts',(-0.110233508147556,1.12012616746575,
-2.52099044678715));
#26961=CARTESIAN_POINT('Ctrl Pts',(0.202625788977262,1.11169037854405,-2.54330877782005));
#26962=CARTESIAN_POINT('Ctrl Pts',(0.344594062564991,1.06910154094398,-2.55366009735837));
#26963=CARTESIAN_POINT('Ctrl Pts',(0.586363065095521,0.959974916638415,
-2.57255024413075));
#26964=CARTESIAN_POINT('Ctrl Pts',(0.704733656287596,0.877644037487909,
-2.58263575715875));
#26965=CARTESIAN_POINT('Ctrl Pts',(0.924445762808999,0.651144082671885,
-2.60514789486952));
#26966=CARTESIAN_POINT('Ctrl Pts',(0.99587830302718,0.517818669122217,-2.61569215217414));
#26967=CARTESIAN_POINT('Ctrl Pts',(1.08982166380632,0.277939862987316,-2.63403504577381));
#26968=CARTESIAN_POINT('Ctrl Pts',(1.1169872981078,0.139044412854726,-2.64394629670335));
#26969=CARTESIAN_POINT('Ctrl Pts',(1.1169872981078,-0.139044412854725,-2.66378873021465));
#26970=CARTESIAN_POINT('Ctrl Pts',(1.08982166380632,-0.277939862987314,
-2.67369998114575));
#26971=CARTESIAN_POINT('Ctrl Pts',(0.995878303027182,-0.517818669122213,
-2.69204287474531));
#26972=CARTESIAN_POINT('Ctrl Pts',(0.924445762809003,-0.651144082671879,
-2.70258713204978));
#26973=CARTESIAN_POINT('Ctrl Pts',(0.704733656287605,-0.877644037487902,
-2.72509926976052));
#26974=CARTESIAN_POINT('Ctrl Pts',(0.586363065095532,-0.959974916638408,
-2.7351847827886));
#26975=CARTESIAN_POINT('Ctrl Pts',(0.344594062565008,-1.06910154094397,
-2.75407492956103));
#26976=CARTESIAN_POINT('Ctrl Pts',(0.202625788977281,-1.11169037854405,
-2.76442624909944));
#26977=CARTESIAN_POINT('Ctrl Pts',(-0.110233508147534,-1.12012616746575,
-2.78674458013225));
#26978=CARTESIAN_POINT('Ctrl Pts',(-0.254954649474639,-1.09592824110065,
-2.79699768638819));
#26979=CARTESIAN_POINT('Ctrl Pts',(-0.499473987912779,-1.00559671816688,
-2.81556906177376));
#26980=CARTESIAN_POINT('Ctrl Pts',(-0.6309082113693,-0.938430669099301,
-2.82587443060851));
#26981=CARTESIAN_POINT('Ctrl Pts',(-0.865889506205103,-0.719096632405906,
-2.84878348174746));
#26982=CARTESIAN_POINT('Ctrl Pts',(-0.953355092950165,-0.598483057720684,
-2.85918759237696));
#26983=CARTESIAN_POINT('Ctrl Pts',(-1.09120934524511,-0.300938815206566,
-2.88256466454204));
#26984=CARTESIAN_POINT('Ctrl Pts',(-1.11127472608703,-0.15238299872605,
-2.89301472769358));
#26985=CARTESIAN_POINT('Ctrl Pts',(-1.12102369397598,0.101931202388061,
-2.91114310364352));
#26986=CARTESIAN_POINT('Ctrl Pts',(-1.09791444748828,0.250846118613146,
-2.92166474109352));
#26987=CARTESIAN_POINT('Ctrl Pts',(-0.989304020610919,0.545163021076564,
-2.94404248596658));
#26988=CARTESIAN_POINT('Ctrl Pts',(-0.905273423514507,0.663857977873298,
-2.95420257483704));
#26989=CARTESIAN_POINT('Ctrl Pts',(-0.725113385898971,0.861211673415808,
-2.97323050709035));
#26990=CARTESIAN_POINT('Ctrl Pts',(-0.603413551668552,0.951563052462833,
-2.98381686695739));
#26991=CARTESIAN_POINT('Ctrl Pts',(-0.341786112597064,1.07261170247852,
-3.00438591132201));
#26992=CARTESIAN_POINT('Ctrl Pts',(-0.203851405860783,1.10611718857029,
-3.0143263313382));
#26993=CARTESIAN_POINT('Ctrl Pts',(0.0349012702549246,1.12007370080308,
-3.03135486833769));
#26994=CARTESIAN_POINT('Ctrl Pts',(0.191201997533667,1.11682300306852,-3.04221809027818));
#26995=CARTESIAN_POINT('Ctrl Pts',(0.502214996937503,1.00732385711169,-3.06574203875153));
#26996=CARTESIAN_POINT('Ctrl Pts',(0.626214316349839,0.934430304671182,
-3.0758046186634));
#26997=CARTESIAN_POINT('Ctrl Pts',(0.825915661788615,0.761161572818546,
-3.09463244532758));
#26998=CARTESIAN_POINT('Ctrl Pts',(0.924464855646201,0.64997675704,-3.10500640985651));
#26999=CARTESIAN_POINT('Ctrl Pts',(1.06324590215937,0.36925356539136,-3.12733919312616));
#27000=CARTESIAN_POINT('Ctrl Pts',(1.10179845703877,0.228016486144748,-3.13757072082647));
#27001=CARTESIAN_POINT('Ctrl Pts',(1.12165266273671,-0.0230529286473686,
-3.15551263954268));
#27002=CARTESIAN_POINT('Ctrl Pts',(1.11857306467121,-0.173002860562954,
-3.16597065679267));
#27003=CARTESIAN_POINT('Ctrl Pts',(1.01607631574407,-0.484189787750162,
-3.18932287502831));
#27004=CARTESIAN_POINT('Ctrl Pts',(0.94339790793787,-0.613934547621978,
-3.19970839674746));
#27005=CARTESIAN_POINT('Ctrl Pts',(0.731331226988465,-0.86397400629994,
-3.22307863229059));
#27006=CARTESIAN_POINT('Ctrl Pts',(0.604852724324542,-0.944731736167613,
-3.23354062141293));
#27007=CARTESIAN_POINT('Ctrl Pts',(0.377700605109028,-1.06037143957914,
-3.25169805664457));
#27008=CARTESIAN_POINT('Ctrl Pts',(0.232981315456776,-1.10176800386664,
-3.26220746164662));
#27009=CARTESIAN_POINT('Ctrl Pts',(-0.0794663775051832,-1.12675755955542,
-3.28456428016241));
#27010=CARTESIAN_POINT('Ctrl Pts',(-0.222597234321235,-1.1004636264182,
-3.294732278827));
#27011=CARTESIAN_POINT('Ctrl Pts',(-0.47823452975111,-1.0191711099922,-3.31383422514422));
#27012=CARTESIAN_POINT('Ctrl Pts',(-0.61118224779973,-0.946513834085741,
-3.32441525733414));
#27013=CARTESIAN_POINT('Ctrl Pts',(-0.840538191683135,-0.751460714065271,
-3.345898011639));
#27014=CARTESIAN_POINT('Ctrl Pts',(-0.9255889082428,-0.636392952388535,
-3.3559100952136));
#27015=CARTESIAN_POINT('Ctrl Pts',(-1.02997735713433,-0.440477084842065,
-3.37171618375233));
#27016=CARTESIAN_POINT('Ctrl Pts',(-1.09418460733438,-0.296790717289765,
-3.38263809987196));
#27017=CARTESIAN_POINT('Ctrl Pts',(-1.1250370353998,0.0352369170928032,
-3.40642866117045));
#27018=CARTESIAN_POINT('Ctrl Pts',(-1.11066616674449,0.178042375581391,
-3.41647070761312));
#27019=CARTESIAN_POINT('Ctrl Pts',(-1.03703915589555,0.431145768277807,
-3.4352412199916));
#27020=CARTESIAN_POINT('Ctrl Pts',(-0.977352549963121,0.567498199932441,
-3.44563223691794));
#27021=CARTESIAN_POINT('Ctrl Pts',(-0.78038305541925,0.811029500761437,
-3.46797004573511));
#27022=CARTESIAN_POINT('Ctrl Pts',(-0.668471432388838,0.904915646636014,
-3.47817926042074));
#27023=CARTESIAN_POINT('Ctrl Pts',(-0.461203748610943,1.02120417552907,
-3.49510952128985));
#27024=CARTESIAN_POINT('Ctrl Pts',(-0.372801878430417,1.05728988862616,
-3.50186529968027));
#27025=CARTESIAN_POINT('Ctrl Pts',(-0.189124507262864,1.1048491526056,-3.51540775381488));
#27026=CARTESIAN_POINT('Ctrl Pts',(-0.0945477069597182,1.11645974724111,
-3.52214984360044));
#27027=CARTESIAN_POINT('Ctrl Pts',(-2.02707199615241E-6,1.11628565404413,
-3.52888591117587));
#27028=CARTESIAN_POINT('Ctrl Pts',(0.4696881186261,-0.9981380597272,-1.735864569721));
#27029=CARTESIAN_POINT('Ctrl Pts',(0.2318942596183,-1.110035356068,-1.754822903054));
#27030=CARTESIAN_POINT('Ctrl Pts',(-0.3258579542137,-1.155927922117,-1.792739569721));
#27031=CARTESIAN_POINT('Ctrl Pts',(-1.003936318643,-0.6594544137959,-1.849614569721));
#27032=CARTESIAN_POINT('Ctrl Pts',(-1.190400720751,0.1598981886148,-1.906489569721));
#27033=CARTESIAN_POINT('Ctrl Pts',(-0.7943069665412,0.9009591520544,-1.963364569721));
#27034=CARTESIAN_POINT('Ctrl Pts',(-0.009432467987834,1.201066414053,-2.020239569721));
#27035=CARTESIAN_POINT('Ctrl Pts',(0.7800537946193,0.9133258114035,-2.077114569721));
#27036=CARTESIAN_POINT('Ctrl Pts',(1.187754649245,0.1785709428966,-2.133989569721));
#27037=CARTESIAN_POINT('Ctrl Pts',(1.014124826746,-0.6435832038027,-2.190864569721));
#27038=CARTESIAN_POINT('Ctrl Pts',(0.3441455177085,-1.150744276231,-2.247739569721));
#27039=CARTESIAN_POINT('Ctrl Pts',(-0.4942711510281,-1.094689252768,-2.304614569721));
#27040=CARTESIAN_POINT('Ctrl Pts',(-1.090773532456,-0.5028534860695,-2.361489569721));
#27041=CARTESIAN_POINT('Ctrl Pts',(-1.153411671532,0.3350970673819,-2.418364569721));
#27042=CARTESIAN_POINT('Ctrl Pts',(-0.6515281822355,1.009038926982,-2.475239569721));
#27043=CARTESIAN_POINT('Ctrl Pts',(0.169236898936,1.189120431432,-2.532114569721));
#27044=CARTESIAN_POINT('Ctrl Pts',(0.9071712857378,0.7872031419892,-2.588989569721));
#27045=CARTESIAN_POINT('Ctrl Pts',(1.201103046544,0.,-2.645864569721));
#27046=CARTESIAN_POINT('Ctrl Pts',(0.9071712857378,-0.7872031419892,-2.702739569721));
#27047=CARTESIAN_POINT('Ctrl Pts',(0.169236898936,-1.189120431432,-2.759614569721));
#27048=CARTESIAN_POINT('Ctrl Pts',(-0.6515281822355,-1.009038926982,-2.816489569721));
#27049=CARTESIAN_POINT('Ctrl Pts',(-1.153411671532,-0.3350970673819,-2.873364569721));
#27050=CARTESIAN_POINT('Ctrl Pts',(-1.090773532456,0.5028534860695,-2.930239569721));
#27051=CARTESIAN_POINT('Ctrl Pts',(-0.4942711510281,1.094689252768,-2.987114569721));
#27052=CARTESIAN_POINT('Ctrl Pts',(0.3441455177085,1.150744276231,-3.043989569721));
#27053=CARTESIAN_POINT('Ctrl Pts',(1.014124826746,0.6435832038027,-3.100864569721));
#27054=CARTESIAN_POINT('Ctrl Pts',(1.187754649245,-0.1785709428966,-3.157739569721));
#27055=CARTESIAN_POINT('Ctrl Pts',(0.7800537946193,-0.9133258114035,-3.214614569721));
#27056=CARTESIAN_POINT('Ctrl Pts',(-0.009432467987832,-1.201066414053,-3.271489569721));
#27057=CARTESIAN_POINT('Ctrl Pts',(-0.7943069665412,-0.9009591520544,-3.328364569721));
#27058=CARTESIAN_POINT('Ctrl Pts',(-1.190400720751,-0.1598981886148,-3.385239569721));
#27059=CARTESIAN_POINT('Ctrl Pts',(-1.003936318643,0.6594544137959,-3.442114569721));
#27060=CARTESIAN_POINT('Ctrl Pts',(-0.3258579542138,1.155927922117,-3.498989569721));
#27061=CARTESIAN_POINT('Ctrl Pts',(0.2318942596183,1.110035356068,-3.536906236387));
#27062=CARTESIAN_POINT('Ctrl Pts',(0.4696881186261,0.9981380597272,-3.555864569721));
#27063=CARTESIAN_POINT('Ctrl Pts',(0.5279823721497,-1.122019654338,-1.814910694393));
#27064=CARTESIAN_POINT('Ctrl Pts',(0.2606752788197,-1.247804824574,-1.833869027727));
#27065=CARTESIAN_POINT('Ctrl Pts',(-0.3663010598456,-1.299393240218,-1.871785694393));
#27066=CARTESIAN_POINT('Ctrl Pts',(-1.128537550737,-0.7413010717389,-1.928660694393));
#27067=CARTESIAN_POINT('Ctrl Pts',(-1.33814455045,0.1797435821333,-1.985535694393));
#27068=CARTESIAN_POINT('Ctrl Pts',(-0.892890536887,1.012779611507,-2.042410694393));
#27069=CARTESIAN_POINT('Ctrl Pts',(-0.01060315691615,1.350133991585,-2.099285694393));
#27070=CARTESIAN_POINT('Ctrl Pts',(0.8768683655278,1.026681130153,-2.156160694393));
#27071=CARTESIAN_POINT('Ctrl Pts',(1.335170067905,0.2007338620856,-2.213035694393));
#27072=CARTESIAN_POINT('Ctrl Pts',(1.139990581936,-0.723460043259,-2.269910694393));
#27073=CARTESIAN_POINT('Ctrl Pts',(0.3868583419482,-1.293566238123,-2.326785694393));
#27074=CARTESIAN_POINT('Ctrl Pts',(-0.555616470709,-1.230554075189,-2.383660694393));
#27075=CARTESIAN_POINT('Ctrl Pts',(-1.226152364316,-0.5652639823961,-2.440535694393));
#27076=CARTESIAN_POINT('Ctrl Pts',(-1.296564691016,0.3766868641562,-2.497410694393));
#27077=CARTESIAN_POINT('Ctrl Pts',(-0.7323910942975,1.134273457497,-2.554285694393));
#27078=CARTESIAN_POINT('Ctrl Pts',(0.190241344867,1.336705360987,-2.611160694393));
#27079=CARTESIAN_POINT('Ctrl Pts',(1.019762749782,0.8849050375959,-2.668035694393));
#27080=CARTESIAN_POINT('Ctrl Pts',(1.350175170634,0.,-2.724910694393));
#27081=CARTESIAN_POINT('Ctrl Pts',(1.019762749782,-0.8849050375959,-2.781785694393));
#27082=CARTESIAN_POINT('Ctrl Pts',(0.190241344867,-1.336705360987,-2.838660694393));
#27083=CARTESIAN_POINT('Ctrl Pts',(-0.7323910942975,-1.134273457497,-2.895535694393));
#27084=CARTESIAN_POINT('Ctrl Pts',(-1.296564691016,-0.3766868641562,-2.952410694393));
#27085=CARTESIAN_POINT('Ctrl Pts',(-1.226152364316,0.5652639823961,-3.009285694393));
#27086=CARTESIAN_POINT('Ctrl Pts',(-0.555616470709,1.230554075189,-3.066160694393));
#27087=CARTESIAN_POINT('Ctrl Pts',(0.3868583419482,1.293566238123,-3.123035694393));
#27088=CARTESIAN_POINT('Ctrl Pts',(1.139990581936,0.723460043259,-3.179910694393));
#27089=CARTESIAN_POINT('Ctrl Pts',(1.335170067905,-0.2007338620856,-3.236785694393));
#27090=CARTESIAN_POINT('Ctrl Pts',(0.8768683655278,-1.026681130153,-3.293660694393));
#27091=CARTESIAN_POINT('Ctrl Pts',(-0.01060315691615,-1.350133991585,-3.350535694393));
#27092=CARTESIAN_POINT('Ctrl Pts',(-0.892890536887,-1.012779611507,-3.407410694393));
#27093=CARTESIAN_POINT('Ctrl Pts',(-1.33814455045,-0.1797435821333,-3.464285694393));
#27094=CARTESIAN_POINT('Ctrl Pts',(-1.128537550737,0.7413010717389,-3.521160694393));
#27095=CARTESIAN_POINT('Ctrl Pts',(-0.3663010598456,1.299393240218,-3.578035694393));
#27096=CARTESIAN_POINT('Ctrl Pts',(0.2606752788197,1.247804824574,-3.61595236106));
#27097=CARTESIAN_POINT('Ctrl Pts',(0.5279823721497,1.122019654338,-3.634910694393));
#27098=CARTESIAN_POINT('Ctrl Pts',(0.5862766256734,-1.24590124895,-1.893956819066));
#27099=CARTESIAN_POINT('Ctrl Pts',(0.2894562980212,-1.38557429308,-1.912915152399));
#27100=CARTESIAN_POINT('Ctrl Pts',(-0.4067441654775,-1.442858558319,-1.950831819066));
#27101=CARTESIAN_POINT('Ctrl Pts',(-1.253138782831,-0.823147729682,-2.007706819066));
#27102=CARTESIAN_POINT('Ctrl Pts',(-1.48588838015,0.1995889756518,-2.064581819066));
#27103=CARTESIAN_POINT('Ctrl Pts',(-0.9914741072328,1.12460007096,-2.121456819066));
#27104=CARTESIAN_POINT('Ctrl Pts',(-0.01177384584446,1.499201569118,-2.178331819066));
#27105=CARTESIAN_POINT('Ctrl Pts',(0.9736829364363,1.140036448902,-2.235206819066));
#27106=CARTESIAN_POINT('Ctrl Pts',(1.482585486565,0.2228967812747,-2.292081819066));
#27107=CARTESIAN_POINT('Ctrl Pts',(1.265856337127,-0.8033368827153,-2.348956819066));
#27108=CARTESIAN_POINT('Ctrl Pts',(0.4295711661878,-1.436388200015,-2.405831819066));
#27109=CARTESIAN_POINT('Ctrl Pts',(-0.61696179039,-1.36641889761,-2.462706819066));
#27110=CARTESIAN_POINT('Ctrl Pts',(-1.361531196175,-0.6276744787227,-2.519581819066));
#27111=CARTESIAN_POINT('Ctrl Pts',(-1.439717710501,0.4182766609306,-2.576456819066));
#27112=CARTESIAN_POINT('Ctrl Pts',(-0.8132540063595,1.259507988013,-2.633331819066));
#27113=CARTESIAN_POINT('Ctrl Pts',(0.211245790798,1.484290290542,-2.690206819066));
#27114=CARTESIAN_POINT('Ctrl Pts',(1.132354213826,0.9826069332027,-2.747081819066));
#27115=CARTESIAN_POINT('Ctrl Pts',(1.499247294724,0.,-2.803956819066));
#27116=CARTESIAN_POINT('Ctrl Pts',(1.132354213826,-0.9826069332027,-2.860831819066));
#27117=CARTESIAN_POINT('Ctrl Pts',(0.211245790798,-1.484290290542,-2.917706819066));
#27118=CARTESIAN_POINT('Ctrl Pts',(-0.8132540063595,-1.259507988013,-2.974581819066));
#27119=CARTESIAN_POINT('Ctrl Pts',(-1.439717710501,-0.4182766609306,-3.031456819066));
#27120=CARTESIAN_POINT('Ctrl Pts',(-1.361531196175,0.6276744787227,-3.088331819066));
#27121=CARTESIAN_POINT('Ctrl Pts',(-0.61696179039,1.36641889761,-3.145206819066));
#27122=CARTESIAN_POINT('Ctrl Pts',(0.4295711661878,1.436388200015,-3.202081819066));
#27123=CARTESIAN_POINT('Ctrl Pts',(1.265856337127,0.8033368827153,-3.258956819066));
#27124=CARTESIAN_POINT('Ctrl Pts',(1.482585486565,-0.2228967812747,-3.315831819066));
#27125=CARTESIAN_POINT('Ctrl Pts',(0.9736829364363,-1.140036448902,-3.372706819066));
#27126=CARTESIAN_POINT('Ctrl Pts',(-0.01177384584446,-1.499201569118,-3.429581819066));
#27127=CARTESIAN_POINT('Ctrl Pts',(-0.9914741072328,-1.12460007096,-3.486456819066));
#27128=CARTESIAN_POINT('Ctrl Pts',(-1.48588838015,-0.1995889756517,-3.543331819066));
#27129=CARTESIAN_POINT('Ctrl Pts',(-1.253138782831,0.823147729682,-3.600206819066));
#27130=CARTESIAN_POINT('Ctrl Pts',(-0.4067441654775,1.442858558319,-3.657081819066));
#27131=CARTESIAN_POINT('Ctrl Pts',(0.2894562980212,1.38557429308,-3.694998485733));
#27132=CARTESIAN_POINT('Ctrl Pts',(0.5862766256734,1.24590124895,-3.713956819066));
#27133=CARTESIAN_POINT('Ctrl Pts',(0.644570879197,-1.369782843561,-1.973002943739));
#27134=CARTESIAN_POINT('Ctrl Pts',(0.3182373172226,-1.523343761587,-1.991961277072));
#27135=CARTESIAN_POINT('Ctrl Pts',(-0.4471872711094,-1.586323876419,-2.029877943739));
#27136=CARTESIAN_POINT('Ctrl Pts',(-1.377740014924,-0.904994387625,-2.086752943739));
#27137=CARTESIAN_POINT('Ctrl Pts',(-1.633632209849,0.2194343691702,-2.143627943739));
#27138=CARTESIAN_POINT('Ctrl Pts',(-1.090057677579,1.236420530413,-2.200502943739));
#27139=CARTESIAN_POINT('Ctrl Pts',(-0.01294453477278,1.648269146651,-2.257377943739));
#27140=CARTESIAN_POINT('Ctrl Pts',(1.070497507345,1.253391767652,-2.314252943739));
#27141=CARTESIAN_POINT('Ctrl Pts',(1.630000905225,0.2450597004638,-2.371127943739));
#27142=CARTESIAN_POINT('Ctrl Pts',(1.391722092318,-0.8832137221716,-2.428002943739));
#27143=CARTESIAN_POINT('Ctrl Pts',(0.4722839904274,-1.579210161907,-2.484877943739));
#27144=CARTESIAN_POINT('Ctrl Pts',(-0.6783071100709,-1.502283720031,-2.541752943739));
#27145=CARTESIAN_POINT('Ctrl Pts',(-1.496910028035,-0.6900849750494,-2.598627943739));
#27146=CARTESIAN_POINT('Ctrl Pts',(-1.582870729986,0.4598664577049,-2.655502943739));
#27147=CARTESIAN_POINT('Ctrl Pts',(-0.8941169184215,1.384742518528,-2.712377943739));
#27148=CARTESIAN_POINT('Ctrl Pts',(0.232250236729,1.631875220096,-2.769252943739));
#27149=CARTESIAN_POINT('Ctrl Pts',(1.24494567787,1.080308828809,-2.826127943739));
#27150=CARTESIAN_POINT('Ctrl Pts',(1.648319418813,0.,-2.883002943739));
#27151=CARTESIAN_POINT('Ctrl Pts',(1.24494567787,-1.080308828809,-2.939877943739));
#27152=CARTESIAN_POINT('Ctrl Pts',(0.232250236729,-1.631875220096,-2.996752943739));
#27153=CARTESIAN_POINT('Ctrl Pts',(-0.8941169184215,-1.384742518528,-3.053627943739));
#27154=CARTESIAN_POINT('Ctrl Pts',(-1.582870729986,-0.4598664577049,-3.110502943739));
#27155=CARTESIAN_POINT('Ctrl Pts',(-1.496910028035,0.6900849750494,-3.167377943739));
#27156=CARTESIAN_POINT('Ctrl Pts',(-0.6783071100709,1.502283720031,-3.224252943739));
#27157=CARTESIAN_POINT('Ctrl Pts',(0.4722839904274,1.579210161907,-3.281127943739));
#27158=CARTESIAN_POINT('Ctrl Pts',(1.391722092318,0.8832137221716,-3.338002943739));
#27159=CARTESIAN_POINT('Ctrl Pts',(1.630000905225,-0.2450597004638,-3.394877943739));
#27160=CARTESIAN_POINT('Ctrl Pts',(1.070497507345,-1.253391767652,-3.451752943739));
#27161=CARTESIAN_POINT('Ctrl Pts',(-0.01294453477277,-1.648269146651,-3.508627943739));
#27162=CARTESIAN_POINT('Ctrl Pts',(-1.090057677579,-1.236420530413,-3.565502943739));
#27163=CARTESIAN_POINT('Ctrl Pts',(-1.633632209849,-0.2194343691702,-3.622377943739));
#27164=CARTESIAN_POINT('Ctrl Pts',(-1.377740014924,0.904994387625,-3.679252943739));
#27165=CARTESIAN_POINT('Ctrl Pts',(-0.4471872711094,1.586323876419,-3.736127943739));
#27166=CARTESIAN_POINT('Ctrl Pts',(0.3182373172226,1.523343761587,-3.774044610405));
#27167=CARTESIAN_POINT('Ctrl Pts',(0.644570879197,1.369782843561,-3.793002943739));
#27168=CARTESIAN_POINT('',(-1.98293436576097E-9,1.49923261688451,-3.74955700104142));
#27169=CARTESIAN_POINT('',(0.,1.116987298108,-3.528867513459));
#27170=CARTESIAN_POINT('Ctrl Pts',(-2.23097736339398E-5,1.49898153286063,
-3.74997329818232));
#27171=CARTESIAN_POINT('Ctrl Pts',(-0.134297990364599,1.49921292012494,
-3.74284084449308));
#27172=CARTESIAN_POINT('Ctrl Pts',(-0.268638579334411,1.4817717682223,-3.73571955672579));
#27173=CARTESIAN_POINT('Ctrl Pts',(-0.528263299353071,1.41043848354384,
-3.7214835046435));
#27174=CARTESIAN_POINT('Ctrl Pts',(-0.652764717085495,1.35640654604196,
-3.71435338885275));
#27175=CARTESIAN_POINT('Ctrl Pts',(-0.93173523235398,1.1891402211788,-3.69707781285224));
#27176=CARTESIAN_POINT('Ctrl Pts',(-1.07750856874978,1.05993244186351,-3.68689192394793));
#27177=CARTESIAN_POINT('Ctrl Pts',(-1.25254458058096,0.831135438061306,
-3.67160665077089));
#27178=CARTESIAN_POINT('Ctrl Pts',(-1.30304061564861,0.74921731834058,-3.66653951792222));
#27179=CARTESIAN_POINT('Ctrl Pts',(-1.43181232730633,0.485623094910584,
-3.65097008072865));
#27180=CARTESIAN_POINT('Ctrl Pts',(-1.48316632248211,0.291366952803233,
-3.64048349674964));
#27181=CARTESIAN_POINT('Ctrl Pts',(-1.50934594069338,-0.102298203372775,
-3.61953593410385));
#27182=CARTESIAN_POINT('Ctrl Pts',(-1.48352322466648,-0.297075624561851,
-3.60935212892794));
#27183=CARTESIAN_POINT('Ctrl Pts',(-1.35557800746622,-0.667978453013121,
-3.58851892695713));
#27184=CARTESIAN_POINT('Ctrl Pts',(-1.25672305133621,-0.839706849423558,
-3.57816968266589));
#27185=CARTESIAN_POINT('Ctrl Pts',(-1.06762968939388,-1.05767327012927,
-3.5628546682347));
#27186=CARTESIAN_POINT('Ctrl Pts',(-0.999122949219283,-1.12299757074587,
-3.55786874093753));
#27187=CARTESIAN_POINT('Ctrl Pts',(-0.767475932851098,-1.30345310761049,
-3.54230752101967));
#27188=CARTESIAN_POINT('Ctrl Pts',(-0.585984095946929,-1.39346685040132,
-3.53173765623922));
#27189=CARTESIAN_POINT('Ctrl Pts',(-0.300277764313124,-1.47207219521031,
-3.51599600554029));
#27190=CARTESIAN_POINT('Ctrl Pts',(-0.203413451744069,-1.48897913532964,
-3.51079851028164));
#27191=CARTESIAN_POINT('Ctrl Pts',(-0.0102966124493356,-1.50310836142732,
-3.50053281146868));
#27192=CARTESIAN_POINT('Ctrl Pts',(0.0847306681168998,-1.50057826174177,
-3.49552882854339));
#27193=CARTESIAN_POINT('Ctrl Pts',(0.371065755655233,-1.46518483944735,
-3.48022026878835));
#27194=CARTESIAN_POINT('Ctrl Pts',(0.558528693198532,-1.4040395721907,-3.46992086661752));
#27195=CARTESIAN_POINT('Ctrl Pts',(0.90153284875694,-1.21492375687663,-3.44911971811302));
#27196=CARTESIAN_POINT('Ctrl Pts',(1.05210335279266,-1.08744425337218,-3.43889366904479));
#27197=CARTESIAN_POINT('Ctrl Pts',(1.29645238593754,-0.777009497911457,
-3.41791551601252));
#27198=CARTESIAN_POINT('Ctrl Pts',(1.38796572683809,-0.59897640207039,-3.40746395634614));
#27199=CARTESIAN_POINT('Ctrl Pts',(1.49653070285487,-0.222284526241667,
-3.38665963898178));
#27200=CARTESIAN_POINT('Ctrl Pts',(1.51209522337162,-0.030383558262909,
-3.37667624280134));
#27201=CARTESIAN_POINT('Ctrl Pts',(1.46756784636134,0.362285640434857,-3.35568821166625));
#27202=CARTESIAN_POINT('Ctrl Pts',(1.4068673977224,0.555204171359176,-3.34513613647265));
#27203=CARTESIAN_POINT('Ctrl Pts',(1.2647554046479,0.812299723145478,-3.32955745876526));
#27204=CARTESIAN_POINT('Ctrl Pts',(1.21076623735938,0.890422663210658,-3.32455458934434));
#27205=CARTESIAN_POINT('Ctrl Pts',(1.02479816055779,1.11092233383098,-3.30923718460512));
#27206=CARTESIAN_POINT('Ctrl Pts',(0.871086100543727,1.23469586808278,-3.29892246712298));
#27207=CARTESIAN_POINT('Ctrl Pts',(0.593490819192611,1.38245304443696,-3.28222967441605));
#27208=CARTESIAN_POINT('Ctrl Pts',(0.479555239505383,1.42667704405794,-3.27581122112143));
#27209=CARTESIAN_POINT('Ctrl Pts',(0.242844402015829,1.48495859802652,-3.26291338963858));
#27210=CARTESIAN_POINT('Ctrl Pts',(0.121403313286431,1.49919069968979,-3.25647421623353));
#27211=CARTESIAN_POINT('Ctrl Pts',(2.23097736028535E-5,1.49898153286063,
-3.25002670181768));
#27212=CARTESIAN_POINT('Ctrl Pts',(-0.644570879197,1.369782843561,-3.206997056261));
#27213=CARTESIAN_POINT('Ctrl Pts',(-0.3182373172226,1.523343761587,-3.225955389595));
#27214=CARTESIAN_POINT('Ctrl Pts',(0.4471872711094,1.586323876419,-3.263872056261));
#27215=CARTESIAN_POINT('Ctrl Pts',(1.377740014924,0.904994387625,-3.320747056261));
#27216=CARTESIAN_POINT('Ctrl Pts',(1.633632209849,-0.2194343691702,-3.377622056261));
#27217=CARTESIAN_POINT('Ctrl Pts',(1.090057677579,-1.236420530413,-3.434497056261));
#27218=CARTESIAN_POINT('Ctrl Pts',(0.01294453477278,-1.648269146651,-3.491372056261));
#27219=CARTESIAN_POINT('Ctrl Pts',(-1.070497507345,-1.253391767652,-3.548247056261));
#27220=CARTESIAN_POINT('Ctrl Pts',(-1.630000905225,-0.2450597004638,-3.605122056261));
#27221=CARTESIAN_POINT('Ctrl Pts',(-1.391722092318,0.8832137221716,-3.661997056261));
#27222=CARTESIAN_POINT('Ctrl Pts',(-0.4722839904274,1.579210161907,-3.718872056261));
#27223=CARTESIAN_POINT('Ctrl Pts',(0.6783071100709,1.502283720031,-3.775747056261));
#27224=CARTESIAN_POINT('Ctrl Pts',(1.496910028035,0.6900849750494,-3.832622056261));
#27225=CARTESIAN_POINT('Ctrl Pts',(1.582870729986,-0.4598664577049,-3.889497056261));
#27226=CARTESIAN_POINT('Ctrl Pts',(0.8941169184216,-1.384742518528,-3.946372056261));
#27227=CARTESIAN_POINT('Ctrl Pts',(-0.232250236729,-1.631875220096,-4.003247056261));
#27228=CARTESIAN_POINT('Ctrl Pts',(-1.24494567787,-1.080308828809,-4.060122056261));
#27229=CARTESIAN_POINT('Ctrl Pts',(-1.648319418813,0.,-4.116997056261));
#27230=CARTESIAN_POINT('Ctrl Pts',(-1.24494567787,1.080308828809,-4.173872056261));
#27231=CARTESIAN_POINT('Ctrl Pts',(-0.232250236729,1.631875220096,-4.230747056261));
#27232=CARTESIAN_POINT('Ctrl Pts',(0.8941169184215,1.384742518528,-4.287622056261));
#27233=CARTESIAN_POINT('Ctrl Pts',(1.582870729986,0.4598664577049,-4.344497056261));
#27234=CARTESIAN_POINT('Ctrl Pts',(1.496910028035,-0.6900849750494,-4.401372056261));
#27235=CARTESIAN_POINT('Ctrl Pts',(0.6783071100709,-1.502283720031,-4.458247056261));
#27236=CARTESIAN_POINT('Ctrl Pts',(-0.4722839904274,-1.579210161907,-4.515122056261));
#27237=CARTESIAN_POINT('Ctrl Pts',(-1.391722092318,-0.8832137221716,-4.571997056261));
#27238=CARTESIAN_POINT('Ctrl Pts',(-1.630000905225,0.2450597004637,-4.628872056261));
#27239=CARTESIAN_POINT('Ctrl Pts',(-1.070497507345,1.253391767652,-4.685747056261));
#27240=CARTESIAN_POINT('Ctrl Pts',(0.01294453477278,1.648269146651,-4.742622056261));
#27241=CARTESIAN_POINT('Ctrl Pts',(1.090057677579,1.236420530413,-4.799497056261));
#27242=CARTESIAN_POINT('Ctrl Pts',(1.633632209849,0.2194343691702,-4.856372056261));
#27243=CARTESIAN_POINT('Ctrl Pts',(1.377740014924,-0.904994387625,-4.913247056261));
#27244=CARTESIAN_POINT('Ctrl Pts',(0.4471872711094,-1.586323876419,-4.970122056261));
#27245=CARTESIAN_POINT('Ctrl Pts',(-0.3182373172226,-1.523343761587,-5.008038722928));
#27246=CARTESIAN_POINT('Ctrl Pts',(-0.644570879197,-1.369782843561,-5.026997056261));
#27247=CARTESIAN_POINT('Ctrl Pts',(-0.5862766256734,1.24590124895,-3.286043180934));
#27248=CARTESIAN_POINT('Ctrl Pts',(-0.2894562980212,1.38557429308,-3.305001514267));
#27249=CARTESIAN_POINT('Ctrl Pts',(0.4067441654775,1.442858558319,-3.342918180934));
#27250=CARTESIAN_POINT('Ctrl Pts',(1.253138782831,0.823147729682,-3.399793180934));
#27251=CARTESIAN_POINT('Ctrl Pts',(1.48588838015,-0.1995889756518,-3.456668180934));
#27252=CARTESIAN_POINT('Ctrl Pts',(0.9914741072328,-1.12460007096,-3.513543180934));
#27253=CARTESIAN_POINT('Ctrl Pts',(0.01177384584447,-1.499201569118,-3.570418180934));
#27254=CARTESIAN_POINT('Ctrl Pts',(-0.9736829364363,-1.140036448902,-3.627293180934));
#27255=CARTESIAN_POINT('Ctrl Pts',(-1.482585486565,-0.2228967812747,-3.684168180934));
#27256=CARTESIAN_POINT('Ctrl Pts',(-1.265856337127,0.8033368827153,-3.741043180934));
#27257=CARTESIAN_POINT('Ctrl Pts',(-0.4295711661878,1.436388200015,-3.797918180934));
#27258=CARTESIAN_POINT('Ctrl Pts',(0.61696179039,1.36641889761,-3.854793180934));
#27259=CARTESIAN_POINT('Ctrl Pts',(1.361531196175,0.6276744787227,-3.911668180934));
#27260=CARTESIAN_POINT('Ctrl Pts',(1.439717710501,-0.4182766609306,-3.968543180934));
#27261=CARTESIAN_POINT('Ctrl Pts',(0.8132540063595,-1.259507988013,-4.025418180934));
#27262=CARTESIAN_POINT('Ctrl Pts',(-0.211245790798,-1.484290290542,-4.082293180934));
#27263=CARTESIAN_POINT('Ctrl Pts',(-1.132354213826,-0.9826069332027,-4.139168180934));
#27264=CARTESIAN_POINT('Ctrl Pts',(-1.499247294724,0.,-4.196043180934));
#27265=CARTESIAN_POINT('Ctrl Pts',(-1.132354213826,0.9826069332027,-4.252918180934));
#27266=CARTESIAN_POINT('Ctrl Pts',(-0.211245790798,1.484290290542,-4.309793180934));
#27267=CARTESIAN_POINT('Ctrl Pts',(0.8132540063595,1.259507988013,-4.366668180934));
#27268=CARTESIAN_POINT('Ctrl Pts',(1.439717710501,0.4182766609306,-4.423543180934));
#27269=CARTESIAN_POINT('Ctrl Pts',(1.361531196175,-0.6276744787227,-4.480418180934));
#27270=CARTESIAN_POINT('Ctrl Pts',(0.61696179039,-1.36641889761,-4.537293180934));
#27271=CARTESIAN_POINT('Ctrl Pts',(-0.4295711661878,-1.436388200015,-4.594168180934));
#27272=CARTESIAN_POINT('Ctrl Pts',(-1.265856337127,-0.8033368827153,-4.651043180934));
#27273=CARTESIAN_POINT('Ctrl Pts',(-1.482585486565,0.2228967812747,-4.707918180934));
#27274=CARTESIAN_POINT('Ctrl Pts',(-0.9736829364363,1.140036448902,-4.764793180934));
#27275=CARTESIAN_POINT('Ctrl Pts',(0.01177384584446,1.499201569118,-4.821668180934));
#27276=CARTESIAN_POINT('Ctrl Pts',(0.9914741072328,1.12460007096,-4.878543180934));
#27277=CARTESIAN_POINT('Ctrl Pts',(1.48588838015,0.1995889756517,-4.935418180934));
#27278=CARTESIAN_POINT('Ctrl Pts',(1.253138782831,-0.823147729682,-4.992293180934));
#27279=CARTESIAN_POINT('Ctrl Pts',(0.4067441654775,-1.442858558319,-5.049168180934));
#27280=CARTESIAN_POINT('Ctrl Pts',(-0.2894562980212,-1.38557429308,-5.087084847601));
#27281=CARTESIAN_POINT('Ctrl Pts',(-0.5862766256734,-1.24590124895,-5.106043180934));
#27282=CARTESIAN_POINT('Ctrl Pts',(-0.5279823721497,1.122019654338,-3.365089305607));
#27283=CARTESIAN_POINT('Ctrl Pts',(-0.2606752788197,1.247804824574,-3.38404763894));
#27284=CARTESIAN_POINT('Ctrl Pts',(0.3663010598456,1.299393240218,-3.421964305607));
#27285=CARTESIAN_POINT('Ctrl Pts',(1.128537550737,0.7413010717389,-3.478839305607));
#27286=CARTESIAN_POINT('Ctrl Pts',(1.33814455045,-0.1797435821333,-3.535714305607));
#27287=CARTESIAN_POINT('Ctrl Pts',(0.892890536887,-1.012779611507,-3.592589305607));
#27288=CARTESIAN_POINT('Ctrl Pts',(0.01060315691615,-1.350133991585,-3.649464305607));
#27289=CARTESIAN_POINT('Ctrl Pts',(-0.8768683655278,-1.026681130153,-3.706339305607));
#27290=CARTESIAN_POINT('Ctrl Pts',(-1.335170067905,-0.2007338620856,-3.763214305607));
#27291=CARTESIAN_POINT('Ctrl Pts',(-1.139990581936,0.723460043259,-3.820089305607));
#27292=CARTESIAN_POINT('Ctrl Pts',(-0.3868583419482,1.293566238123,-3.876964305607));
#27293=CARTESIAN_POINT('Ctrl Pts',(0.555616470709,1.230554075189,-3.933839305607));
#27294=CARTESIAN_POINT('Ctrl Pts',(1.226152364316,0.5652639823961,-3.990714305607));
#27295=CARTESIAN_POINT('Ctrl Pts',(1.296564691016,-0.3766868641562,-4.047589305607));
#27296=CARTESIAN_POINT('Ctrl Pts',(0.7323910942975,-1.134273457497,-4.104464305607));
#27297=CARTESIAN_POINT('Ctrl Pts',(-0.190241344867,-1.336705360987,-4.161339305607));
#27298=CARTESIAN_POINT('Ctrl Pts',(-1.019762749782,-0.8849050375959,-4.218214305607));
#27299=CARTESIAN_POINT('Ctrl Pts',(-1.350175170634,0.,-4.275089305607));
#27300=CARTESIAN_POINT('Ctrl Pts',(-1.019762749782,0.8849050375959,-4.331964305607));
#27301=CARTESIAN_POINT('Ctrl Pts',(-0.190241344867,1.336705360987,-4.388839305607));
#27302=CARTESIAN_POINT('Ctrl Pts',(0.7323910942975,1.134273457497,-4.445714305607));
#27303=CARTESIAN_POINT('Ctrl Pts',(1.296564691016,0.3766868641562,-4.502589305607));
#27304=CARTESIAN_POINT('Ctrl Pts',(1.226152364316,-0.5652639823961,-4.559464305607));
#27305=CARTESIAN_POINT('Ctrl Pts',(0.555616470709,-1.230554075189,-4.616339305607));
#27306=CARTESIAN_POINT('Ctrl Pts',(-0.3868583419482,-1.293566238123,-4.673214305607));
#27307=CARTESIAN_POINT('Ctrl Pts',(-1.139990581936,-0.723460043259,-4.730089305607));
#27308=CARTESIAN_POINT('Ctrl Pts',(-1.335170067905,0.2007338620856,-4.786964305607));
#27309=CARTESIAN_POINT('Ctrl Pts',(-0.8768683655278,1.026681130153,-4.843839305607));
#27310=CARTESIAN_POINT('Ctrl Pts',(0.01060315691615,1.350133991585,-4.900714305607));
#27311=CARTESIAN_POINT('Ctrl Pts',(0.892890536887,1.012779611507,-4.957589305607));
#27312=CARTESIAN_POINT('Ctrl Pts',(1.33814455045,0.1797435821333,-5.014464305607));
#27313=CARTESIAN_POINT('Ctrl Pts',(1.128537550737,-0.7413010717389,-5.071339305607));
#27314=CARTESIAN_POINT('Ctrl Pts',(0.3663010598456,-1.299393240218,-5.128214305607));
#27315=CARTESIAN_POINT('Ctrl Pts',(-0.2606752788197,-1.247804824574,-5.166130972273));
#27316=CARTESIAN_POINT('Ctrl Pts',(-0.5279823721497,-1.122019654338,-5.185089305607));
#27317=CARTESIAN_POINT('Ctrl Pts',(-0.4696881186261,0.9981380597272,-3.444135430279));
#27318=CARTESIAN_POINT('Ctrl Pts',(-0.2318942596183,1.110035356068,-3.463093763613));
#27319=CARTESIAN_POINT('Ctrl Pts',(0.3258579542137,1.155927922117,-3.501010430279));
#27320=CARTESIAN_POINT('Ctrl Pts',(1.003936318643,0.6594544137959,-3.557885430279));
#27321=CARTESIAN_POINT('Ctrl Pts',(1.190400720751,-0.1598981886148,-3.614760430279));
#27322=CARTESIAN_POINT('Ctrl Pts',(0.7943069665412,-0.9009591520544,-3.671635430279));
#27323=CARTESIAN_POINT('Ctrl Pts',(0.009432467987836,-1.201066414053,-3.728510430279));
#27324=CARTESIAN_POINT('Ctrl Pts',(-0.7800537946193,-0.9133258114035,-3.785385430279));
#27325=CARTESIAN_POINT('Ctrl Pts',(-1.187754649245,-0.1785709428966,-3.842260430279));
#27326=CARTESIAN_POINT('Ctrl Pts',(-1.014124826746,0.6435832038027,-3.899135430279));
#27327=CARTESIAN_POINT('Ctrl Pts',(-0.3441455177085,1.150744276231,-3.956010430279));
#27328=CARTESIAN_POINT('Ctrl Pts',(0.4942711510281,1.094689252768,-4.012885430279));
#27329=CARTESIAN_POINT('Ctrl Pts',(1.090773532456,0.5028534860695,-4.069760430279));
#27330=CARTESIAN_POINT('Ctrl Pts',(1.153411671532,-0.3350970673819,-4.126635430279));
#27331=CARTESIAN_POINT('Ctrl Pts',(0.6515281822355,-1.009038926982,-4.183510430279));
#27332=CARTESIAN_POINT('Ctrl Pts',(-0.169236898936,-1.189120431432,-4.240385430279));
#27333=CARTESIAN_POINT('Ctrl Pts',(-0.9071712857378,-0.7872031419892,-4.297260430279));
#27334=CARTESIAN_POINT('Ctrl Pts',(-1.201103046544,0.,-4.354135430279));
#27335=CARTESIAN_POINT('Ctrl Pts',(-0.9071712857378,0.7872031419892,-4.411010430279));
#27336=CARTESIAN_POINT('Ctrl Pts',(-0.169236898936,1.189120431432,-4.467885430279));
#27337=CARTESIAN_POINT('Ctrl Pts',(0.6515281822355,1.009038926982,-4.524760430279));
#27338=CARTESIAN_POINT('Ctrl Pts',(1.153411671532,0.3350970673819,-4.581635430279));
#27339=CARTESIAN_POINT('Ctrl Pts',(1.090773532456,-0.5028534860695,-4.638510430279));
#27340=CARTESIAN_POINT('Ctrl Pts',(0.4942711510281,-1.094689252768,-4.695385430279));
#27341=CARTESIAN_POINT('Ctrl Pts',(-0.3441455177085,-1.150744276231,-4.752260430279));
#27342=CARTESIAN_POINT('Ctrl Pts',(-1.014124826746,-0.6435832038027,-4.809135430279));
#27343=CARTESIAN_POINT('Ctrl Pts',(-1.187754649245,0.1785709428966,-4.866010430279));
#27344=CARTESIAN_POINT('Ctrl Pts',(-0.7800537946193,0.9133258114035,-4.922885430279));
#27345=CARTESIAN_POINT('Ctrl Pts',(0.009432467987837,1.201066414053,-4.979760430279));
#27346=CARTESIAN_POINT('Ctrl Pts',(0.7943069665412,0.9009591520544,-5.036635430279));
#27347=CARTESIAN_POINT('Ctrl Pts',(1.190400720751,0.1598981886148,-5.093510430279));
#27348=CARTESIAN_POINT('Ctrl Pts',(1.003936318643,-0.6594544137959,-5.150385430279));
#27349=CARTESIAN_POINT('Ctrl Pts',(0.3258579542137,-1.155927922117,-5.207260430279));
#27350=CARTESIAN_POINT('Ctrl Pts',(-0.2318942596183,-1.110035356068,-5.245177096946));
#27351=CARTESIAN_POINT('Ctrl Pts',(-0.4696881186261,-0.9981380597272,-5.264135430279));
#27352=CARTESIAN_POINT('',(-1.98293436122935E-9,-1.49923261688425,-5.00044299895813));
#27353=CARTESIAN_POINT('Ctrl Pts',(-2.06854461059408E-5,1.49901358627223,
-3.74995486355702));
#27354=CARTESIAN_POINT('Ctrl Pts',(0.0953214838108722,1.49902491199573,
-3.75491761318045));
#27355=CARTESIAN_POINT('Ctrl Pts',(0.190691030215867,1.49011947635385,-3.75989138992608));
#27356=CARTESIAN_POINT('Ctrl Pts',(0.372498933869856,1.4554667038667,-3.76973052378357));
#27357=CARTESIAN_POINT('Ctrl Pts',(0.458525227543786,1.43085386099119,-3.77459116547234));
#27358=CARTESIAN_POINT('Ctrl Pts',(0.722446426616915,1.32838383657262,-3.79004693335256));
#27359=CARTESIAN_POINT('Ctrl Pts',(0.866454933804677,1.23164641754742,-3.79893369151964));
#27360=CARTESIAN_POINT('Ctrl Pts',(1.06600265467696,1.0603973538125,-3.81260503313005));
#27361=CARTESIAN_POINT('Ctrl Pts',(1.14683835565651,0.97298033137476,-3.81875630933353));
#27362=CARTESIAN_POINT('Ctrl Pts',(1.29967423550168,0.762168700626042,-3.83268102999226));
#27363=CARTESIAN_POINT('Ctrl Pts',(1.36539620478676,0.636646697395098,-3.84046986466727));
#27364=CARTESIAN_POINT('Ctrl Pts',(1.44568091735346,0.409137312957459,-3.85325803431838));
#27365=CARTESIAN_POINT('Ctrl Pts',(1.46940771045131,0.312321550321848,-3.85841762364376));
#27366=CARTESIAN_POINT('Ctrl Pts',(1.50054215939582,0.0968012311807324,
-3.86974762234647));
#27367=CARTESIAN_POINT('Ctrl Pts',(1.50386336583334,-0.0225864242439717,
-3.87592790099484));
#27368=CARTESIAN_POINT('Ctrl Pts',(1.48028992278844,-0.279075253883447,
-3.88972651028424));
#27369=CARTESIAN_POINT('Ctrl Pts',(1.44824876150166,-0.413867874229844,
-3.89734526453951));
#27370=CARTESIAN_POINT('Ctrl Pts',(1.36138274914184,-0.635627037819925,
-3.90997498794205));
#27371=CARTESIAN_POINT('Ctrl Pts',(1.31601337842991,-0.724432162572956,
-3.91513698024775));
#27372=CARTESIAN_POINT('Ctrl Pts',(1.1985813070018,-0.907957044093197,-3.92647071223722));
#27373=CARTESIAN_POINT('Ctrl Pts',(1.12297157880747,-1.00051622230352,-3.93265174258831));
#27374=CARTESIAN_POINT('Ctrl Pts',(0.935510734630078,-1.18096930350538,
-3.94658311814019));
#27375=CARTESIAN_POINT('Ctrl Pts',(0.82085370381211,-1.26317291479204,-3.95433952071051));
#27376=CARTESIAN_POINT('Ctrl Pts',(0.607361198665975,-1.3742110709498,-3.96709317469488));
#27377=CARTESIAN_POINT('Ctrl Pts',(0.514819503017504,-1.41125178892118,
-3.97225152016788));
#27378=CARTESIAN_POINT('Ctrl Pts',(0.306211258635138,-1.47211310867903,
-3.98355595013962));
#27379=CARTESIAN_POINT('Ctrl Pts',(0.188926596878288,-1.49208312971452,
-3.98971190758976));
#27380=CARTESIAN_POINT('Ctrl Pts',(-0.0670817760633412,-1.50479893204468,
-4.00344188021202));
#27381=CARTESIAN_POINT('Ctrl Pts',(-0.204264061836427,-1.49224160547226,
-4.01101759022916));
#27382=CARTESIAN_POINT('Ctrl Pts',(-0.435383240178148,-1.43800305381015,
-4.02361014831978));
#27383=CARTESIAN_POINT('Ctrl Pts',(-0.529759724212074,-1.40572556203709,
-4.02877412817637));
#27384=CARTESIAN_POINT('Ctrl Pts',(-0.728440094304539,-1.31545684930298,
-4.04012620086496));
#27385=CARTESIAN_POINT('Ctrl Pts',(-0.831081185799221,-1.25358147405089,
-4.04632332229975));
#27386=CARTESIAN_POINT('Ctrl Pts',(-1.03747315158834,-1.09264013452199,
-4.06033406844491));
#27387=CARTESIAN_POINT('Ctrl Pts',(-1.13578892642194,-0.989806391524769,
-4.06815505599112));
#27388=CARTESIAN_POINT('Ctrl Pts',(-1.27616339680925,-0.79292350020094,
-4.08096631701665));
#27389=CARTESIAN_POINT('Ctrl Pts',(-1.32572981587319,-0.706468967379275,
-4.08612261921322));
#27390=CARTESIAN_POINT('Ctrl Pts',(-1.41494914035009,-0.508669815653088,
-4.09741077045872));
#27391=CARTESIAN_POINT('Ctrl Pts',(-1.45101571447823,-0.395608673695437,
-4.10355276851211));
#27392=CARTESIAN_POINT('Ctrl Pts',(-1.49905455000182,-0.145868247220127,
-4.11717831536221));
#27393=CARTESIAN_POINT('Ctrl Pts',(-1.50597375104998,-0.00999053376809994,
-4.12466154019219));
#27394=CARTESIAN_POINT('Ctrl Pts',(-1.48555860957934,0.224860674033037,
-4.13717178661237));
#27395=CARTESIAN_POINT('Ctrl Pts',(-1.46712396673882,0.32292021535189,-4.14233879547487));
#27396=CARTESIAN_POINT('Ctrl Pts',(-1.40609716643174,0.532947437375313,
-4.15371621536766));
#27397=CARTESIAN_POINT('Ctrl Pts',(-1.35932684529104,0.643798827202036,
-4.15993516379194));
#27398=CARTESIAN_POINT('Ctrl Pts',(-1.22813604202709,0.873215485968564,
-4.17407803827426));
#27399=CARTESIAN_POINT('Ctrl Pts',(-1.13881445511541,0.986617888170726,
-4.18201228151039));
#27400=CARTESIAN_POINT('Ctrl Pts',(-0.961751173064932,1.15426033407093,
-4.19492489192118));
#27401=CARTESIAN_POINT('Ctrl Pts',(-0.883016083174209,1.21528568040051,
-4.20007785607496));
#27402=CARTESIAN_POINT('Ctrl Pts',(-0.699907663242897,1.33073761999726,
-4.21133910588142));
#27403=CARTESIAN_POINT('Ctrl Pts',(-0.59339436076046,1.38193694102476,-4.21745797747921));
#27404=CARTESIAN_POINT('Ctrl Pts',(-0.356452332247489,1.4630284072985,-4.23088037938893));
#27405=CARTESIAN_POINT('Ctrl Pts',(-0.226267156170153,1.48861703792723,
-4.2381799877178));
#27406=CARTESIAN_POINT('Ctrl Pts',(0.00575573259620276,1.50249422398779,
-4.25052727259274));
#27407=CARTESIAN_POINT('Ctrl Pts',(0.105522727996987,1.49854594605214,-4.25570057131407));
#27408=CARTESIAN_POINT('Ctrl Pts',(0.323231911347154,1.46862568093766,-4.26713232860675));
#27409=CARTESIAN_POINT('Ctrl Pts',(0.440651133512366,1.43814338966245,-4.27339821195148));
#27410=CARTESIAN_POINT('Ctrl Pts',(0.691202779825676,1.33949753157944,-4.28779882845233));
#27411=CARTESIAN_POINT('Ctrl Pts',(0.819432220535704,1.26490268988052,-4.29594988333619));
#27412=CARTESIAN_POINT('Ctrl Pts',(1.01263927792164,1.10985318182305,-4.3090569998956));
#27413=CARTESIAN_POINT('Ctrl Pts',(1.08376671441976,1.04021565780867,-4.31420386152154));
#27414=CARTESIAN_POINT('Ctrl Pts',(1.22248539198388,0.875270661352502,-4.32541672165898));
#27415=CARTESIAN_POINT('Ctrl Pts',(1.28731113077411,0.777524084484609,-4.33149402762996));
#27416=CARTESIAN_POINT('Ctrl Pts',(1.39385162400454,0.566766273420988,-4.34415987801976));
#27417=CARTESIAN_POINT('Ctrl Pts',(1.43435322284828,0.454479793977223,-4.35073445226797));
#27418=CARTESIAN_POINT('Ctrl Pts',(1.50158127237526,0.16035036256143,-4.36683902084268));
#27419=CARTESIAN_POINT('Ctrl Pts',(1.50960418346802,-0.024600845584221,
-4.37616861592655));
#27420=CARTESIAN_POINT('Ctrl Pts',(1.45976216022343,-0.392156499866828,
-4.39565249615808));
#27421=CARTESIAN_POINT('Ctrl Pts',(1.39976156558948,-0.571423312178124,
-4.40599198974702));
#27422=CARTESIAN_POINT('Ctrl Pts',(1.2396181854439,-0.853752427360892,-4.42322630594188));
#27423=CARTESIAN_POINT('Ctrl Pts',(1.15716102195368,-0.962143722097524,
-4.43020040010785));
#27424=CARTESIAN_POINT('Ctrl Pts',(0.992056672639983,-1.12835719191808,
-4.44241776529972));
#27425=CARTESIAN_POINT('Ctrl Pts',(0.915130849967703,-1.19202945764122,
-4.44763968365768));
#27426=CARTESIAN_POINT('Ctrl Pts',(0.751015587707874,-1.30203114853202,
-4.458282264193));
#27427=CARTESIAN_POINT('Ctrl Pts',(0.664441333631893,-1.34825382205082,
-4.46368412404472));
#27428=CARTESIAN_POINT('Ctrl Pts',(0.469866631067643,-1.42827884860942,
-4.47497345546702));
#27429=CARTESIAN_POINT('Ctrl Pts',(0.361429858991136,-1.45911306466684,
-4.48082613074989));
#27430=CARTESIAN_POINT('Ctrl Pts',(0.0868762359092743,-1.50558560899775,
-4.49531699283451));
#27431=CARTESIAN_POINT('Ctrl Pts',(-0.108524317716607,-1.51122808335893,
-4.50529891944146));
#27432=CARTESIAN_POINT('Ctrl Pts',(-0.523722674797389,-1.42104336266443,
-4.52848372599792));
#27433=CARTESIAN_POINT('Ctrl Pts',(-0.694234730239479,-1.33806699523359,
-4.53820584742696));
#27434=CARTESIAN_POINT('Ctrl Pts',(-0.910861496374433,-1.19466783514413,
-4.55172096812832));
#27435=CARTESIAN_POINT('Ctrl Pts',(-0.98867136206926,-1.13146867135376,
-4.55691876600439));
#27436=CARTESIAN_POINT('Ctrl Pts',(-1.15071022637616,-0.970526548867814,
-4.56906886005236));
#27437=CARTESIAN_POINT('Ctrl Pts',(-1.22919775433432,-0.86912994570599,
-4.57612660127595));
#27438=CARTESIAN_POINT('Ctrl Pts',(-1.35102651289326,-0.66008878878192,
-4.58909822282328));
#27439=CARTESIAN_POINT('Ctrl Pts',(-1.39685081727062,-0.555601837992771,
-4.59501522777262));
#27440=CARTESIAN_POINT('Ctrl Pts',(-1.46023242591247,-0.35263118015693,
-4.60607893598703));
#27441=CARTESIAN_POINT('Ctrl Pts',(-1.48061440505115,-0.254942345678531,
-4.61123656160695));
#27442=CARTESIAN_POINT('Ctrl Pts',(-1.50710266895417,-0.00828580751651268,
-4.62435255893666));
#27443=CARTESIAN_POINT('Ctrl Pts',(-1.50081675130974,0.14007412730559,-4.63250645615578));
#27444=CARTESIAN_POINT('Ctrl Pts',(-1.44962171172692,0.400100283576456,
-4.64669155693514));
#27445=CARTESIAN_POINT('Ctrl Pts',(-1.41383856371387,0.511332352490623,
-4.65273927950174));
#27446=CARTESIAN_POINT('Ctrl Pts',(-1.32508034509336,0.707735304809056,
-4.66395129249828));
#27447=CARTESIAN_POINT('Ctrl Pts',(-1.27525799313722,0.794428647654011,
-4.66912511463795));
#27448=CARTESIAN_POINT('Ctrl Pts',(-1.13603749863021,0.989120951306691,
-4.68180966008535));
#27449=CARTESIAN_POINT('Ctrl Pts',(-1.039783729169,1.09007739184694,-4.68947685530421));
#27450=CARTESIAN_POINT('Ctrl Pts',(-0.839992920828512,1.24722356599085,
-4.70309675364886));
#27451=CARTESIAN_POINT('Ctrl Pts',(-0.742007099499302,1.30747183338976,
-4.709058034298));
#27452=CARTESIAN_POINT('Ctrl Pts',(-0.548714342600776,1.39841818027375,
-4.72017198315358));
#27453=CARTESIAN_POINT('Ctrl Pts',(-0.454659915595358,1.43197845452504,
-4.72533518699329));
#27454=CARTESIAN_POINT('Ctrl Pts',(-0.216974120292315,1.49111903235912,
-4.7382953841698));
#27455=CARTESIAN_POINT('Ctrl Pts',(-0.0724161569414992,1.50527557455243,
-4.74627396486505));
#27456=CARTESIAN_POINT('Ctrl Pts',(0.188277504903036,1.49194501788249,-4.76025172537461));
#27457=CARTESIAN_POINT('Ctrl Pts',(0.302762928080303,1.47261448509728,-4.76626424532973));
#27458=CARTESIAN_POINT('Ctrl Pts',(0.509166190956025,1.41331142809291,-4.77743639057917));
#27459=CARTESIAN_POINT('Ctrl Pts',(0.602092049133723,1.37653010345847,-4.78260599265093));
#27460=CARTESIAN_POINT('Ctrl Pts',(0.816798907969054,1.26585681257779,-4.79539924148338));
#27461=CARTESIAN_POINT('Ctrl Pts',(0.932266966022699,1.18361839847875,-4.80318933375506));
#27462=CARTESIAN_POINT('Ctrl Pts',(1.11767176119119,1.00598881419239,-4.81694380600376));
#27463=CARTESIAN_POINT('Ctrl Pts',(1.19119922319881,0.917143963828736,-4.8229188128383));
#27464=CARTESIAN_POINT('Ctrl Pts',(1.30836409219123,0.738141596019945,-4.83404861925251));
#27465=CARTESIAN_POINT('Ctrl Pts',(1.35471182572177,0.649655711812843,-4.83921376341602));
#27466=CARTESIAN_POINT('Ctrl Pts',(1.44584034292757,0.423842525840391,-4.8521023404286));
#27467=CARTESIAN_POINT('Ctrl Pts',(1.47984174077659,0.284133317597195,-4.860001653993));
#27468=CARTESIAN_POINT('Ctrl Pts',(1.50356071468381,0.0257340761359156,
-4.87390253859832));
#27469=CARTESIAN_POINT('Ctrl Pts',(1.50070694923776,-0.0902601036702479,
-4.87991376788426));
#27470=CARTESIAN_POINT('Ctrl Pts',(1.47138357560968,-0.3028900573086,-4.8910824294789));
#27471=CARTESIAN_POINT('Ctrl Pts',(1.44820663630591,-0.400068083839261,
-4.89625016146622));
#27472=CARTESIAN_POINT('Ctrl Pts',(1.36846871474656,-0.630511787660118,
-4.90916112595295));
#27473=CARTESIAN_POINT('Ctrl Pts',(1.30213290035627,-0.75843222776214,-4.91707761328718));
#27474=CARTESIAN_POINT('Ctrl Pts',(1.1501446460106,-0.968689653567613,-4.93095602028381));
#27475=CARTESIAN_POINT('Ctrl Pts',(1.07203283432548,-1.05396027144246,-4.93693871001663));
#27476=CARTESIAN_POINT('Ctrl Pts',(0.872606659872905,-1.22786655368374,
-4.95069608904956));
#27477=CARTESIAN_POINT('Ctrl Pts',(0.726903650728373,-1.32597814557149,
-4.95968126963874));
#27478=CARTESIAN_POINT('Ctrl Pts',(0.46234340839985,-1.42967442692867,-4.97519006837574));
#27479=CARTESIAN_POINT('Ctrl Pts',(0.375674252659661,-1.45470533198711,
-4.98009449424626));
#27480=CARTESIAN_POINT('Ctrl Pts',(0.192359458102347,-1.4899630079936,-4.99002156504881));
#27481=CARTESIAN_POINT('Ctrl Pts',(0.096155412570898,-1.49902501105836,
-4.99503897916822));
#27482=CARTESIAN_POINT('Ctrl Pts',(-2.06854460854666E-5,-1.49901358627223,
-5.00004513644297));
#27483=CARTESIAN_POINT('',(3.24550813202643E-10,-1.11698717744401,-5.22113249718027));
#27484=CARTESIAN_POINT('',(0.,-1.5,-5.));
#27485=CARTESIAN_POINT('Ctrl Pts',(2.02707198384535E-6,1.11628565404413,
-3.47111408882413));
#27486=CARTESIAN_POINT('Ctrl Pts',(0.0945477069597151,1.11645974724111,
-3.47785015639956));
#27487=CARTESIAN_POINT('Ctrl Pts',(0.189124507262868,1.1048491526056,-3.48459224618512));
#27488=CARTESIAN_POINT('Ctrl Pts',(0.37280187843043,1.05728988862616,-3.49813470031972));
#27489=CARTESIAN_POINT('Ctrl Pts',(0.46120374861096,1.02120417552907,-3.50489047871014));
#27490=CARTESIAN_POINT('Ctrl Pts',(0.668471432388854,0.904915646636005,
-3.52182073957925));
#27491=CARTESIAN_POINT('Ctrl Pts',(0.780383055419262,0.81102950076143,-3.53202995426488));
#27492=CARTESIAN_POINT('Ctrl Pts',(0.977352549963127,0.567498199932436,
-3.55436776308206));
#27493=CARTESIAN_POINT('Ctrl Pts',(1.03703915589555,0.431145768277802,-3.5647587800084));
#27494=CARTESIAN_POINT('Ctrl Pts',(1.11066616674449,0.178042375581387,-3.58352929238688));
#27495=CARTESIAN_POINT('Ctrl Pts',(1.1250370353998,0.0352369170927974,-3.59357133882956));
#27496=CARTESIAN_POINT('Ctrl Pts',(1.09418460733437,-0.296790717289763,
-3.61736190012804));
#27497=CARTESIAN_POINT('Ctrl Pts',(1.02997735713433,-0.440477084842063,
-3.62828381624767));
#27498=CARTESIAN_POINT('Ctrl Pts',(0.9255889082428,-0.636392952388534,-3.64408990478641));
#27499=CARTESIAN_POINT('Ctrl Pts',(0.840538191683136,-0.751460714065273,
-3.65410198836101));
#27500=CARTESIAN_POINT('Ctrl Pts',(0.61118224779972,-0.946513834085747,
-3.67558474266587));
#27501=CARTESIAN_POINT('Ctrl Pts',(0.4782345297511,-1.0191711099922,-3.68616577485579));
#27502=CARTESIAN_POINT('Ctrl Pts',(0.222597234321225,-1.1004636264182,-3.705267721173));
#27503=CARTESIAN_POINT('Ctrl Pts',(0.0794663775051739,-1.12675755955542,
-3.71543571983759));
#27504=CARTESIAN_POINT('Ctrl Pts',(-0.232981315456785,-1.10176800386664,
-3.73779253835339));
#27505=CARTESIAN_POINT('Ctrl Pts',(-0.377700605109036,-1.06037143957914,
-3.74830194335543));
#27506=CARTESIAN_POINT('Ctrl Pts',(-0.604852724324544,-0.94473173616761,
-3.76645937858707));
#27507=CARTESIAN_POINT('Ctrl Pts',(-0.731331226988469,-0.863974006299937,
-3.77692136770941));
#27508=CARTESIAN_POINT('Ctrl Pts',(-0.943397907937875,-0.61393454762197,
-3.80029160325254));
#27509=CARTESIAN_POINT('Ctrl Pts',(-1.01607631574408,-0.484189787750154,
-3.81067712497169));
#27510=CARTESIAN_POINT('Ctrl Pts',(-1.11857306467123,-0.173002860562893,
-3.83402934320733));
#27511=CARTESIAN_POINT('Ctrl Pts',(-1.1216526627367,-0.0230529286472856,
-3.84448736045733));
#27512=CARTESIAN_POINT('Ctrl Pts',(-1.10179845703877,0.228016486144775,
-3.86242927917354));
#27513=CARTESIAN_POINT('Ctrl Pts',(-1.06324590215936,0.369253565391399,
-3.87266080687385));
#27514=CARTESIAN_POINT('Ctrl Pts',(-0.924464855646186,0.649976757040046,
-3.89499359014349));
#27515=CARTESIAN_POINT('Ctrl Pts',(-0.825915661788603,0.761161572818591,
-3.90536755467241));
#27516=CARTESIAN_POINT('Ctrl Pts',(-0.626214316349842,0.934430304671211,
-3.92419538133658));
#27517=CARTESIAN_POINT('Ctrl Pts',(-0.502214996937528,1.0073238571117,-3.93425796124846));
#27518=CARTESIAN_POINT('Ctrl Pts',(-0.19120199753371,1.11682300306852,-3.95778190972181));
#27519=CARTESIAN_POINT('Ctrl Pts',(-0.0349012702549547,1.12007370080308,
-3.96864513166231));
#27520=CARTESIAN_POINT('Ctrl Pts',(0.203851405860764,1.10611718857029,-3.98567366866181));
#27521=CARTESIAN_POINT('Ctrl Pts',(0.341786112597055,1.07261170247851,-3.995614088678));
#27522=CARTESIAN_POINT('Ctrl Pts',(0.603413551668548,0.951563052462829,
-4.01618313304261));
#27523=CARTESIAN_POINT('Ctrl Pts',(0.725113385898965,0.86121167341581,-4.02676949290965));
#27524=CARTESIAN_POINT('Ctrl Pts',(0.905273423514502,0.663857977873305,
-4.04579742516296));
#27525=CARTESIAN_POINT('Ctrl Pts',(0.989304020610915,0.545163021076572,
-4.05595751403342));
#27526=CARTESIAN_POINT('Ctrl Pts',(1.09791444748827,0.250846118613153,-4.07833525890648));
#27527=CARTESIAN_POINT('Ctrl Pts',(1.12102369397598,0.101931202388067,-4.08885689635648));
#27528=CARTESIAN_POINT('Ctrl Pts',(1.11127472608703,-0.152382998726041,
-4.10698527230642));
#27529=CARTESIAN_POINT('Ctrl Pts',(1.09120934524511,-0.300938815206558,
-4.11743533545796));
#27530=CARTESIAN_POINT('Ctrl Pts',(0.953355092950169,-0.598483057720678,
-4.14081240762304));
#27531=CARTESIAN_POINT('Ctrl Pts',(0.865889506205107,-0.719096632405901,
-4.15121651825254));
#27532=CARTESIAN_POINT('Ctrl Pts',(0.630908211369321,-0.938430669099282,
-4.17412556939149));
#27533=CARTESIAN_POINT('Ctrl Pts',(0.499473987912806,-1.00559671816687,
-4.18443093822623));
#27534=CARTESIAN_POINT('Ctrl Pts',(0.254954649474644,-1.09592824110065,
-4.20300231361181));
#27535=CARTESIAN_POINT('Ctrl Pts',(0.110233508147538,-1.12012616746575,
-4.21325541986775));
#27536=CARTESIAN_POINT('Ctrl Pts',(-0.202625788977277,-1.11169037854405,
-4.23557375090056));
#27537=CARTESIAN_POINT('Ctrl Pts',(-0.344594062565005,-1.06910154094397,
-4.24592507043897));
#27538=CARTESIAN_POINT('Ctrl Pts',(-0.586363065095529,-0.95997491663841,
-4.2648152172114));
#27539=CARTESIAN_POINT('Ctrl Pts',(-0.704733656287602,-0.877644037487904,
-4.27490073023948));
#27540=CARTESIAN_POINT('Ctrl Pts',(-0.924445762809004,-0.651144082671878,
-4.29741286795022));
#27541=CARTESIAN_POINT('Ctrl Pts',(-0.995878303027182,-0.517818669122211,
-4.30795712525469));
#27542=CARTESIAN_POINT('Ctrl Pts',(-1.08982166380632,-0.277939862987314,
-4.32630001885425));
#27543=CARTESIAN_POINT('Ctrl Pts',(-1.1169872981078,-0.139044412854724,
-4.33621126978535));
#27544=CARTESIAN_POINT('Ctrl Pts',(-1.1169872981078,0.139044412854727,-4.35605370329665));
#27545=CARTESIAN_POINT('Ctrl Pts',(-1.08982166380632,0.277939862987316,
-4.36596495422619));
#27546=CARTESIAN_POINT('Ctrl Pts',(-0.995878303027179,0.517818669122219,
-4.38430784782586));
#27547=CARTESIAN_POINT('Ctrl Pts',(-0.924445762808998,0.651144082671885,
-4.39485210513048));
#27548=CARTESIAN_POINT('Ctrl Pts',(-0.704733656287599,0.877644037487907,
-4.41736424284125));
#27549=CARTESIAN_POINT('Ctrl Pts',(-0.586363065095524,0.959974916638413,
-4.42744975586925));
#27550=CARTESIAN_POINT('Ctrl Pts',(-0.344594062564994,1.06910154094398,
-4.44633990264163));
#27551=CARTESIAN_POINT('Ctrl Pts',(-0.202625788977266,1.11169037854405,
-4.45669122217995));
#27552=CARTESIAN_POINT('Ctrl Pts',(0.110233508147553,1.12012616746575,-4.47900955321285));
#27553=CARTESIAN_POINT('Ctrl Pts',(0.254954649474663,1.09592824110064,-4.48926265946891));
#27554=CARTESIAN_POINT('Ctrl Pts',(0.499473987912846,1.00559671816685,-4.50783403485462));
#27555=CARTESIAN_POINT('Ctrl Pts',(0.630908211369362,0.938430669099253,
-4.51813940368944));
#27556=CARTESIAN_POINT('Ctrl Pts',(0.865889506205137,0.719096632405866,
-4.54104845482854));
#27557=CARTESIAN_POINT('Ctrl Pts',(0.953355092950198,0.598483057720634,
-4.55145256545815));
#27558=CARTESIAN_POINT('Ctrl Pts',(1.09120934524514,0.300938815206483,-4.57482963762336));
#27559=CARTESIAN_POINT('Ctrl Pts',(1.11127472608704,0.152382998725954,-4.58527970077493));
#27560=CARTESIAN_POINT('Ctrl Pts',(1.12102369397598,-0.10193120238813,-4.60340807672478));
#27561=CARTESIAN_POINT('Ctrl Pts',(1.09791444748826,-0.250846118613211,
-4.61392971417461));
#27562=CARTESIAN_POINT('Ctrl Pts',(0.989304020610889,-0.545163021076618,
-4.63630745904754));
#27563=CARTESIAN_POINT('Ctrl Pts',(0.905273423514473,-0.663857977873342,
-4.64646754791798));
#27564=CARTESIAN_POINT('Ctrl Pts',(0.725113385898935,-0.861211673415836,
-4.66549548017135));
#27565=CARTESIAN_POINT('Ctrl Pts',(0.603413551668514,-0.951563052462852,
-4.67608184003854));
#27566=CARTESIAN_POINT('Ctrl Pts',(0.341786112597019,-1.07261170247852,
-4.69665088440312));
#27567=CARTESIAN_POINT('Ctrl Pts',(0.203851405860731,-1.1061171885703,-4.70659130441917));
#27568=CARTESIAN_POINT('Ctrl Pts',(-0.034901270254981,-1.12007370080307,
-4.72361984141848));
#27569=CARTESIAN_POINT('Ctrl Pts',(-0.191201997533732,-1.11682300306852,
-4.73448306335868));
#27570=CARTESIAN_POINT('Ctrl Pts',(-0.502214996937548,-1.00732385711169,
-4.75800701183202));
#27571=CARTESIAN_POINT('Ctrl Pts',(-0.626214316349861,-0.934430304671198,
-4.76806959174406));
#27572=CARTESIAN_POINT('Ctrl Pts',(-0.82591566178862,-0.761161572818574,
-4.78689741840843));
#27573=CARTESIAN_POINT('Ctrl Pts',(-0.924464855646204,-0.649976757040023,
-4.79727138293758));
#27574=CARTESIAN_POINT('Ctrl Pts',(-1.06324590215937,-0.369253565391362,
-4.81960416620731));
#27575=CARTESIAN_POINT('Ctrl Pts',(-1.10179845703878,-0.228016486144732,
-4.82983569390757));
#27576=CARTESIAN_POINT('Ctrl Pts',(-1.12165266273671,0.0230529286474007,
-4.84777761262373));
#27577=CARTESIAN_POINT('Ctrl Pts',(-1.11857306467121,0.173002860562986,
-4.85823562987364));
#27578=CARTESIAN_POINT('Ctrl Pts',(-1.01607631574406,0.484189787750189,
-4.88158784810919));
#27579=CARTESIAN_POINT('Ctrl Pts',(-0.943397907937854,0.613934547622001,
-4.8919733698283));
#27580=CARTESIAN_POINT('Ctrl Pts',(-0.731331226988424,0.863974006299981,
-4.91534360537137));
#27581=CARTESIAN_POINT('Ctrl Pts',(-0.604852724324483,0.944731736167644,
-4.92580559449369));
#27582=CARTESIAN_POINT('Ctrl Pts',(-0.377700605109008,1.06037143957915,
-4.9439630297253));
#27583=CARTESIAN_POINT('Ctrl Pts',(-0.232981315456755,1.10176800386665,
-4.95447243472734));
#27584=CARTESIAN_POINT('Ctrl Pts',(0.0794663775052038,1.12675755955542,
-4.97682925324312));
#27585=CARTESIAN_POINT('Ctrl Pts',(0.222597234321253,1.1004636264182,-4.98699725190771));
#27586=CARTESIAN_POINT('Ctrl Pts',(0.478234529751118,1.01917110999219,-5.00609919822493));
#27587=CARTESIAN_POINT('Ctrl Pts',(0.611182247799728,0.946513834085734,
-5.01668023041484));
#27588=CARTESIAN_POINT('Ctrl Pts',(0.840538191683134,0.751460714065251,
-5.03816298471982));
#27589=CARTESIAN_POINT('Ctrl Pts',(0.925588908242794,0.636392952388502,
-5.04817506829456));
#27590=CARTESIAN_POINT('Ctrl Pts',(1.02997735713434,0.440477084842007,-5.06398115683345));
#27591=CARTESIAN_POINT('Ctrl Pts',(1.09418460733438,0.296790717289679,-5.07490307295331));
#27592=CARTESIAN_POINT('Ctrl Pts',(1.1250370353998,-0.0352369170928775,
-5.09869363425173));
#27593=CARTESIAN_POINT('Ctrl Pts',(1.11066616674449,-0.178042375581458,
-5.10873568069418));
#27594=CARTESIAN_POINT('Ctrl Pts',(1.03703915589554,-0.431145768277862,
-5.12750619307245));
#27595=CARTESIAN_POINT('Ctrl Pts',(0.977352549963114,-0.567498199932472,
-5.13789720999855));
#27596=CARTESIAN_POINT('Ctrl Pts',(0.780383055419248,-0.811029500761452,
-5.16023501881578));
#27597=CARTESIAN_POINT('Ctrl Pts',(0.668471432388827,-0.904915646636028,
-5.17044423350158));
#27598=CARTESIAN_POINT('Ctrl Pts',(0.461203748610708,-1.02120417552921,
-5.18737449437092));
#27599=CARTESIAN_POINT('Ctrl Pts',(0.372801878429925,-1.05728988862637,
-5.19413027276147));
#27600=CARTESIAN_POINT('Ctrl Pts',(0.189124462134141,-1.10484916429063,
-5.20767273022349));
#27601=CARTESIAN_POINT('Ctrl Pts',(0.0945476136912826,-1.11645975869105,
-5.21441482333081));
#27602=CARTESIAN_POINT('Ctrl Pts',(1.88721575241811E-6,-1.11628565378659,
-5.22115089422152));
#27603=CARTESIAN_POINT('Ctrl Pts',(-0.4755900604755,1.010680324589,-3.420126599063));
#27604=CARTESIAN_POINT('Ctrl Pts',(-0.2348081643589,1.123983684464,-3.439084932396));
#27605=CARTESIAN_POINT('Ctrl Pts',(0.329952574922,1.170452920957,-3.477001599063));
#27606=CARTESIAN_POINT('Ctrl Pts',(1.016551442463,0.6677408946504,-3.533876599063));
#27607=CARTESIAN_POINT('Ctrl Pts',(1.205358893105,-0.1619074151071,-3.590751599063));
#27608=CARTESIAN_POINT('Ctrl Pts',(0.8042879589087,-0.9122802996697,-3.647626599063));
#27609=CARTESIAN_POINT('Ctrl Pts',(0.009550993186479,-1.216158607898,-3.704501599063));
#27610=CARTESIAN_POINT('Ctrl Pts',(-0.7898556864549,-0.9248023542725,-3.761376599063));
#27611=CARTESIAN_POINT('Ctrl Pts',(-1.202679571961,-0.180814804896,-3.818251599063));
#27612=CARTESIAN_POINT('Ctrl Pts',(-1.026867975908,0.6516702524068,-3.875126599063));
#27613=CARTESIAN_POINT('Ctrl Pts',(-0.348469933747,1.165204139133,-3.932001599063));
#27614=CARTESIAN_POINT('Ctrl Pts',(0.5004819949382,1.108444747226,-3.988876599063));
#27615=CARTESIAN_POINT('Ctrl Pts',(1.104479823299,0.5091721726955,-4.045751599063));
#27616=CARTESIAN_POINT('Ctrl Pts',(1.167905052019,-0.3393077836576,-4.102626599063));
#27617=CARTESIAN_POINT('Ctrl Pts',(0.6597150647482,-1.02171816845,-4.159501599063));
#27618=CARTESIAN_POINT('Ctrl Pts',(-0.1713634724997,-1.204062516105,-4.216376599063));
#27619=CARTESIAN_POINT('Ctrl Pts',(-0.9185704929214,-0.7970948701029,-4.273251599063));
#27620=CARTESIAN_POINT('Ctrl Pts',(-1.216195700701,0.,-4.330126599063));
#27621=CARTESIAN_POINT('Ctrl Pts',(-0.9185704929214,0.7970948701029,-4.387001599063));
#27622=CARTESIAN_POINT('Ctrl Pts',(-0.1713634724997,1.204062516105,-4.443876599063));
#27623=CARTESIAN_POINT('Ctrl Pts',(0.6597150647482,1.02171816845,-4.500751599063));
#27624=CARTESIAN_POINT('Ctrl Pts',(1.167905052019,0.3393077836576,-4.557626599063));
#27625=CARTESIAN_POINT('Ctrl Pts',(1.104479823299,-0.5091721726955,-4.614501599063));
#27626=CARTESIAN_POINT('Ctrl Pts',(0.5004819949382,-1.108444747226,-4.671376599063));
#27627=CARTESIAN_POINT('Ctrl Pts',(-0.348469933747,-1.165204139133,-4.728251599063));
#27628=CARTESIAN_POINT('Ctrl Pts',(-1.026867975908,-0.6516702524068,-4.785126599063));
#27629=CARTESIAN_POINT('Ctrl Pts',(-1.202679571961,0.180814804896,-4.842001599063));
#27630=CARTESIAN_POINT('Ctrl Pts',(-0.7898556864549,0.9248023542725,-4.898876599063));
#27631=CARTESIAN_POINT('Ctrl Pts',(0.00955099318648,1.216158607898,-4.955751599063));
#27632=CARTESIAN_POINT('Ctrl Pts',(0.8042879589087,0.9122802996697,-5.012626599063));
#27633=CARTESIAN_POINT('Ctrl Pts',(1.205358893105,0.161907415107,-5.069501599063));
#27634=CARTESIAN_POINT('Ctrl Pts',(1.016551442463,-0.6677408946504,-5.126376599063));
#27635=CARTESIAN_POINT('Ctrl Pts',(0.329952574922,-1.170452920957,-5.183251599063));
#27636=CARTESIAN_POINT('Ctrl Pts',(-0.2348081643589,-1.123983684464,-5.22116826573));
#27637=CARTESIAN_POINT('Ctrl Pts',(-0.4755900604755,-1.010680324589,-5.240126599063));
#27638=CARTESIAN_POINT('Ctrl Pts',(-0.4755900604755,1.010680324589,-3.450042199688));
#27639=CARTESIAN_POINT('Ctrl Pts',(-0.2348081643589,1.123983684464,-3.469000533021));
#27640=CARTESIAN_POINT('Ctrl Pts',(0.329952574922,1.170452920957,-3.506917199688));
#27641=CARTESIAN_POINT('Ctrl Pts',(1.016551442463,0.6677408946504,-3.563792199688));
#27642=CARTESIAN_POINT('Ctrl Pts',(1.205358893105,-0.1619074151071,-3.620667199688));
#27643=CARTESIAN_POINT('Ctrl Pts',(0.8042879589087,-0.9122802996697,-3.677542199688));
#27644=CARTESIAN_POINT('Ctrl Pts',(0.009550993186479,-1.216158607898,-3.734417199688));
#27645=CARTESIAN_POINT('Ctrl Pts',(-0.7898556864549,-0.9248023542725,-3.791292199688));
#27646=CARTESIAN_POINT('Ctrl Pts',(-1.202679571961,-0.180814804896,-3.848167199688));
#27647=CARTESIAN_POINT('Ctrl Pts',(-1.026867975908,0.6516702524068,-3.905042199688));
#27648=CARTESIAN_POINT('Ctrl Pts',(-0.348469933747,1.165204139133,-3.961917199688));
#27649=CARTESIAN_POINT('Ctrl Pts',(0.5004819949382,1.108444747226,-4.018792199688));
#27650=CARTESIAN_POINT('Ctrl Pts',(1.104479823299,0.5091721726955,-4.075667199688));
#27651=CARTESIAN_POINT('Ctrl Pts',(1.167905052019,-0.3393077836576,-4.132542199688));
#27652=CARTESIAN_POINT('Ctrl Pts',(0.6597150647482,-1.02171816845,-4.189417199688));
#27653=CARTESIAN_POINT('Ctrl Pts',(-0.1713634724997,-1.204062516105,-4.246292199688));
#27654=CARTESIAN_POINT('Ctrl Pts',(-0.9185704929214,-0.7970948701029,-4.303167199688));
#27655=CARTESIAN_POINT('Ctrl Pts',(-1.216195700701,0.,-4.360042199688));
#27656=CARTESIAN_POINT('Ctrl Pts',(-0.9185704929214,0.7970948701029,-4.416917199688));
#27657=CARTESIAN_POINT('Ctrl Pts',(-0.1713634724997,1.204062516105,-4.473792199688));
#27658=CARTESIAN_POINT('Ctrl Pts',(0.6597150647482,1.02171816845,-4.530667199688));
#27659=CARTESIAN_POINT('Ctrl Pts',(1.167905052019,0.3393077836576,-4.587542199688));
#27660=CARTESIAN_POINT('Ctrl Pts',(1.104479823299,-0.5091721726955,-4.644417199688));
#27661=CARTESIAN_POINT('Ctrl Pts',(0.5004819949382,-1.108444747226,-4.701292199688));
#27662=CARTESIAN_POINT('Ctrl Pts',(-0.348469933747,-1.165204139133,-4.758167199688));
#27663=CARTESIAN_POINT('Ctrl Pts',(-1.026867975908,-0.6516702524068,-4.815042199688));
#27664=CARTESIAN_POINT('Ctrl Pts',(-1.202679571961,0.180814804896,-4.871917199688));
#27665=CARTESIAN_POINT('Ctrl Pts',(-0.7898556864549,0.9248023542725,-4.928792199688));
#27666=CARTESIAN_POINT('Ctrl Pts',(0.00955099318648,1.216158607898,-4.985667199688));
#27667=CARTESIAN_POINT('Ctrl Pts',(0.8042879589087,0.9122802996697,-5.042542199688));
#27668=CARTESIAN_POINT('Ctrl Pts',(1.205358893105,0.161907415107,-5.099417199688));
#27669=CARTESIAN_POINT('Ctrl Pts',(1.016551442463,-0.6677408946504,-5.156292199688));
#27670=CARTESIAN_POINT('Ctrl Pts',(0.329952574922,-1.170452920957,-5.213167199688));
#27671=CARTESIAN_POINT('Ctrl Pts',(-0.2348081643589,-1.123983684464,-5.251083866354));
#27672=CARTESIAN_POINT('Ctrl Pts',(-0.4755900604755,-1.010680324589,-5.270042199688));
#27673=CARTESIAN_POINT('Ctrl Pts',(-0.4755900604755,1.010680324589,-3.479957800312));
#27674=CARTESIAN_POINT('Ctrl Pts',(-0.2348081643589,1.123983684464,-3.498916133646));
#27675=CARTESIAN_POINT('Ctrl Pts',(0.329952574922,1.170452920957,-3.536832800312));
#27676=CARTESIAN_POINT('Ctrl Pts',(1.016551442463,0.6677408946504,-3.593707800312));
#27677=CARTESIAN_POINT('Ctrl Pts',(1.205358893105,-0.1619074151071,-3.650582800312));
#27678=CARTESIAN_POINT('Ctrl Pts',(0.8042879589087,-0.9122802996697,-3.707457800312));
#27679=CARTESIAN_POINT('Ctrl Pts',(0.009550993186479,-1.216158607898,-3.764332800312));
#27680=CARTESIAN_POINT('Ctrl Pts',(-0.7898556864549,-0.9248023542725,-3.821207800312));
#27681=CARTESIAN_POINT('Ctrl Pts',(-1.202679571961,-0.180814804896,-3.878082800312));
#27682=CARTESIAN_POINT('Ctrl Pts',(-1.026867975908,0.6516702524068,-3.934957800312));
#27683=CARTESIAN_POINT('Ctrl Pts',(-0.348469933747,1.165204139133,-3.991832800312));
#27684=CARTESIAN_POINT('Ctrl Pts',(0.5004819949382,1.108444747226,-4.048707800312));
#27685=CARTESIAN_POINT('Ctrl Pts',(1.104479823299,0.5091721726955,-4.105582800312));
#27686=CARTESIAN_POINT('Ctrl Pts',(1.167905052019,-0.3393077836576,-4.162457800312));
#27687=CARTESIAN_POINT('Ctrl Pts',(0.6597150647482,-1.02171816845,-4.219332800312));
#27688=CARTESIAN_POINT('Ctrl Pts',(-0.1713634724997,-1.204062516105,-4.276207800312));
#27689=CARTESIAN_POINT('Ctrl Pts',(-0.9185704929214,-0.7970948701029,-4.333082800312));
#27690=CARTESIAN_POINT('Ctrl Pts',(-1.216195700701,0.,-4.389957800312));
#27691=CARTESIAN_POINT('Ctrl Pts',(-0.9185704929214,0.7970948701029,-4.446832800312));
#27692=CARTESIAN_POINT('Ctrl Pts',(-0.1713634724997,1.204062516105,-4.503707800312));
#27693=CARTESIAN_POINT('Ctrl Pts',(0.6597150647482,1.02171816845,-4.560582800312));
#27694=CARTESIAN_POINT('Ctrl Pts',(1.167905052019,0.3393077836576,-4.617457800312));
#27695=CARTESIAN_POINT('Ctrl Pts',(1.104479823299,-0.5091721726955,-4.674332800312));
#27696=CARTESIAN_POINT('Ctrl Pts',(0.5004819949382,-1.108444747226,-4.731207800312));
#27697=CARTESIAN_POINT('Ctrl Pts',(-0.348469933747,-1.165204139133,-4.788082800312));
#27698=CARTESIAN_POINT('Ctrl Pts',(-1.026867975908,-0.6516702524068,-4.844957800312));
#27699=CARTESIAN_POINT('Ctrl Pts',(-1.202679571961,0.180814804896,-4.901832800312));
#27700=CARTESIAN_POINT('Ctrl Pts',(-0.7898556864549,0.9248023542725,-4.958707800312));
#27701=CARTESIAN_POINT('Ctrl Pts',(0.00955099318648,1.216158607898,-5.015582800312));
#27702=CARTESIAN_POINT('Ctrl Pts',(0.8042879589087,0.9122802996697,-5.072457800312));
#27703=CARTESIAN_POINT('Ctrl Pts',(1.205358893105,0.161907415107,-5.129332800312));
#27704=CARTESIAN_POINT('Ctrl Pts',(1.016551442463,-0.6677408946504,-5.186207800312));
#27705=CARTESIAN_POINT('Ctrl Pts',(0.329952574922,-1.170452920957,-5.243082800312));
#27706=CARTESIAN_POINT('Ctrl Pts',(-0.2348081643589,-1.123983684464,-5.280999466979));
#27707=CARTESIAN_POINT('Ctrl Pts',(-0.4755900604755,-1.010680324589,-5.299957800312));
#27708=CARTESIAN_POINT('Ctrl Pts',(-0.4755900604755,1.010680324589,-3.509873400937));
#27709=CARTESIAN_POINT('Ctrl Pts',(-0.2348081643589,1.123983684464,-3.52883173427));
#27710=CARTESIAN_POINT('Ctrl Pts',(0.329952574922,1.170452920957,-3.566748400937));
#27711=CARTESIAN_POINT('Ctrl Pts',(1.016551442463,0.6677408946504,-3.623623400937));
#27712=CARTESIAN_POINT('Ctrl Pts',(1.205358893105,-0.1619074151071,-3.680498400937));
#27713=CARTESIAN_POINT('Ctrl Pts',(0.8042879589087,-0.9122802996697,-3.737373400937));
#27714=CARTESIAN_POINT('Ctrl Pts',(0.009550993186479,-1.216158607898,-3.794248400937));
#27715=CARTESIAN_POINT('Ctrl Pts',(-0.7898556864549,-0.9248023542725,-3.851123400937));
#27716=CARTESIAN_POINT('Ctrl Pts',(-1.202679571961,-0.180814804896,-3.907998400937));
#27717=CARTESIAN_POINT('Ctrl Pts',(-1.026867975908,0.6516702524068,-3.964873400937));
#27718=CARTESIAN_POINT('Ctrl Pts',(-0.348469933747,1.165204139133,-4.021748400937));
#27719=CARTESIAN_POINT('Ctrl Pts',(0.5004819949382,1.108444747226,-4.078623400937));
#27720=CARTESIAN_POINT('Ctrl Pts',(1.104479823299,0.5091721726955,-4.135498400937));
#27721=CARTESIAN_POINT('Ctrl Pts',(1.167905052019,-0.3393077836576,-4.192373400937));
#27722=CARTESIAN_POINT('Ctrl Pts',(0.6597150647482,-1.02171816845,-4.249248400937));
#27723=CARTESIAN_POINT('Ctrl Pts',(-0.1713634724997,-1.204062516105,-4.306123400937));
#27724=CARTESIAN_POINT('Ctrl Pts',(-0.9185704929214,-0.7970948701029,-4.362998400937));
#27725=CARTESIAN_POINT('Ctrl Pts',(-1.216195700701,0.,-4.419873400937));
#27726=CARTESIAN_POINT('Ctrl Pts',(-0.9185704929214,0.7970948701029,-4.476748400937));
#27727=CARTESIAN_POINT('Ctrl Pts',(-0.1713634724997,1.204062516105,-4.533623400937));
#27728=CARTESIAN_POINT('Ctrl Pts',(0.6597150647482,1.02171816845,-4.590498400937));
#27729=CARTESIAN_POINT('Ctrl Pts',(1.167905052019,0.3393077836576,-4.647373400937));
#27730=CARTESIAN_POINT('Ctrl Pts',(1.104479823299,-0.5091721726955,-4.704248400937));
#27731=CARTESIAN_POINT('Ctrl Pts',(0.5004819949382,-1.108444747226,-4.761123400937));
#27732=CARTESIAN_POINT('Ctrl Pts',(-0.348469933747,-1.165204139133,-4.817998400937));
#27733=CARTESIAN_POINT('Ctrl Pts',(-1.026867975908,-0.6516702524068,-4.874873400937));
#27734=CARTESIAN_POINT('Ctrl Pts',(-1.202679571961,0.180814804896,-4.931748400937));
#27735=CARTESIAN_POINT('Ctrl Pts',(-0.7898556864549,0.9248023542725,-4.988623400937));
#27736=CARTESIAN_POINT('Ctrl Pts',(0.00955099318648,1.216158607898,-5.045498400937));
#27737=CARTESIAN_POINT('Ctrl Pts',(0.8042879589087,0.9122802996697,-5.102373400937));
#27738=CARTESIAN_POINT('Ctrl Pts',(1.205358893105,0.161907415107,-5.159248400937));
#27739=CARTESIAN_POINT('Ctrl Pts',(1.016551442463,-0.6677408946504,-5.216123400937));
#27740=CARTESIAN_POINT('Ctrl Pts',(0.329952574922,-1.170452920957,-5.272998400937));
#27741=CARTESIAN_POINT('Ctrl Pts',(-0.2348081643589,-1.123983684464,-5.310915067604));
#27742=CARTESIAN_POINT('Ctrl Pts',(-0.4755900604755,-1.010680324589,-5.329873400937));
#27743=CARTESIAN_POINT('',(3.48982018972651E-10,-1.11698717731251,-5.27886751164369));
#27744=CARTESIAN_POINT('',(0.,-1.116987298108,-5.221132486541));
#27745=CARTESIAN_POINT('Ctrl Pts',(1.88721574551803E-6,1.11628565378659,
-3.52884910577848));
#27746=CARTESIAN_POINT('Ctrl Pts',(0.094547613691279,1.11645975869105,-3.53558517666919));
#27747=CARTESIAN_POINT('Ctrl Pts',(0.189124462134141,1.10484916429063,-3.5423272697765));
#27748=CARTESIAN_POINT('Ctrl Pts',(0.372801878429929,1.05728988862636,-3.55586972723853));
#27749=CARTESIAN_POINT('Ctrl Pts',(0.461203748610714,1.0212041755292,-3.56262550562908));
#27750=CARTESIAN_POINT('Ctrl Pts',(0.668471432388828,0.904915646636025,
-3.57955576649842));
#27751=CARTESIAN_POINT('Ctrl Pts',(0.780383055419241,0.811029500761451,
-3.58976498118421));
#27752=CARTESIAN_POINT('Ctrl Pts',(0.97735254996311,0.567498199932464,-3.61210279000144));
#27753=CARTESIAN_POINT('Ctrl Pts',(1.03703915589554,0.431145768277837,-3.62249380692754));
#27754=CARTESIAN_POINT('Ctrl Pts',(1.11066616674449,0.17804237558142,-3.64126431930581));
#27755=CARTESIAN_POINT('Ctrl Pts',(1.1250370353998,0.0352369170928312,-3.65130636574828));
#27756=CARTESIAN_POINT('Ctrl Pts',(1.09418460733438,-0.296790717289799,
-3.67509692704671));
#27757=CARTESIAN_POINT('Ctrl Pts',(1.02997735713431,-0.440477084842101,
-3.68601884316657));
#27758=CARTESIAN_POINT('Ctrl Pts',(0.925588908242806,-0.636392952388531,
-3.70182493170545));
#27759=CARTESIAN_POINT('Ctrl Pts',(0.840538191683137,-0.751460714065268,
-3.71183701528019));
#27760=CARTESIAN_POINT('Ctrl Pts',(0.61118224779974,-0.946513834085734,
-3.73331976958516));
#27761=CARTESIAN_POINT('Ctrl Pts',(0.478234529751121,-1.0191711099922,-3.74390080177506));
#27762=CARTESIAN_POINT('Ctrl Pts',(0.222597234321247,-1.1004636264182,-3.76300274809229));
#27763=CARTESIAN_POINT('Ctrl Pts',(0.0794663775051982,-1.12675755955542,
-3.77317074675688));
#27764=CARTESIAN_POINT('Ctrl Pts',(-0.232981315456759,-1.10176800386665,
-3.79552756527266));
#27765=CARTESIAN_POINT('Ctrl Pts',(-0.377700605109011,-1.06037143957915,
-3.8060369702747));
#27766=CARTESIAN_POINT('Ctrl Pts',(-0.604852724324492,-0.94473173616764,
-3.82419440550631));
#27767=CARTESIAN_POINT('Ctrl Pts',(-0.731331226988429,-0.863974006299976,
-3.83465639462863));
#27768=CARTESIAN_POINT('Ctrl Pts',(-0.943397907937854,-0.613934547622002,
-3.8580266301717));
#27769=CARTESIAN_POINT('Ctrl Pts',(-1.01607631574406,-0.484189787750189,
-3.86841215189081));
#27770=CARTESIAN_POINT('Ctrl Pts',(-1.11857306467121,-0.173002860562982,
-3.89176437012636));
#27771=CARTESIAN_POINT('Ctrl Pts',(-1.12165266273671,-0.0230529286473959,
-3.90222238737627));
#27772=CARTESIAN_POINT('Ctrl Pts',(-1.10179845703878,0.228016486144733,
-3.92016430609243));
#27773=CARTESIAN_POINT('Ctrl Pts',(-1.06324590215937,0.369253565391362,
-3.93039583379269));
#27774=CARTESIAN_POINT('Ctrl Pts',(-0.924464855646203,0.649976757040024,
-3.95272861706242));
#27775=CARTESIAN_POINT('Ctrl Pts',(-0.825915661788619,0.761161572818574,
-3.96310258159157));
#27776=CARTESIAN_POINT('Ctrl Pts',(-0.626214316349861,0.934430304671198,
-3.98193040825594));
#27777=CARTESIAN_POINT('Ctrl Pts',(-0.502214996937548,1.00732385711169,
-3.99199298816798));
#27778=CARTESIAN_POINT('Ctrl Pts',(-0.191201997533737,1.11682300306852,
-4.01551693664132));
#27779=CARTESIAN_POINT('Ctrl Pts',(-0.0349012702549876,1.12007370080308,
-4.02638015858152));
#27780=CARTESIAN_POINT('Ctrl Pts',(0.203851405860731,1.1061171885703,-4.04340869558083));
#27781=CARTESIAN_POINT('Ctrl Pts',(0.34178611259702,1.07261170247852,-4.05334911559688));
#27782=CARTESIAN_POINT('Ctrl Pts',(0.603413551668515,0.951563052462852,
-4.07391815996146));
#27783=CARTESIAN_POINT('Ctrl Pts',(0.725113385898937,0.861211673415834,
-4.08450451982865));
#27784=CARTESIAN_POINT('Ctrl Pts',(0.905273423514475,0.663857977873339,
-4.10353245208202));
#27785=CARTESIAN_POINT('Ctrl Pts',(0.989304020610891,0.545163021076615,
-4.11369254095246));
#27786=CARTESIAN_POINT('Ctrl Pts',(1.09791444748826,0.250846118613209,-4.13607028582539));
#27787=CARTESIAN_POINT('Ctrl Pts',(1.12102369397598,0.101931202388127,-4.14659192327522));
#27788=CARTESIAN_POINT('Ctrl Pts',(1.11127472608704,-0.152382998725977,
-4.16472029922507));
#27789=CARTESIAN_POINT('Ctrl Pts',(1.09120934524513,-0.3009388152065,-4.17517036237664));
#27790=CARTESIAN_POINT('Ctrl Pts',(0.953355092950196,-0.598483057720636,
-4.19854743454185));
#27791=CARTESIAN_POINT('Ctrl Pts',(0.865889506205136,-0.719096632405867,
-4.20895154517146));
#27792=CARTESIAN_POINT('Ctrl Pts',(0.630908211369377,-0.938430669099238,
-4.23186059631055));
#27793=CARTESIAN_POINT('Ctrl Pts',(0.499473987912868,-1.00559671816684,
-4.24216596514538));
#27794=CARTESIAN_POINT('Ctrl Pts',(0.254954649474665,-1.09592824110064,
-4.26073734053109));
#27795=CARTESIAN_POINT('Ctrl Pts',(0.110233508147556,-1.12012616746575,
-4.27099044678715));
#27796=CARTESIAN_POINT('Ctrl Pts',(-0.202625788977262,-1.11169037854405,
-4.29330877782005));
#27797=CARTESIAN_POINT('Ctrl Pts',(-0.34459406256499,-1.06910154094398,
-4.30366009735837));
#27798=CARTESIAN_POINT('Ctrl Pts',(-0.586363065095521,-0.959974916638415,
-4.32255024413075));
#27799=CARTESIAN_POINT('Ctrl Pts',(-0.704733656287596,-0.877644037487909,
-4.33263575715875));
#27800=CARTESIAN_POINT('Ctrl Pts',(-0.924445762808999,-0.651144082671885,
-4.35514789486952));
#27801=CARTESIAN_POINT('Ctrl Pts',(-0.99587830302718,-0.517818669122217,
-4.36569215217414));
#27802=CARTESIAN_POINT('Ctrl Pts',(-1.08982166380632,-0.277939862987316,
-4.38403504577381));
#27803=CARTESIAN_POINT('Ctrl Pts',(-1.1169872981078,-0.139044412854727,
-4.39394629670335));
#27804=CARTESIAN_POINT('Ctrl Pts',(-1.1169872981078,0.139044412854725,-4.41378873021465));
#27805=CARTESIAN_POINT('Ctrl Pts',(-1.08982166380632,0.277939862987314,
-4.42369998114575));
#27806=CARTESIAN_POINT('Ctrl Pts',(-0.995878303027181,0.517818669122213,
-4.44204287474531));
#27807=CARTESIAN_POINT('Ctrl Pts',(-0.924445762809003,0.651144082671879,
-4.45258713204978));
#27808=CARTESIAN_POINT('Ctrl Pts',(-0.704733656287605,0.877644037487902,
-4.47509926976052));
#27809=CARTESIAN_POINT('Ctrl Pts',(-0.586363065095532,0.959974916638408,
-4.4851847827886));
#27810=CARTESIAN_POINT('Ctrl Pts',(-0.344594062565008,1.06910154094397,
-4.50407492956103));
#27811=CARTESIAN_POINT('Ctrl Pts',(-0.202625788977281,1.11169037854405,
-4.51442624909944));
#27812=CARTESIAN_POINT('Ctrl Pts',(0.110233508147534,1.12012616746575,-4.53674458013225));
#27813=CARTESIAN_POINT('Ctrl Pts',(0.254954649474639,1.09592824110065,-4.54699768638819));
#27814=CARTESIAN_POINT('Ctrl Pts',(0.499473987912787,1.00559671816687,-4.56556906177377));
#27815=CARTESIAN_POINT('Ctrl Pts',(0.630908211369306,0.938430669099295,
-4.57587443060851));
#27816=CARTESIAN_POINT('Ctrl Pts',(0.865889506205103,0.719096632405906,
-4.59878348174746));
#27817=CARTESIAN_POINT('Ctrl Pts',(0.953355092950165,0.598483057720684,
-4.60918759237697));
#27818=CARTESIAN_POINT('Ctrl Pts',(1.09120934524511,0.300938815206566,-4.63256466454204));
#27819=CARTESIAN_POINT('Ctrl Pts',(1.11127472608703,0.15238299872605,-4.64301472769358));
#27820=CARTESIAN_POINT('Ctrl Pts',(1.12102369397598,-0.101931202388062,
-4.66114310364352));
#27821=CARTESIAN_POINT('Ctrl Pts',(1.09791444748828,-0.250846118613148,
-4.67166474109352));
#27822=CARTESIAN_POINT('Ctrl Pts',(0.989304020610918,-0.545163021076567,
-4.69404248596659));
#27823=CARTESIAN_POINT('Ctrl Pts',(0.905273423514505,-0.663857977873301,
-4.70420257483704));
#27824=CARTESIAN_POINT('Ctrl Pts',(0.725113385898968,-0.861211673415808,
-4.72323050709035));
#27825=CARTESIAN_POINT('Ctrl Pts',(0.603413551668551,-0.951563052462828,
-4.73381686695739));
#27826=CARTESIAN_POINT('Ctrl Pts',(0.341786112597057,-1.07261170247851,
-4.754385911322));
#27827=CARTESIAN_POINT('Ctrl Pts',(0.203851405860766,-1.10611718857029,
-4.76432633133819));
#27828=CARTESIAN_POINT('Ctrl Pts',(-0.0349012702549451,-1.12007370080308,
-4.78135486833769));
#27829=CARTESIAN_POINT('Ctrl Pts',(-0.191201997533703,-1.11682300306853,
-4.79221809027819));
#27830=CARTESIAN_POINT('Ctrl Pts',(-0.502214996937524,-1.0073238571117,
-4.81574203875154));
#27831=CARTESIAN_POINT('Ctrl Pts',(-0.626214316349838,-0.934430304671214,
-4.82580461866342));
#27832=CARTESIAN_POINT('Ctrl Pts',(-0.825915661788601,-0.761161572818594,
-4.84463244532759));
#27833=CARTESIAN_POINT('Ctrl Pts',(-0.924464855646184,-0.64997675704005,
-4.85500640985651));
#27834=CARTESIAN_POINT('Ctrl Pts',(-1.06324590215936,-0.369253565391402,
-4.87733919312616));
#27835=CARTESIAN_POINT('Ctrl Pts',(-1.10179845703877,-0.228016486144777,
-4.88757072082646));
#27836=CARTESIAN_POINT('Ctrl Pts',(-1.1216526627367,0.023052928647293,-4.90551263954267));
#27837=CARTESIAN_POINT('Ctrl Pts',(-1.11857306467123,0.173002860562897,
-4.91597065679267));
#27838=CARTESIAN_POINT('Ctrl Pts',(-1.01607631574408,0.484189787750149,
-4.93932287502831));
#27839=CARTESIAN_POINT('Ctrl Pts',(-0.943397907937877,0.613934547621966,
-4.94970839674746));
#27840=CARTESIAN_POINT('Ctrl Pts',(-0.73133122698847,0.863974006299937,
-4.97307863229059));
#27841=CARTESIAN_POINT('Ctrl Pts',(-0.604852724324544,0.94473173616761,
-4.98354062141293));
#27842=CARTESIAN_POINT('Ctrl Pts',(-0.377700605109039,1.06037143957914,
-5.00169805664457));
#27843=CARTESIAN_POINT('Ctrl Pts',(-0.232981315456788,1.10176800386664,
-5.01220746164662));
#27844=CARTESIAN_POINT('Ctrl Pts',(0.0794663775051714,1.12675755955542,
-5.03456428016241));
#27845=CARTESIAN_POINT('Ctrl Pts',(0.222597234321221,1.1004636264182,-5.044732278827));
#27846=CARTESIAN_POINT('Ctrl Pts',(0.478234529751088,1.01917110999221,-5.06383422514421));
#27847=CARTESIAN_POINT('Ctrl Pts',(0.6111822477997,0.946513834085752,-5.07441525733413));
#27848=CARTESIAN_POINT('Ctrl Pts',(0.84053819168314,0.751460714065252,-5.09589801163899));
#27849=CARTESIAN_POINT('Ctrl Pts',(0.925588908242792,0.636392952388495,
-5.10591009521358));
#27850=CARTESIAN_POINT('Ctrl Pts',(1.02997735713436,0.440477084841974,-5.12171618375232));
#27851=CARTESIAN_POINT('Ctrl Pts',(1.09418460733437,0.296790717289649,-5.13263809987195));
#27852=CARTESIAN_POINT('Ctrl Pts',(1.1250370353998,-0.0352369170928343,
-5.15642866117045));
#27853=CARTESIAN_POINT('Ctrl Pts',(1.1106661667445,-0.178042375581416,-5.16647070761313));
#27854=CARTESIAN_POINT('Ctrl Pts',(1.03703915589556,-0.43114576827782,-5.18524121999161));
#27855=CARTESIAN_POINT('Ctrl Pts',(0.977352549963136,-0.567498199932438,
-5.19563223691795));
#27856=CARTESIAN_POINT('Ctrl Pts',(0.780383055419275,-0.811029500761424,
-5.21797004573512));
#27857=CARTESIAN_POINT('Ctrl Pts',(0.668471432388861,-0.904915646636002,
-5.22817926042075));
#27858=CARTESIAN_POINT('Ctrl Pts',(0.461203748610963,-1.02120417552907,
-5.24510952128986));
#27859=CARTESIAN_POINT('Ctrl Pts',(0.372801878430432,-1.05728988862616,
-5.25186529968028));
#27860=CARTESIAN_POINT('Ctrl Pts',(0.189124507262871,-1.1048491526056,-5.26540775381488));
#27861=CARTESIAN_POINT('Ctrl Pts',(0.094547706959721,-1.11645974724111,
-5.27214984360044));
#27862=CARTESIAN_POINT('Ctrl Pts',(2.02707199375124E-6,-1.11628565404413,
-5.27888591117587));
#27863=CARTESIAN_POINT('Ctrl Pts',(-0.4696881186261,0.9981380597272,-3.485864569721));
#27864=CARTESIAN_POINT('Ctrl Pts',(-0.2318942596183,1.110035356068,-3.504822903054));
#27865=CARTESIAN_POINT('Ctrl Pts',(0.3258579542137,1.155927922117,-3.542739569721));
#27866=CARTESIAN_POINT('Ctrl Pts',(1.003936318643,0.6594544137959,-3.599614569721));
#27867=CARTESIAN_POINT('Ctrl Pts',(1.190400720751,-0.1598981886148,-3.656489569721));
#27868=CARTESIAN_POINT('Ctrl Pts',(0.7943069665412,-0.9009591520544,-3.713364569721));
#27869=CARTESIAN_POINT('Ctrl Pts',(0.009432467987835,-1.201066414053,-3.770239569721));
#27870=CARTESIAN_POINT('Ctrl Pts',(-0.7800537946193,-0.9133258114035,-3.827114569721));
#27871=CARTESIAN_POINT('Ctrl Pts',(-1.187754649245,-0.1785709428966,-3.883989569721));
#27872=CARTESIAN_POINT('Ctrl Pts',(-1.014124826746,0.6435832038027,-3.940864569721));
#27873=CARTESIAN_POINT('Ctrl Pts',(-0.3441455177085,1.150744276231,-3.997739569721));
#27874=CARTESIAN_POINT('Ctrl Pts',(0.4942711510281,1.094689252768,-4.054614569721));
#27875=CARTESIAN_POINT('Ctrl Pts',(1.090773532456,0.5028534860695,-4.111489569721));
#27876=CARTESIAN_POINT('Ctrl Pts',(1.153411671532,-0.3350970673819,-4.168364569721));
#27877=CARTESIAN_POINT('Ctrl Pts',(0.6515281822355,-1.009038926982,-4.225239569721));
#27878=CARTESIAN_POINT('Ctrl Pts',(-0.169236898936,-1.189120431432,-4.282114569721));
#27879=CARTESIAN_POINT('Ctrl Pts',(-0.9071712857378,-0.7872031419892,-4.338989569721));
#27880=CARTESIAN_POINT('Ctrl Pts',(-1.201103046544,0.,-4.395864569721));
#27881=CARTESIAN_POINT('Ctrl Pts',(-0.9071712857378,0.7872031419892,-4.452739569721));
#27882=CARTESIAN_POINT('Ctrl Pts',(-0.169236898936,1.189120431432,-4.509614569721));
#27883=CARTESIAN_POINT('Ctrl Pts',(0.6515281822355,1.009038926982,-4.566489569721));
#27884=CARTESIAN_POINT('Ctrl Pts',(1.153411671532,0.3350970673819,-4.623364569721));
#27885=CARTESIAN_POINT('Ctrl Pts',(1.090773532456,-0.5028534860695,-4.680239569721));
#27886=CARTESIAN_POINT('Ctrl Pts',(0.4942711510281,-1.094689252768,-4.737114569721));
#27887=CARTESIAN_POINT('Ctrl Pts',(-0.3441455177085,-1.150744276231,-4.793989569721));
#27888=CARTESIAN_POINT('Ctrl Pts',(-1.014124826746,-0.6435832038027,-4.850864569721));
#27889=CARTESIAN_POINT('Ctrl Pts',(-1.187754649245,0.1785709428966,-4.907739569721));
#27890=CARTESIAN_POINT('Ctrl Pts',(-0.7800537946193,0.9133258114035,-4.964614569721));
#27891=CARTESIAN_POINT('Ctrl Pts',(0.009432467987837,1.201066414053,-5.021489569721));
#27892=CARTESIAN_POINT('Ctrl Pts',(0.7943069665412,0.9009591520544,-5.078364569721));
#27893=CARTESIAN_POINT('Ctrl Pts',(1.190400720751,0.1598981886148,-5.135239569721));
#27894=CARTESIAN_POINT('Ctrl Pts',(1.003936318643,-0.6594544137959,-5.192114569721));
#27895=CARTESIAN_POINT('Ctrl Pts',(0.3258579542137,-1.155927922117,-5.248989569721));
#27896=CARTESIAN_POINT('Ctrl Pts',(-0.2318942596183,-1.110035356068,-5.286906236387));
#27897=CARTESIAN_POINT('Ctrl Pts',(-0.4696881186261,-0.9981380597272,-5.305864569721));
#27898=CARTESIAN_POINT('Ctrl Pts',(-0.5279823721497,1.122019654338,-3.564910694393));
#27899=CARTESIAN_POINT('Ctrl Pts',(-0.2606752788197,1.247804824574,-3.583869027727));
#27900=CARTESIAN_POINT('Ctrl Pts',(0.3663010598456,1.299393240218,-3.621785694393));
#27901=CARTESIAN_POINT('Ctrl Pts',(1.128537550737,0.7413010717389,-3.678660694393));
#27902=CARTESIAN_POINT('Ctrl Pts',(1.33814455045,-0.1797435821333,-3.735535694393));
#27903=CARTESIAN_POINT('Ctrl Pts',(0.892890536887,-1.012779611507,-3.792410694393));
#27904=CARTESIAN_POINT('Ctrl Pts',(0.01060315691615,-1.350133991585,-3.849285694393));
#27905=CARTESIAN_POINT('Ctrl Pts',(-0.8768683655278,-1.026681130153,-3.906160694393));
#27906=CARTESIAN_POINT('Ctrl Pts',(-1.335170067905,-0.2007338620856,-3.963035694393));
#27907=CARTESIAN_POINT('Ctrl Pts',(-1.139990581936,0.723460043259,-4.019910694393));
#27908=CARTESIAN_POINT('Ctrl Pts',(-0.3868583419482,1.293566238123,-4.076785694393));
#27909=CARTESIAN_POINT('Ctrl Pts',(0.555616470709,1.230554075189,-4.133660694393));
#27910=CARTESIAN_POINT('Ctrl Pts',(1.226152364316,0.5652639823961,-4.190535694393));
#27911=CARTESIAN_POINT('Ctrl Pts',(1.296564691016,-0.3766868641562,-4.247410694393));
#27912=CARTESIAN_POINT('Ctrl Pts',(0.7323910942975,-1.134273457497,-4.304285694393));
#27913=CARTESIAN_POINT('Ctrl Pts',(-0.190241344867,-1.336705360987,-4.361160694393));
#27914=CARTESIAN_POINT('Ctrl Pts',(-1.019762749782,-0.8849050375959,-4.418035694393));
#27915=CARTESIAN_POINT('Ctrl Pts',(-1.350175170634,0.,-4.474910694393));
#27916=CARTESIAN_POINT('Ctrl Pts',(-1.019762749782,0.8849050375959,-4.531785694393));
#27917=CARTESIAN_POINT('Ctrl Pts',(-0.190241344867,1.336705360987,-4.588660694393));
#27918=CARTESIAN_POINT('Ctrl Pts',(0.7323910942975,1.134273457497,-4.645535694393));
#27919=CARTESIAN_POINT('Ctrl Pts',(1.296564691016,0.3766868641562,-4.702410694393));
#27920=CARTESIAN_POINT('Ctrl Pts',(1.226152364316,-0.5652639823961,-4.759285694393));
#27921=CARTESIAN_POINT('Ctrl Pts',(0.555616470709,-1.230554075189,-4.816160694393));
#27922=CARTESIAN_POINT('Ctrl Pts',(-0.3868583419482,-1.293566238123,-4.873035694393));
#27923=CARTESIAN_POINT('Ctrl Pts',(-1.139990581936,-0.723460043259,-4.929910694393));
#27924=CARTESIAN_POINT('Ctrl Pts',(-1.335170067905,0.2007338620856,-4.986785694393));
#27925=CARTESIAN_POINT('Ctrl Pts',(-0.8768683655278,1.026681130153,-5.043660694393));
#27926=CARTESIAN_POINT('Ctrl Pts',(0.01060315691615,1.350133991585,-5.100535694393));
#27927=CARTESIAN_POINT('Ctrl Pts',(0.892890536887,1.012779611507,-5.157410694393));
#27928=CARTESIAN_POINT('Ctrl Pts',(1.33814455045,0.1797435821333,-5.214285694393));
#27929=CARTESIAN_POINT('Ctrl Pts',(1.128537550737,-0.7413010717389,-5.271160694393));
#27930=CARTESIAN_POINT('Ctrl Pts',(0.3663010598456,-1.299393240218,-5.328035694393));
#27931=CARTESIAN_POINT('Ctrl Pts',(-0.2606752788197,-1.247804824574,-5.36595236106));
#27932=CARTESIAN_POINT('Ctrl Pts',(-0.5279823721497,-1.122019654338,-5.384910694393));
#27933=CARTESIAN_POINT('Ctrl Pts',(-0.5862766256734,1.24590124895,-3.643956819066));
#27934=CARTESIAN_POINT('Ctrl Pts',(-0.2894562980212,1.38557429308,-3.662915152399));
#27935=CARTESIAN_POINT('Ctrl Pts',(0.4067441654775,1.442858558319,-3.700831819066));
#27936=CARTESIAN_POINT('Ctrl Pts',(1.253138782831,0.823147729682,-3.757706819066));
#27937=CARTESIAN_POINT('Ctrl Pts',(1.48588838015,-0.1995889756518,-3.814581819066));
#27938=CARTESIAN_POINT('Ctrl Pts',(0.9914741072328,-1.12460007096,-3.871456819066));
#27939=CARTESIAN_POINT('Ctrl Pts',(0.01177384584447,-1.499201569118,-3.928331819066));
#27940=CARTESIAN_POINT('Ctrl Pts',(-0.9736829364363,-1.140036448902,-3.985206819066));
#27941=CARTESIAN_POINT('Ctrl Pts',(-1.482585486565,-0.2228967812747,-4.042081819066));
#27942=CARTESIAN_POINT('Ctrl Pts',(-1.265856337127,0.8033368827153,-4.098956819066));
#27943=CARTESIAN_POINT('Ctrl Pts',(-0.4295711661878,1.436388200015,-4.155831819066));
#27944=CARTESIAN_POINT('Ctrl Pts',(0.61696179039,1.36641889761,-4.212706819066));
#27945=CARTESIAN_POINT('Ctrl Pts',(1.361531196175,0.6276744787227,-4.269581819066));
#27946=CARTESIAN_POINT('Ctrl Pts',(1.439717710501,-0.4182766609306,-4.326456819066));
#27947=CARTESIAN_POINT('Ctrl Pts',(0.8132540063595,-1.259507988013,-4.383331819066));
#27948=CARTESIAN_POINT('Ctrl Pts',(-0.211245790798,-1.484290290542,-4.440206819066));
#27949=CARTESIAN_POINT('Ctrl Pts',(-1.132354213826,-0.9826069332027,-4.497081819066));
#27950=CARTESIAN_POINT('Ctrl Pts',(-1.499247294724,0.,-4.553956819066));
#27951=CARTESIAN_POINT('Ctrl Pts',(-1.132354213826,0.9826069332027,-4.610831819066));
#27952=CARTESIAN_POINT('Ctrl Pts',(-0.211245790798,1.484290290542,-4.667706819066));
#27953=CARTESIAN_POINT('Ctrl Pts',(0.8132540063595,1.259507988013,-4.724581819066));
#27954=CARTESIAN_POINT('Ctrl Pts',(1.439717710501,0.4182766609306,-4.781456819066));
#27955=CARTESIAN_POINT('Ctrl Pts',(1.361531196175,-0.6276744787227,-4.838331819066));
#27956=CARTESIAN_POINT('Ctrl Pts',(0.61696179039,-1.36641889761,-4.895206819066));
#27957=CARTESIAN_POINT('Ctrl Pts',(-0.4295711661878,-1.436388200015,-4.952081819066));
#27958=CARTESIAN_POINT('Ctrl Pts',(-1.265856337127,-0.8033368827153,-5.008956819066));
#27959=CARTESIAN_POINT('Ctrl Pts',(-1.482585486565,0.2228967812747,-5.065831819066));
#27960=CARTESIAN_POINT('Ctrl Pts',(-0.9736829364363,1.140036448902,-5.122706819066));
#27961=CARTESIAN_POINT('Ctrl Pts',(0.01177384584447,1.499201569118,-5.179581819066));
#27962=CARTESIAN_POINT('Ctrl Pts',(0.9914741072328,1.12460007096,-5.236456819066));
#27963=CARTESIAN_POINT('Ctrl Pts',(1.48588838015,0.1995889756517,-5.293331819066));
#27964=CARTESIAN_POINT('Ctrl Pts',(1.253138782831,-0.823147729682,-5.350206819066));
#27965=CARTESIAN_POINT('Ctrl Pts',(0.4067441654775,-1.442858558319,-5.407081819066));
#27966=CARTESIAN_POINT('Ctrl Pts',(-0.2894562980212,-1.38557429308,-5.444998485733));
#27967=CARTESIAN_POINT('Ctrl Pts',(-0.5862766256734,-1.24590124895,-5.463956819066));
#27968=CARTESIAN_POINT('Ctrl Pts',(-0.644570879197,1.369782843561,-3.723002943739));
#27969=CARTESIAN_POINT('Ctrl Pts',(-0.3182373172226,1.523343761587,-3.741961277072));
#27970=CARTESIAN_POINT('Ctrl Pts',(0.4471872711094,1.586323876419,-3.779877943739));
#27971=CARTESIAN_POINT('Ctrl Pts',(1.377740014924,0.904994387625,-3.836752943739));
#27972=CARTESIAN_POINT('Ctrl Pts',(1.633632209849,-0.2194343691702,-3.893627943739));
#27973=CARTESIAN_POINT('Ctrl Pts',(1.090057677579,-1.236420530413,-3.950502943739));
#27974=CARTESIAN_POINT('Ctrl Pts',(0.01294453477278,-1.648269146651,-4.007377943739));
#27975=CARTESIAN_POINT('Ctrl Pts',(-1.070497507345,-1.253391767652,-4.064252943739));
#27976=CARTESIAN_POINT('Ctrl Pts',(-1.630000905225,-0.2450597004638,-4.121127943739));
#27977=CARTESIAN_POINT('Ctrl Pts',(-1.391722092318,0.8832137221716,-4.178002943739));
#27978=CARTESIAN_POINT('Ctrl Pts',(-0.4722839904274,1.579210161907,-4.234877943739));
#27979=CARTESIAN_POINT('Ctrl Pts',(0.6783071100709,1.502283720031,-4.291752943739));
#27980=CARTESIAN_POINT('Ctrl Pts',(1.496910028035,0.6900849750494,-4.348627943739));
#27981=CARTESIAN_POINT('Ctrl Pts',(1.582870729986,-0.4598664577049,-4.405502943739));
#27982=CARTESIAN_POINT('Ctrl Pts',(0.8941169184216,-1.384742518528,-4.462377943739));
#27983=CARTESIAN_POINT('Ctrl Pts',(-0.232250236729,-1.631875220096,-4.519252943739));
#27984=CARTESIAN_POINT('Ctrl Pts',(-1.24494567787,-1.080308828809,-4.576127943739));
#27985=CARTESIAN_POINT('Ctrl Pts',(-1.648319418813,0.,-4.633002943739));
#27986=CARTESIAN_POINT('Ctrl Pts',(-1.24494567787,1.080308828809,-4.689877943739));
#27987=CARTESIAN_POINT('Ctrl Pts',(-0.232250236729,1.631875220096,-4.746752943739));
#27988=CARTESIAN_POINT('Ctrl Pts',(0.8941169184215,1.384742518528,-4.803627943739));
#27989=CARTESIAN_POINT('Ctrl Pts',(1.582870729986,0.4598664577049,-4.860502943739));
#27990=CARTESIAN_POINT('Ctrl Pts',(1.496910028035,-0.6900849750494,-4.917377943739));
#27991=CARTESIAN_POINT('Ctrl Pts',(0.6783071100709,-1.502283720031,-4.974252943739));
#27992=CARTESIAN_POINT('Ctrl Pts',(-0.4722839904274,-1.579210161907,-5.031127943739));
#27993=CARTESIAN_POINT('Ctrl Pts',(-1.391722092318,-0.8832137221716,-5.088002943739));
#27994=CARTESIAN_POINT('Ctrl Pts',(-1.630000905225,0.2450597004637,-5.144877943739));
#27995=CARTESIAN_POINT('Ctrl Pts',(-1.070497507345,1.253391767652,-5.201752943739));
#27996=CARTESIAN_POINT('Ctrl Pts',(0.01294453477278,1.648269146651,-5.258627943739));
#27997=CARTESIAN_POINT('Ctrl Pts',(1.090057677579,1.236420530413,-5.315502943739));
#27998=CARTESIAN_POINT('Ctrl Pts',(1.633632209849,0.2194343691702,-5.372377943739));
#27999=CARTESIAN_POINT('Ctrl Pts',(1.377740014924,-0.904994387625,-5.429252943739));
#28000=CARTESIAN_POINT('Ctrl Pts',(0.4471872711094,-1.586323876419,-5.486127943739));
#28001=CARTESIAN_POINT('Ctrl Pts',(-0.3182373172226,-1.523343761587,-5.524044610405));
#28002=CARTESIAN_POINT('Ctrl Pts',(-0.644570879197,-1.369782843561,-5.543002943739));
#28003=CARTESIAN_POINT('',(2.00265715005522E-9,-1.49923261689948,-5.49955700101554));
#28004=CARTESIAN_POINT('',(0.,-1.116987298108,-5.278867513459));
#28005=CARTESIAN_POINT('Ctrl Pts',(2.25467602528104E-5,-1.49898153326899,
-5.49997328559406));
#28006=CARTESIAN_POINT('Ctrl Pts',(0.134374632780694,-1.49921303139129,
-5.49283677341645));
#28007=CARTESIAN_POINT('Ctrl Pts',(0.268791711313178,-1.48175186835438,
-5.48571144240093));
#28008=CARTESIAN_POINT('Ctrl Pts',(0.528400848841846,-1.41037838885025,
-5.47147567834219));
#28009=CARTESIAN_POINT('Ctrl Pts',(0.652827217258384,-1.35636907961786,
-5.46434951866967));
#28010=CARTESIAN_POINT('Ctrl Pts',(0.931735289868362,-1.18914017573126,
-5.44707780898663));
#28011=CARTESIAN_POINT('Ctrl Pts',(1.0775086183468,-1.05993239151383,-5.4368919202179));
#28012=CARTESIAN_POINT('Ctrl Pts',(1.25254461905446,-0.831135380419128,
-5.42160664710595));
#28013=CARTESIAN_POINT('Ctrl Pts',(1.30304065093549,-0.749217256680278,
-5.41653951416285));
#28014=CARTESIAN_POINT('Ctrl Pts',(1.43181234949439,-0.48562302793946,-5.40097007701216));
#28015=CARTESIAN_POINT('Ctrl Pts',(1.48316633571126,-0.29136688504635,-5.39048349311008));
#28016=CARTESIAN_POINT('Ctrl Pts',(1.50934593665312,0.102298274369429,-5.36953593036026));
#28017=CARTESIAN_POINT('Ctrl Pts',(1.48352321036142,0.29707569525196,-5.35935212513633));
#28018=CARTESIAN_POINT('Ctrl Pts',(1.35557797560351,0.667978516742168,-5.33851892320214));
#28019=CARTESIAN_POINT('Ctrl Pts',(1.25672301292779,0.839706906902107,-5.32816967902004));
#28020=CARTESIAN_POINT('Ctrl Pts',(1.06762964134381,1.05767331909946,-5.31285466460304));
#28021=CARTESIAN_POINT('Ctrl Pts',(0.999122897304844,1.12299761706242,-5.30786873726412));
#28022=CARTESIAN_POINT('Ctrl Pts',(0.767475871655381,1.30345314303507,-5.29230751729651));
#28023=CARTESIAN_POINT('Ctrl Pts',(0.585984031534433,1.39346687732159,-5.28173765255888));
#28024=CARTESIAN_POINT('Ctrl Pts',(0.3002776975602,1.4720722090405,-5.26599600192716));
#28025=CARTESIAN_POINT('Ctrl Pts',(0.203413384541745,1.48897914475702,-5.26079850668725));
#28026=CARTESIAN_POINT('Ctrl Pts',(0.0102965460479719,1.50310836187032,
-5.25053280796051));
#28027=CARTESIAN_POINT('Ctrl Pts',(-0.084730733565112,1.50057825774572,
-5.24552882507392));
#28028=CARTESIAN_POINT('Ctrl Pts',(-0.371065819632636,1.46518482322893,
-5.23022026530771));
#28029=CARTESIAN_POINT('Ctrl Pts',(-0.558528756656742,1.40403954733574,
-5.21992086302571));
#28030=CARTESIAN_POINT('Ctrl Pts',(-0.901532905294185,1.21492371530542,
-5.19911971442108));
#28031=CARTESIAN_POINT('Ctrl Pts',(-1.05210340104688,1.0874442058747,-5.18889366548199));
#28032=CARTESIAN_POINT('Ctrl Pts',(-1.29645242039468,0.777009440525124,
-5.16791551248259));
#28033=CARTESIAN_POINT('Ctrl Pts',(-1.387965754438,0.598976339288918,-5.15746395273279));
#28034=CARTESIAN_POINT('Ctrl Pts',(-1.49653071624039,0.222284446845803,
-5.13665963474268));
#28035=CARTESIAN_POINT('Ctrl Pts',(-1.51209522263139,0.030383479807373,
-5.12667623865883));
#28036=CARTESIAN_POINT('Ctrl Pts',(-1.46756783108178,-0.362285702864463,
-5.10568820827822));
#28037=CARTESIAN_POINT('Ctrl Pts',(-1.40686737422156,-0.555204232228066,
-5.09513613303635));
#28038=CARTESIAN_POINT('Ctrl Pts',(-1.26475536972579,-0.812299777461656,
-5.07955745535228));
#28039=CARTESIAN_POINT('Ctrl Pts',(-1.21076619934412,-0.890422714394832,
-5.07455458596799));
#28040=CARTESIAN_POINT('Ctrl Pts',(-1.02479811336611,-1.11092237734564,
-5.05923718121733));
#28041=CARTESIAN_POINT('Ctrl Pts',(-0.871086046599528,-1.23469590658041,
-5.04892246362952));
#28042=CARTESIAN_POINT('Ctrl Pts',(-0.59349076679898,-1.38245306620357,
-5.03222967142159));
#28043=CARTESIAN_POINT('Ctrl Pts',(-0.479555196543473,-1.42667705756963,
-5.02581121874688));
#28044=CARTESIAN_POINT('Ctrl Pts',(-0.24284437946229,-1.48495860067024,
-5.01291338844306));
#28045=CARTESIAN_POINT('Ctrl Pts',(-0.121403302012765,-1.49919069967036,
-5.0064742156347));
#28046=CARTESIAN_POINT('Ctrl Pts',(-2.23097736033392E-5,-1.49898153286063,
-5.00002670181768));
#28047=CARTESIAN_POINT('Ctrl Pts',(0.644570879197,-1.369782843561,-4.956997056261));
#28048=CARTESIAN_POINT('Ctrl Pts',(0.3182373172226,-1.523343761587,-4.975955389595));
#28049=CARTESIAN_POINT('Ctrl Pts',(-0.4471872711094,-1.586323876419,-5.013872056261));
#28050=CARTESIAN_POINT('Ctrl Pts',(-1.377740014924,-0.904994387625,-5.070747056261));
#28051=CARTESIAN_POINT('Ctrl Pts',(-1.633632209849,0.2194343691702,-5.127622056261));
#28052=CARTESIAN_POINT('Ctrl Pts',(-1.090057677579,1.236420530413,-5.184497056261));
#28053=CARTESIAN_POINT('Ctrl Pts',(-0.01294453477278,1.648269146651,-5.241372056261));
#28054=CARTESIAN_POINT('Ctrl Pts',(1.070497507345,1.253391767652,-5.298247056261));
#28055=CARTESIAN_POINT('Ctrl Pts',(1.630000905225,0.2450597004638,-5.355122056261));
#28056=CARTESIAN_POINT('Ctrl Pts',(1.391722092318,-0.8832137221716,-5.411997056261));
#28057=CARTESIAN_POINT('Ctrl Pts',(0.4722839904274,-1.579210161907,-5.468872056261));
#28058=CARTESIAN_POINT('Ctrl Pts',(-0.6783071100709,-1.502283720031,-5.525747056261));
#28059=CARTESIAN_POINT('Ctrl Pts',(-1.496910028035,-0.6900849750494,-5.582622056261));
#28060=CARTESIAN_POINT('Ctrl Pts',(-1.582870729986,0.4598664577049,-5.639497056261));
#28061=CARTESIAN_POINT('Ctrl Pts',(-0.8941169184216,1.384742518528,-5.696372056261));
#28062=CARTESIAN_POINT('Ctrl Pts',(0.232250236729,1.631875220096,-5.753247056261));
#28063=CARTESIAN_POINT('Ctrl Pts',(1.24494567787,1.080308828809,-5.810122056261));
#28064=CARTESIAN_POINT('Ctrl Pts',(1.648319418813,0.,-5.866997056261));
#28065=CARTESIAN_POINT('Ctrl Pts',(1.24494567787,-1.080308828809,-5.923872056261));
#28066=CARTESIAN_POINT('Ctrl Pts',(0.232250236729,-1.631875220096,-5.980747056261));
#28067=CARTESIAN_POINT('Ctrl Pts',(-0.8941169184215,-1.384742518528,-6.037622056261));
#28068=CARTESIAN_POINT('Ctrl Pts',(-1.582870729986,-0.459866457705,-6.094497056261));
#28069=CARTESIAN_POINT('Ctrl Pts',(-1.496910028035,0.6900849750494,-6.151372056261));
#28070=CARTESIAN_POINT('Ctrl Pts',(-0.6783071100709,1.502283720031,-6.208247056261));
#28071=CARTESIAN_POINT('Ctrl Pts',(0.4722839904274,1.579210161907,-6.265122056261));
#28072=CARTESIAN_POINT('Ctrl Pts',(1.391722092318,0.8832137221716,-6.321997056261));
#28073=CARTESIAN_POINT('Ctrl Pts',(1.630000905225,-0.2450597004637,-6.378872056261));
#28074=CARTESIAN_POINT('Ctrl Pts',(1.070497507345,-1.253391767652,-6.435747056261));
#28075=CARTESIAN_POINT('Ctrl Pts',(-0.01294453477276,-1.648269146651,-6.492622056261));
#28076=CARTESIAN_POINT('Ctrl Pts',(-1.090057677579,-1.236420530413,-6.549497056261));
#28077=CARTESIAN_POINT('Ctrl Pts',(-1.633632209849,-0.2194343691702,-6.606372056261));
#28078=CARTESIAN_POINT('Ctrl Pts',(-1.377740014924,0.904994387625,-6.663247056261));
#28079=CARTESIAN_POINT('Ctrl Pts',(-0.4471872711094,1.586323876419,-6.720122056261));
#28080=CARTESIAN_POINT('Ctrl Pts',(0.3182373172226,1.523343761587,-6.758038722928));
#28081=CARTESIAN_POINT('Ctrl Pts',(0.644570879197,1.369782843561,-6.776997056261));
#28082=CARTESIAN_POINT('Ctrl Pts',(0.5862766256734,-1.24590124895,-5.036043180934));
#28083=CARTESIAN_POINT('Ctrl Pts',(0.2894562980212,-1.38557429308,-5.055001514267));
#28084=CARTESIAN_POINT('Ctrl Pts',(-0.4067441654775,-1.442858558319,-5.092918180934));
#28085=CARTESIAN_POINT('Ctrl Pts',(-1.253138782831,-0.823147729682,-5.149793180934));
#28086=CARTESIAN_POINT('Ctrl Pts',(-1.48588838015,0.1995889756518,-5.206668180934));
#28087=CARTESIAN_POINT('Ctrl Pts',(-0.9914741072328,1.12460007096,-5.263543180934));
#28088=CARTESIAN_POINT('Ctrl Pts',(-0.01177384584447,1.499201569118,-5.320418180934));
#28089=CARTESIAN_POINT('Ctrl Pts',(0.9736829364363,1.140036448902,-5.377293180934));
#28090=CARTESIAN_POINT('Ctrl Pts',(1.482585486565,0.2228967812747,-5.434168180934));
#28091=CARTESIAN_POINT('Ctrl Pts',(1.265856337127,-0.8033368827153,-5.491043180934));
#28092=CARTESIAN_POINT('Ctrl Pts',(0.4295711661878,-1.436388200015,-5.547918180934));
#28093=CARTESIAN_POINT('Ctrl Pts',(-0.61696179039,-1.36641889761,-5.604793180934));
#28094=CARTESIAN_POINT('Ctrl Pts',(-1.361531196175,-0.6276744787227,-5.661668180934));
#28095=CARTESIAN_POINT('Ctrl Pts',(-1.439717710501,0.4182766609306,-5.718543180934));
#28096=CARTESIAN_POINT('Ctrl Pts',(-0.8132540063595,1.259507988013,-5.775418180934));
#28097=CARTESIAN_POINT('Ctrl Pts',(0.211245790798,1.484290290542,-5.832293180934));
#28098=CARTESIAN_POINT('Ctrl Pts',(1.132354213826,0.9826069332027,-5.889168180934));
#28099=CARTESIAN_POINT('Ctrl Pts',(1.499247294724,0.,-5.946043180934));
#28100=CARTESIAN_POINT('Ctrl Pts',(1.132354213826,-0.9826069332027,-6.002918180934));
#28101=CARTESIAN_POINT('Ctrl Pts',(0.211245790798,-1.484290290542,-6.059793180934));
#28102=CARTESIAN_POINT('Ctrl Pts',(-0.8132540063595,-1.259507988013,-6.116668180934));
#28103=CARTESIAN_POINT('Ctrl Pts',(-1.439717710501,-0.4182766609306,-6.173543180934));
#28104=CARTESIAN_POINT('Ctrl Pts',(-1.361531196175,0.6276744787227,-6.230418180934));
#28105=CARTESIAN_POINT('Ctrl Pts',(-0.61696179039,1.36641889761,-6.287293180934));
#28106=CARTESIAN_POINT('Ctrl Pts',(0.4295711661878,1.436388200015,-6.344168180934));
#28107=CARTESIAN_POINT('Ctrl Pts',(1.265856337127,0.8033368827153,-6.401043180934));
#28108=CARTESIAN_POINT('Ctrl Pts',(1.482585486565,-0.2228967812747,-6.457918180934));
#28109=CARTESIAN_POINT('Ctrl Pts',(0.9736829364363,-1.140036448902,-6.514793180934));
#28110=CARTESIAN_POINT('Ctrl Pts',(-0.01177384584445,-1.499201569118,-6.571668180934));
#28111=CARTESIAN_POINT('Ctrl Pts',(-0.9914741072328,-1.12460007096,-6.628543180934));
#28112=CARTESIAN_POINT('Ctrl Pts',(-1.48588838015,-0.1995889756518,-6.685418180934));
#28113=CARTESIAN_POINT('Ctrl Pts',(-1.253138782831,0.823147729682,-6.742293180934));
#28114=CARTESIAN_POINT('Ctrl Pts',(-0.4067441654775,1.442858558319,-6.799168180934));
#28115=CARTESIAN_POINT('Ctrl Pts',(0.2894562980212,1.38557429308,-6.837084847601));
#28116=CARTESIAN_POINT('Ctrl Pts',(0.5862766256734,1.24590124895,-6.856043180934));
#28117=CARTESIAN_POINT('Ctrl Pts',(0.5279823721497,-1.122019654338,-5.115089305607));
#28118=CARTESIAN_POINT('Ctrl Pts',(0.2606752788197,-1.247804824574,-5.13404763894));
#28119=CARTESIAN_POINT('Ctrl Pts',(-0.3663010598456,-1.299393240218,-5.171964305607));
#28120=CARTESIAN_POINT('Ctrl Pts',(-1.128537550737,-0.7413010717389,-5.228839305607));
#28121=CARTESIAN_POINT('Ctrl Pts',(-1.33814455045,0.1797435821333,-5.285714305607));
#28122=CARTESIAN_POINT('Ctrl Pts',(-0.892890536887,1.012779611507,-5.342589305607));
#28123=CARTESIAN_POINT('Ctrl Pts',(-0.01060315691615,1.350133991585,-5.399464305607));
#28124=CARTESIAN_POINT('Ctrl Pts',(0.8768683655278,1.026681130153,-5.456339305607));
#28125=CARTESIAN_POINT('Ctrl Pts',(1.335170067905,0.2007338620856,-5.513214305607));
#28126=CARTESIAN_POINT('Ctrl Pts',(1.139990581936,-0.723460043259,-5.570089305607));
#28127=CARTESIAN_POINT('Ctrl Pts',(0.3868583419482,-1.293566238123,-5.626964305607));
#28128=CARTESIAN_POINT('Ctrl Pts',(-0.555616470709,-1.230554075189,-5.683839305607));
#28129=CARTESIAN_POINT('Ctrl Pts',(-1.226152364316,-0.5652639823961,-5.740714305607));
#28130=CARTESIAN_POINT('Ctrl Pts',(-1.296564691016,0.3766868641562,-5.797589305607));
#28131=CARTESIAN_POINT('Ctrl Pts',(-0.7323910942975,1.134273457497,-5.854464305607));
#28132=CARTESIAN_POINT('Ctrl Pts',(0.190241344867,1.336705360987,-5.911339305607));
#28133=CARTESIAN_POINT('Ctrl Pts',(1.019762749782,0.8849050375959,-5.968214305607));
#28134=CARTESIAN_POINT('Ctrl Pts',(1.350175170634,0.,-6.025089305607));
#28135=CARTESIAN_POINT('Ctrl Pts',(1.019762749782,-0.8849050375959,-6.081964305607));
#28136=CARTESIAN_POINT('Ctrl Pts',(0.190241344867,-1.336705360987,-6.138839305607));
#28137=CARTESIAN_POINT('Ctrl Pts',(-0.7323910942975,-1.134273457497,-6.195714305607));
#28138=CARTESIAN_POINT('Ctrl Pts',(-1.296564691016,-0.3766868641562,-6.252589305607));
#28139=CARTESIAN_POINT('Ctrl Pts',(-1.226152364316,0.5652639823961,-6.309464305607));
#28140=CARTESIAN_POINT('Ctrl Pts',(-0.555616470709,1.230554075189,-6.366339305607));
#28141=CARTESIAN_POINT('Ctrl Pts',(0.3868583419481,1.293566238123,-6.423214305607));
#28142=CARTESIAN_POINT('Ctrl Pts',(1.139990581936,0.723460043259,-6.480089305607));
#28143=CARTESIAN_POINT('Ctrl Pts',(1.335170067905,-0.2007338620856,-6.536964305607));
#28144=CARTESIAN_POINT('Ctrl Pts',(0.8768683655278,-1.026681130153,-6.593839305607));
#28145=CARTESIAN_POINT('Ctrl Pts',(-0.01060315691614,-1.350133991585,-6.650714305607));
#28146=CARTESIAN_POINT('Ctrl Pts',(-0.892890536887,-1.012779611507,-6.707589305607));
#28147=CARTESIAN_POINT('Ctrl Pts',(-1.33814455045,-0.1797435821333,-6.764464305607));
#28148=CARTESIAN_POINT('Ctrl Pts',(-1.128537550737,0.7413010717389,-6.821339305607));
#28149=CARTESIAN_POINT('Ctrl Pts',(-0.3663010598456,1.299393240218,-6.878214305607));
#28150=CARTESIAN_POINT('Ctrl Pts',(0.2606752788197,1.247804824574,-6.916130972273));
#28151=CARTESIAN_POINT('Ctrl Pts',(0.5279823721497,1.122019654338,-6.935089305607));
#28152=CARTESIAN_POINT('Ctrl Pts',(0.4696881186261,-0.9981380597272,-5.194135430279));
#28153=CARTESIAN_POINT('Ctrl Pts',(0.2318942596183,-1.110035356068,-5.213093763613));
#28154=CARTESIAN_POINT('Ctrl Pts',(-0.3258579542138,-1.155927922117,-5.251010430279));
#28155=CARTESIAN_POINT('Ctrl Pts',(-1.003936318643,-0.6594544137959,-5.307885430279));
#28156=CARTESIAN_POINT('Ctrl Pts',(-1.190400720751,0.1598981886148,-5.364760430279));
#28157=CARTESIAN_POINT('Ctrl Pts',(-0.7943069665412,0.9009591520544,-5.421635430279));
#28158=CARTESIAN_POINT('Ctrl Pts',(-0.009432467987835,1.201066414053,-5.478510430279));
#28159=CARTESIAN_POINT('Ctrl Pts',(0.7800537946193,0.9133258114035,-5.535385430279));
#28160=CARTESIAN_POINT('Ctrl Pts',(1.187754649245,0.1785709428966,-5.592260430279));
#28161=CARTESIAN_POINT('Ctrl Pts',(1.014124826746,-0.6435832038027,-5.649135430279));
#28162=CARTESIAN_POINT('Ctrl Pts',(0.3441455177085,-1.150744276231,-5.706010430279));
#28163=CARTESIAN_POINT('Ctrl Pts',(-0.4942711510281,-1.094689252768,-5.762885430279));
#28164=CARTESIAN_POINT('Ctrl Pts',(-1.090773532456,-0.5028534860695,-5.819760430279));
#28165=CARTESIAN_POINT('Ctrl Pts',(-1.153411671532,0.3350970673819,-5.876635430279));
#28166=CARTESIAN_POINT('Ctrl Pts',(-0.6515281822355,1.009038926982,-5.933510430279));
#28167=CARTESIAN_POINT('Ctrl Pts',(0.1692368989359,1.189120431432,-5.990385430279));
#28168=CARTESIAN_POINT('Ctrl Pts',(0.9071712857378,0.7872031419892,-6.047260430279));
#28169=CARTESIAN_POINT('Ctrl Pts',(1.201103046544,0.,-6.104135430279));
#28170=CARTESIAN_POINT('Ctrl Pts',(0.9071712857378,-0.7872031419892,-6.161010430279));
#28171=CARTESIAN_POINT('Ctrl Pts',(0.169236898936,-1.189120431432,-6.217885430279));
#28172=CARTESIAN_POINT('Ctrl Pts',(-0.6515281822355,-1.009038926982,-6.274760430279));
#28173=CARTESIAN_POINT('Ctrl Pts',(-1.153411671532,-0.3350970673819,-6.331635430279));
#28174=CARTESIAN_POINT('Ctrl Pts',(-1.090773532456,0.5028534860695,-6.388510430279));
#28175=CARTESIAN_POINT('Ctrl Pts',(-0.4942711510281,1.094689252768,-6.445385430279));
#28176=CARTESIAN_POINT('Ctrl Pts',(0.3441455177085,1.150744276231,-6.502260430279));
#28177=CARTESIAN_POINT('Ctrl Pts',(1.014124826746,0.6435832038027,-6.559135430279));
#28178=CARTESIAN_POINT('Ctrl Pts',(1.187754649245,-0.1785709428966,-6.616010430279));
#28179=CARTESIAN_POINT('Ctrl Pts',(0.7800537946193,-0.9133258114035,-6.672885430279));
#28180=CARTESIAN_POINT('Ctrl Pts',(-0.009432467987825,-1.201066414053,-6.729760430279));
#28181=CARTESIAN_POINT('Ctrl Pts',(-0.7943069665412,-0.9009591520544,-6.786635430279));
#28182=CARTESIAN_POINT('Ctrl Pts',(-1.190400720751,-0.1598981886148,-6.843510430279));
#28183=CARTESIAN_POINT('Ctrl Pts',(-1.003936318643,0.6594544137959,-6.900385430279));
#28184=CARTESIAN_POINT('Ctrl Pts',(-0.3258579542138,1.155927922117,-6.957260430279));
#28185=CARTESIAN_POINT('Ctrl Pts',(0.2318942596183,1.110035356068,-6.995177096946));
#28186=CARTESIAN_POINT('Ctrl Pts',(0.4696881186261,0.9981380597272,-7.014135430279));
#28187=CARTESIAN_POINT('',(-1.42662358638991,-0.463399121050005,-6.59977593084528));
#28188=CARTESIAN_POINT('Ctrl Pts',(2.15083409534766E-5,-1.49901358617426,
-5.49995482072371));
#28189=CARTESIAN_POINT('Ctrl Pts',(-0.0955496771557089,-1.49902499053276,
-5.50492949105024));
#28190=CARTESIAN_POINT('Ctrl Pts',(-0.191148351530597,-1.49007674570699,
-5.50991524849391));
#28191=CARTESIAN_POINT('Ctrl Pts',(-0.37345699690883,-1.45524191779854,
-5.51978321815194));
#28192=CARTESIAN_POINT('Ctrl Pts',(-0.459741647179676,-1.43048283664789,
-5.52466077371444));
#28193=CARTESIAN_POINT('Ctrl Pts',(-0.723943635231431,-1.32758178810656,
-5.54013816144375));
#28194=CARTESIAN_POINT('Ctrl Pts',(-0.868233405527567,-1.23047251955764,
-5.54904358625072));
#28195=CARTESIAN_POINT('Ctrl Pts',(-1.06773131622946,-1.05862209452624,
-5.5627333617516));
#28196=CARTESIAN_POINT('Ctrl Pts',(-1.148176903769,-0.971365181836879,-5.5688666447238));
#28197=CARTESIAN_POINT('Ctrl Pts',(-1.29946460135078,-0.762178852221788,
-5.58267595377255));
#28198=CARTESIAN_POINT('Ctrl Pts',(-1.3644246712698,-0.638332711836241,
-5.59036492013114));
#28199=CARTESIAN_POINT('Ctrl Pts',(-1.44467601633284,-0.412715739435528,
-5.60306386102242));
#28200=CARTESIAN_POINT('Ctrl Pts',(-1.46864458814352,-0.31592360121861,
-5.60822651143182));
#28201=CARTESIAN_POINT('Ctrl Pts',(-1.50036359445655,-0.0999871267283061,
-5.61958217023767));
#28202=CARTESIAN_POINT('Ctrl Pts',(-1.50392985568841,0.019865718040392,
-5.62578458245811));
#28203=CARTESIAN_POINT('Ctrl Pts',(-1.48048429463456,0.279292867532091,
-5.63973465539427));
#28204=CARTESIAN_POINT('Ctrl Pts',(-1.44774382388466,0.416424110223926,
-5.64748580997274));
#28205=CARTESIAN_POINT('Ctrl Pts',(-1.35926609047163,0.640103090039512,
-5.66023359719478));
#28206=CARTESIAN_POINT('Ctrl Pts',(-1.31363362411102,0.728719647986248,
-5.66539144215515));
#28207=CARTESIAN_POINT('Ctrl Pts',(-1.19597964848409,0.911315227476304,
-5.67669094342594));
#28208=CARTESIAN_POINT('Ctrl Pts',(-1.12053071691648,1.00319337865376,-5.68284249309459));
#28209=CARTESIAN_POINT('Ctrl Pts',(-0.935550208753491,1.18053859482883,
-5.69656896808466));
#28210=CARTESIAN_POINT('Ctrl Pts',(-0.82369018732526,1.26097102014602,-5.70414579650042));
#28211=CARTESIAN_POINT('Ctrl Pts',(-0.613558945192887,1.37147933133676,
-5.71673936389039));
#28212=CARTESIAN_POINT('Ctrl Pts',(-0.521120952615554,1.40895055110257,
-5.72190336975471));
#28213=CARTESIAN_POINT('Ctrl Pts',(-0.311906874910792,1.47097335864444,
-5.73325483817663));
#28214=CARTESIAN_POINT('Ctrl Pts',(-0.193841941583796,1.49150426139673,
-5.73945133073325));
#28215=CARTESIAN_POINT('Ctrl Pts',(0.0674181442853415,1.50520456787866,
-5.75345639078522));
#28216=CARTESIAN_POINT('Ctrl Pts',(0.208979515017795,1.49199060124383,-5.76127229255357));
#28217=CARTESIAN_POINT('Ctrl Pts',(0.443959568703562,1.43534782074056,-5.77407909312804));
#28218=CARTESIAN_POINT('Ctrl Pts',(0.538065159488263,1.40254967053854,-5.77923557246599));
#28219=CARTESIAN_POINT('Ctrl Pts',(0.735133568662664,1.31164462684568,-5.79052555352543));
#28220=CARTESIAN_POINT('Ctrl Pts',(0.836510259935816,1.24988394922922,-5.79666918237583));
#28221=CARTESIAN_POINT('Ctrl Pts',(1.03665883498361,1.0926262425576,-5.81030625510528));
#28222=CARTESIAN_POINT('Ctrl Pts',(1.13105693148402,0.994391982106476,-5.81779953159453));
#28223=CARTESIAN_POINT('Ctrl Pts',(1.26961154927999,0.80344812582879,-5.83031868033029));
#28224=CARTESIAN_POINT('Ctrl Pts',(1.31993116959101,0.717293046852347,-5.83548534136846));
#28225=CARTESIAN_POINT('Ctrl Pts',(1.41141289896438,0.51869512759628,-5.84685969634429));
#28226=CARTESIAN_POINT('Ctrl Pts',(1.448698157511,0.404363257879274,-5.85307598458818));
#28227=CARTESIAN_POINT('Ctrl Pts',(1.4998727100313,0.14538332640125,-5.86720379570343));
#28228=CARTESIAN_POINT('Ctrl Pts',(1.50673344696795,0.00142570670132477,
-5.87512531518636));
#28229=CARTESIAN_POINT('Ctrl Pts',(1.48296882824891,-0.241018735058465,
-5.88802654082655));
#28230=CARTESIAN_POINT('Ctrl Pts',(1.46352511372268,-0.338723080023819,
-5.89317987937783));
#28231=CARTESIAN_POINT('Ctrl Pts',(1.40093612574789,-0.546005230890234,
-5.90444414931358));
#28232=CARTESIAN_POINT('Ctrl Pts',(1.35404796790159,-0.654545916048239,
-5.91056561952626));
#28233=CARTESIAN_POINT('Ctrl Pts',(1.2280422871028,-0.871512931630714,-5.92401256541593));
#28234=CARTESIAN_POINT('Ctrl Pts',(1.14620866841746,-0.976467632406652,
-5.93133452999354));
#28235=CARTESIAN_POINT('Ctrl Pts',(0.979670477537851,-1.13919195358528,
-5.94370162815859));
#28236=CARTESIAN_POINT('Ctrl Pts',(0.90169883049161,-1.20154422240757,-5.94887414087997));
#28237=CARTESIAN_POINT('Ctrl Pts',(0.717694897505955,-1.32144958529579,
-5.96029902439949));
#28238=CARTESIAN_POINT('Ctrl Pts',(0.609119018060983,-1.37527468100387,
-5.966558966059));
#28239=CARTESIAN_POINT('Ctrl Pts',(0.355763322450707,-1.46468560692821,
-5.98092856922058));
#28240=CARTESIAN_POINT('Ctrl Pts',(0.210494732858562,-1.49231468129516,
-5.98905380960265));
#28241=CARTESIAN_POINT('Ctrl Pts',(-0.105114080074204,-1.50463465535023,
-6.00576685814989));
#28242=CARTESIAN_POINT('Ctrl Pts',(-0.27386121530662,-1.4831376416099,-6.01437260132996));
#28243=CARTESIAN_POINT('Ctrl Pts',(-0.598411030756974,-1.38575619535043,
-6.03221195337692));
#28244=CARTESIAN_POINT('Ctrl Pts',(-0.75158847914599,-1.30940033084702,
-6.04158964491971));
#28245=CARTESIAN_POINT('Ctrl Pts',(-0.989426246393969,-1.13320912568185,
-6.05736809915289));
#28246=CARTESIAN_POINT('Ctrl Pts',(-1.0800336556722,-1.04674081478275,-6.06381697470126));
#28247=CARTESIAN_POINT('Ctrl Pts',(-1.22229494730029,-0.873529281935807,
-6.07548158717378));
#28248=CARTESIAN_POINT('Ctrl Pts',(-1.27815266708797,-0.7901040870188,-6.08069815236894));
#28249=CARTESIAN_POINT('Ctrl Pts',(-1.38205526713629,-0.595121412220474,
-6.09249216870023));
#28250=CARTESIAN_POINT('Ctrl Pts',(-1.42533016680916,-0.482483454348762,
-6.09913901550064));
#28251=CARTESIAN_POINT('Ctrl Pts',(-1.48197162704049,-0.25462069220679,
-6.11172344484877));
#28252=CARTESIAN_POINT('Ctrl Pts',(-1.49669181174848,-0.141011276460424,
-6.11766251443455));
#28253=CARTESIAN_POINT('Ctrl Pts',(-1.50048257115899,0.0720827841409691,
-6.12875128354957));
#28254=CARTESIAN_POINT('Ctrl Pts',(-1.4925817600996,0.171597804332129,-6.13391172094632));
#28255=CARTESIAN_POINT('Ctrl Pts',(-1.44893779306281,0.414168561930941,
-6.1469478465354));
#28256=CARTESIAN_POINT('Ctrl Pts',(-1.40194658119633,0.553278086222032,
-6.15501197056988));
#28257=CARTESIAN_POINT('Ctrl Pts',(-1.28142731642128,0.786990633207509,
-6.16908997590994));
#28258=CARTESIAN_POINT('Ctrl Pts',(-1.21639079223807,0.883582018957452,
-6.17511867343625));
#28259=CARTESIAN_POINT('Ctrl Pts',(-1.07692358901623,1.04735283327409,-6.18630911703358));
#28260=CARTESIAN_POINT('Ctrl Pts',(-1.00503668752227,1.11681439646067,-6.19148064302672));
#28261=CARTESIAN_POINT('Ctrl Pts',(-0.81638657738249,1.26600851048286,-6.20422266779974));
#28262=CARTESIAN_POINT('Ctrl Pts',(-0.694798758074129,1.33679445990154,
-6.21195493099225));
#28263=CARTESIAN_POINT('Ctrl Pts',(-0.457751478199051,1.43235899883709,
-6.22564808603858));
#28264=CARTESIAN_POINT('Ctrl Pts',(-0.346640730516119,1.46285087542127,
-6.23161846437896));
#28265=CARTESIAN_POINT('Ctrl Pts',(-0.135420020266238,1.49610457258724,
-6.24274277170832));
#28266=CARTESIAN_POINT('Ctrl Pts',(-0.0357172671648247,1.50200364475123,
-6.24790714213475));
#28267=CARTESIAN_POINT('Ctrl Pts',(0.208376743658017,1.49228253689555,-6.2608353648219));
#28268=CARTESIAN_POINT('Ctrl Pts',(0.350481982480695,1.46562737257418,-6.26877796635645));
#28269=CARTESIAN_POINT('Ctrl Pts',(0.596361493247398,1.38046114911593,-6.28271295732946));
#28270=CARTESIAN_POINT('Ctrl Pts',(0.700793946292286,1.3300816912034,-6.28871804158767));
#28271=CARTESIAN_POINT('Ctrl Pts',(0.882395417781042,1.21576000229937,-6.29988171632431));
#28272=CARTESIAN_POINT('Ctrl Pts',(0.961403242228944,1.15457509213465,-6.30505037166592));
#28273=CARTESIAN_POINT('Ctrl Pts',(1.13715212872892,0.988212767642547,-6.31786557844639));
#28274=CARTESIAN_POINT('Ctrl Pts',(1.22540971732273,0.876686690679965,-6.32568061063726));
#28275=CARTESIAN_POINT('Ctrl Pts',(1.35416353490123,0.653817911199552,-6.33946808234627));
#28276=CARTESIAN_POINT('Ctrl Pts',(1.40001199010802,0.547822025382658,-6.3454511973331));
#28277=CARTESIAN_POINT('Ctrl Pts',(1.46253021302436,0.343048931027685,-6.35658995320548));
#28278=CARTESIAN_POINT('Ctrl Pts',(1.48230247613543,0.245128783009541,-6.36175590353927));
#28279=CARTESIAN_POINT('Ctrl Pts',(1.50667741775337,0.00291603616627232,
-6.3746420306679));
#28280=CARTESIAN_POINT('Ctrl Pts',(1.50028685601091,-0.140646645627876,
-6.38253714167809));
#28281=CARTESIAN_POINT('Ctrl Pts',(1.45093683814447,-0.395056510149083,
-6.39641682863631));
#28282=CARTESIAN_POINT('Ctrl Pts',(1.41589906170439,-0.505396081003056,
-6.40241333582343));
#28283=CARTESIAN_POINT('Ctrl Pts',(1.32853968721372,-0.701191607913635,
-6.41356729502109));
#28284=CARTESIAN_POINT('Ctrl Pts',(1.27917419609213,-0.788061567899416,
-6.41873490810641));
#28285=CARTESIAN_POINT('Ctrl Pts',(1.13908763570199,-0.986058514220784,
-6.43157687978795));
#28286=CARTESIAN_POINT('Ctrl Pts',(1.04075623263226,-1.08958631430917,-6.43942218074782));
#28287=CARTESIAN_POINT('Ctrl Pts',(0.837687259251639,-1.24881371019553,
-6.45324445231495));
#28288=CARTESIAN_POINT('Ctrl Pts',(0.739098733652217,-1.30915826685564,
-6.45923252175412));
#28289=CARTESIAN_POINT('Ctrl Pts',(0.545037632306977,-1.39986256838697,
-6.47037686555309));
#28290=CARTESIAN_POINT('Ctrl Pts',(0.450858267314446,-1.43319321067716,
-6.47554339967615));
#28291=CARTESIAN_POINT('Ctrl Pts',(0.214766811622813,-1.49126585950107,
-6.48841436095777));
#28292=CARTESIAN_POINT('Ctrl Pts',(0.0720492191049348,-1.50511059683625,
-6.49629230690851));
#28293=CARTESIAN_POINT('Ctrl Pts',(-0.186413734920357,-1.49215578677182,
-6.51015284666944));
#28294=CARTESIAN_POINT('Ctrl Pts',(-0.300546677067099,-1.47304380550322,
-6.51614712292677));
#28295=CARTESIAN_POINT('Ctrl Pts',(-0.506664425994047,-1.41420525200107,
-6.52729858106496));
#28296=CARTESIAN_POINT('Ctrl Pts',(-0.599629187953682,-1.37759537526464,
-6.53246594964597));
#28297=CARTESIAN_POINT('Ctrl Pts',(-0.815577659267427,-1.26677413083928,
-6.545317024093));
#28298=CARTESIAN_POINT('Ctrl Pts',(-0.932084746077253,-1.18391075257807,
-6.55317245956912));
#28299=CARTESIAN_POINT('Ctrl Pts',(-1.11841809740179,-1.00517888458096,
-6.56700187774727));
#28300=CARTESIAN_POINT('Ctrl Pts',(-1.19201686999432,-0.916103763121076,
-6.57298747263071));
#28301=CARTESIAN_POINT('Ctrl Pts',(-1.32712308915121,-0.709238017225592,
-6.58584110390239));
#28302=CARTESIAN_POINT('Ctrl Pts',(-1.38514527488612,-0.589022817269641,
-6.59271872607206));
#28303=CARTESIAN_POINT('Ctrl Pts',(-1.42628888349589,-0.463297395395638,
-6.59981789523313));
#28304=CARTESIAN_POINT('',(-1.43217561911112,-0.444902799674129,-6.6008559233962));
#28305=CARTESIAN_POINT('Ctrl Pts',(-1.43217561911112,-0.444902799674129,
-6.6008559233962));
#28306=CARTESIAN_POINT('Ctrl Pts',(-1.43039287381244,-0.451087558329368,
-6.60049242607935));
#28307=CARTESIAN_POINT('Ctrl Pts',(-1.42857006684158,-0.457261655368297,
-6.60012892876249));
#28308=CARTESIAN_POINT('Ctrl Pts',(-1.42670732833463,-0.463424572590093,
-6.59976543144564));
#28309=CARTESIAN_POINT('',(-2.07485480732137E-16,1.43111039753271,-6.78927262721387));
#28310=CARTESIAN_POINT('Ctrl Pts',(3.85108611666851E-15,1.43111039753277,
-6.78927262721387));
#28311=CARTESIAN_POINT('Ctrl Pts',(-0.147800856913735,1.43482343493628,
-6.77907114079013));
#28312=CARTESIAN_POINT('Ctrl Pts',(-0.29534771011176,1.41540626957901,-6.76933892746074));
#28313=CARTESIAN_POINT('Ctrl Pts',(-0.554938120622151,1.34022312493367,
-6.75011994068015));
#28314=CARTESIAN_POINT('Ctrl Pts',(-0.668031110176501,1.29126078102496,
-6.74113820669912));
#28315=CARTESIAN_POINT('Ctrl Pts',(-0.935437445880612,1.13229063520146,
-6.71919854254426));
#28316=CARTESIAN_POINT('Ctrl Pts',(-1.07640515392378,1.00564224957176,-6.70712143470464));
#28317=CARTESIAN_POINT('Ctrl Pts',(-1.28983172346691,0.723669754549612,
-6.68324434603939));
#28318=CARTESIAN_POINT('Ctrl Pts',(-1.36728052837544,0.575354244019802,
-6.67118963644036));
#28319=CARTESIAN_POINT('Ctrl Pts',(-1.46623442521789,0.2678743516873,-6.64885199889988));
#28320=CARTESIAN_POINT('Ctrl Pts',(-1.4899792233694,0.11197065002529,-6.63870486526541));
#28321=CARTESIAN_POINT('Ctrl Pts',(-1.48811140632177,-0.180046254082272,
-6.6195763750769));
#28322=CARTESIAN_POINT('Ctrl Pts',(-1.46902193449905,-0.314743580828287,
-6.61026854950158));
#28323=CARTESIAN_POINT('Ctrl Pts',(-1.43217561911112,-0.444902799674129,
-6.6008559233962));
#28324=CARTESIAN_POINT('',(-7.91239893927046E-11,1.11628565063362,-6.97115102811022));
#28325=CARTESIAN_POINT('Ctrl Pts',(-1.75670886845076E-15,1.43111039753272,
-6.78927262721389));
#28326=CARTESIAN_POINT('Ctrl Pts',(7.53530335141514E-16,1.37865404388881,
-6.81957735335642));
#28327=CARTESIAN_POINT('Ctrl Pts',(4.44448508960574E-12,1.32619769024498,
-6.84988207949911));
#28328=CARTESIAN_POINT('Ctrl Pts',(4.44448508960574E-12,1.22125610800045,
-6.91050821322671));
#28329=CARTESIAN_POINT('Ctrl Pts',(6.22406898798232E-15,1.16877087939972,
-6.94082962081159));
#28330=CARTESIAN_POINT('Ctrl Pts',(1.83311314657105E-15,1.11628565079912,
-6.97115102839669));
#28331=CARTESIAN_POINT('Ctrl Pts',(-2.02707198973761E-6,-1.11628565404413,
-5.22111408882413));
#28332=CARTESIAN_POINT('Ctrl Pts',(-0.0945477069597211,-1.11645974724111,
-5.22785015639956));
#28333=CARTESIAN_POINT('Ctrl Pts',(-0.189124507262874,-1.1048491526056,
-5.23459224618512));
#28334=CARTESIAN_POINT('Ctrl Pts',(-0.372801878430438,-1.05728988862616,
-5.24813470031973));
#28335=CARTESIAN_POINT('Ctrl Pts',(-0.461203748610969,-1.02120417552907,
-5.25489047871015));
#28336=CARTESIAN_POINT('Ctrl Pts',(-0.668471432388862,-0.904915646636,-5.27182073957926));
#28337=CARTESIAN_POINT('Ctrl Pts',(-0.780383055419269,-0.811029500761424,
-5.28202995426489));
#28338=CARTESIAN_POINT('Ctrl Pts',(-0.977352549963132,-0.567498199932429,
-5.30436776308206));
#28339=CARTESIAN_POINT('Ctrl Pts',(-1.03703915589556,-0.431145768277794,
-5.3147587800084));
#28340=CARTESIAN_POINT('Ctrl Pts',(-1.11066616674449,-0.178042375581379,
-5.33352929238688));
#28341=CARTESIAN_POINT('Ctrl Pts',(-1.1250370353998,-0.0352369170927895,
-5.34357133882955));
#28342=CARTESIAN_POINT('Ctrl Pts',(-1.09418460733438,0.296790717289725,
-5.36736190012804));
#28343=CARTESIAN_POINT('Ctrl Pts',(-1.02997735713436,0.440477084842023,
-5.37828381624767));
#28344=CARTESIAN_POINT('Ctrl Pts',(-0.925588908242793,0.636392952388546,
-5.39408990478641));
#28345=CARTESIAN_POINT('Ctrl Pts',(-0.840538191683126,0.751460714065282,
-5.404101988361));
#28346=CARTESIAN_POINT('Ctrl Pts',(-0.611182247799713,0.946513834085752,
-5.42558474266587));
#28347=CARTESIAN_POINT('Ctrl Pts',(-0.478234529751092,1.01917110999221,
-5.43616577485578));
#28348=CARTESIAN_POINT('Ctrl Pts',(-0.222597234321215,1.1004636264182,-5.455267721173));
#28349=CARTESIAN_POINT('Ctrl Pts',(-0.0794663775051641,1.12675755955542,
-5.46543571983759));
#28350=CARTESIAN_POINT('Ctrl Pts',(0.232981315456794,1.10176800386664,-5.48779253835339));
#28351=CARTESIAN_POINT('Ctrl Pts',(0.377700605109044,1.06037143957914,-5.49830194335543));
#28352=CARTESIAN_POINT('Ctrl Pts',(0.604852724324554,0.944731736167605,
-5.51645937858707));
#28353=CARTESIAN_POINT('Ctrl Pts',(0.731331226988477,0.86397400629993,-5.52692136770941));
#28354=CARTESIAN_POINT('Ctrl Pts',(0.94339790793788,0.613934547621962,-5.55029160325254));
#28355=CARTESIAN_POINT('Ctrl Pts',(1.01607631574408,0.484189787750145,-5.56067712497169));
#28356=CARTESIAN_POINT('Ctrl Pts',(1.11857306467123,0.173002860562905,-5.58402934320733));
#28357=CARTESIAN_POINT('Ctrl Pts',(1.12165266273671,0.0230529286473064,
-5.59448736045732));
#28358=CARTESIAN_POINT('Ctrl Pts',(1.10179845703877,-0.228016486144784,
-5.61242927917354));
#28359=CARTESIAN_POINT('Ctrl Pts',(1.06324590215936,-0.369253565391408,
-5.62266080687385));
#28360=CARTESIAN_POINT('Ctrl Pts',(0.92446485564618,-0.649976757040055,
-5.64499359014349));
#28361=CARTESIAN_POINT('Ctrl Pts',(0.825915661788595,-0.761161572818599,
-5.65536755467241));
#28362=CARTESIAN_POINT('Ctrl Pts',(0.626214316349833,-0.934430304671217,
-5.67419538133658));
#28363=CARTESIAN_POINT('Ctrl Pts',(0.502214996937518,-1.00732385711171,
-5.68425796124846));
#28364=CARTESIAN_POINT('Ctrl Pts',(0.191201997533698,-1.11682300306853,
-5.70778190972181));
#28365=CARTESIAN_POINT('Ctrl Pts',(0.0349012702549407,-1.12007370080308,
-5.71864513166231));
#28366=CARTESIAN_POINT('Ctrl Pts',(-0.203851405860774,-1.10611718857029,
-5.73567366866181));
#28367=CARTESIAN_POINT('Ctrl Pts',(-0.341786112597065,-1.07261170247851,
-5.745614088678));
#28368=CARTESIAN_POINT('Ctrl Pts',(-0.603413551668558,-0.951563052462823,
-5.76618313304261));
#28369=CARTESIAN_POINT('Ctrl Pts',(-0.725113385898973,-0.861211673415803,
-5.77676949290965));
#28370=CARTESIAN_POINT('Ctrl Pts',(-0.90527342351451,-0.663857977873294,
-5.79579742516296));
#28371=CARTESIAN_POINT('Ctrl Pts',(-0.989304020610922,-0.54516302107656,
-5.80595751403342));
#28372=CARTESIAN_POINT('Ctrl Pts',(-1.09791444748828,-0.250846118613139,
-5.82833525890648));
#28373=CARTESIAN_POINT('Ctrl Pts',(-1.12102369397598,-0.101931202388053,
-5.83885689635648));
#28374=CARTESIAN_POINT('Ctrl Pts',(-1.11127472608703,0.152382998726055,
-5.85698527230642));
#28375=CARTESIAN_POINT('Ctrl Pts',(-1.09120934524511,0.300938815206572,
-5.86743533545795));
#28376=CARTESIAN_POINT('Ctrl Pts',(-0.953355092950161,0.598483057720691,
-5.89081240762303));
#28377=CARTESIAN_POINT('Ctrl Pts',(-0.865889506205097,0.719096632405912,
-5.90121651825254));
#28378=CARTESIAN_POINT('Ctrl Pts',(-0.630908211369292,0.938430669099306,
-5.92412556939149));
#28379=CARTESIAN_POINT('Ctrl Pts',(-0.499473987912771,1.00559671816688,
-5.93443093822624));
#28380=CARTESIAN_POINT('Ctrl Pts',(-0.254954649474623,1.09592824110065,
-5.95300231361182));
#28381=CARTESIAN_POINT('Ctrl Pts',(-0.11023350814751,1.12012616746575,-5.96325541986776));
#28382=CARTESIAN_POINT('Ctrl Pts',(0.202625788977316,1.11169037854405,-5.98557375090056));
#28383=CARTESIAN_POINT('Ctrl Pts',(0.344594062565046,1.06910154094397,-5.99592507043896));
#28384=CARTESIAN_POINT('Ctrl Pts',(0.58636306509556,0.959974916638408,-6.01481521721138));
#28385=CARTESIAN_POINT('Ctrl Pts',(0.704733656287621,0.87764403748791,-6.02490073023946));
#28386=CARTESIAN_POINT('Ctrl Pts',(0.924445762809005,0.651144082671899,
-6.04741286795021));
#28387=CARTESIAN_POINT('Ctrl Pts',(0.995878303027181,0.517818669122234,
-6.05795712525469));
#28388=CARTESIAN_POINT('Ctrl Pts',(1.08982166380632,0.277939862987329,-6.07630001885425));
#28389=CARTESIAN_POINT('Ctrl Pts',(1.1169872981078,0.139044412854732,-6.08621126978534));
#28390=CARTESIAN_POINT('Ctrl Pts',(1.1169872981078,-0.139044412854731,-6.10605370329665));
#28391=CARTESIAN_POINT('Ctrl Pts',(1.08982166380632,-0.277939862987325,
-6.11596495422619));
#28392=CARTESIAN_POINT('Ctrl Pts',(0.995878303027172,-0.517818669122232,
-6.13430784782587));
#28393=CARTESIAN_POINT('Ctrl Pts',(0.92444576280899,-0.651144082671897,
-6.14485210513048));
#28394=CARTESIAN_POINT('Ctrl Pts',(0.704733656287586,-0.877644037487917,
-6.16736424284125));
#28395=CARTESIAN_POINT('Ctrl Pts',(0.586363065095511,-0.959974916638421,
-6.17744975586925));
#28396=CARTESIAN_POINT('Ctrl Pts',(0.344594062564979,-1.06910154094398,
-6.19633990264163));
#28397=CARTESIAN_POINT('Ctrl Pts',(0.202625788977251,-1.11169037854405,
-6.20669122217995));
#28398=CARTESIAN_POINT('Ctrl Pts',(-0.110233508147567,-1.12012616746575,
-6.22900955321285));
#28399=CARTESIAN_POINT('Ctrl Pts',(-0.254954649474677,-1.09592824110064,
-6.23926265946891));
#28400=CARTESIAN_POINT('Ctrl Pts',(-0.499473987912839,-1.00559671816685,
-6.25783403485462));
#28401=CARTESIAN_POINT('Ctrl Pts',(-0.630908211369357,-0.93843066909926,
-6.26813940368944));
#28402=CARTESIAN_POINT('Ctrl Pts',(-0.865889506205144,-0.719096632405857,
-6.29104845482854));
#28403=CARTESIAN_POINT('Ctrl Pts',(-0.953355092950203,-0.598483057720625,
-6.30145256545815));
#28404=CARTESIAN_POINT('Ctrl Pts',(-1.09120934524514,-0.300938815206476,
-6.32482963762336));
#28405=CARTESIAN_POINT('Ctrl Pts',(-1.11127472608704,-0.152382998725948,
-6.33527970077493));
#28406=CARTESIAN_POINT('Ctrl Pts',(-1.12102369397598,0.101931202388141,
-6.35340807672478));
#28407=CARTESIAN_POINT('Ctrl Pts',(-1.09791444748826,0.250846118613222,
-6.36392971417461));
#28408=CARTESIAN_POINT('Ctrl Pts',(-0.989304020610884,0.545163021076626,
-6.38630745904754));
#28409=CARTESIAN_POINT('Ctrl Pts',(-0.905273423514468,0.66385797787335,
-6.39646754791798));
#28410=CARTESIAN_POINT('Ctrl Pts',(-0.725113385898928,0.861211673415845,
-6.41549548017135));
#28411=CARTESIAN_POINT('Ctrl Pts',(-0.603413551668504,0.951563052462865,
-6.42608184003854));
#28412=CARTESIAN_POINT('Ctrl Pts',(-0.341786112597014,1.07261170247853,
-6.44665088440311));
#28413=CARTESIAN_POINT('Ctrl Pts',(-0.203851405860737,1.1061171885703,-6.45659130441916));
#28414=CARTESIAN_POINT('Ctrl Pts',(0.0349012702549632,1.12007370080307,
-6.47361984141847));
#28415=CARTESIAN_POINT('Ctrl Pts',(0.1912019975337,1.11682300306851,-6.48448306335868));
#28416=CARTESIAN_POINT('Ctrl Pts',(0.502214996937536,1.00732385711167,-6.50800701183203));
#28417=CARTESIAN_POINT('Ctrl Pts',(0.626214316349873,0.934430304671156,
-6.51806959174408));
#28418=CARTESIAN_POINT('Ctrl Pts',(0.825915661788643,0.761161572818513,
-6.53689741840845));
#28419=CARTESIAN_POINT('Ctrl Pts',(0.92446485564623,0.64997675703996,-6.54727138293759));
#28420=CARTESIAN_POINT('Ctrl Pts',(1.06324590215939,0.369253565391305,-6.56960416620732));
#28421=CARTESIAN_POINT('Ctrl Pts',(1.10179845703878,0.228016486144688,-6.57983569390757));
#28422=CARTESIAN_POINT('Ctrl Pts',(1.12165266273671,-0.0230529286474655,
-6.59777761262373));
#28423=CARTESIAN_POINT('Ctrl Pts',(1.1185730646712,-0.173002860563037,-6.60823562987364));
#28424=CARTESIAN_POINT('Ctrl Pts',(1.01607631574405,-0.484189787750213,
-6.63158784810919));
#28425=CARTESIAN_POINT('Ctrl Pts',(0.943397907937839,-0.613934547622025,
-6.6419733698283));
#28426=CARTESIAN_POINT('Ctrl Pts',(0.731331226988405,-0.863974006299998,
-6.66534360537137));
#28427=CARTESIAN_POINT('Ctrl Pts',(0.604852724324464,-0.944731736167658,
-6.6758055944937));
#28428=CARTESIAN_POINT('Ctrl Pts',(0.377700605108989,-1.06037143957916,
-6.6939630297253));
#28429=CARTESIAN_POINT('Ctrl Pts',(0.232981315456739,-1.10176800386665,
-6.70447243472734));
#28430=CARTESIAN_POINT('Ctrl Pts',(-0.0794663775052152,-1.12675755955542,
-6.72682925324312));
#28431=CARTESIAN_POINT('Ctrl Pts',(-0.222597234321263,-1.10046362641819,
-6.73699725190771));
#28432=CARTESIAN_POINT('Ctrl Pts',(-0.478234529751139,-1.01917110999219,
-6.75609919822494));
#28433=CARTESIAN_POINT('Ctrl Pts',(-0.61118224779976,-0.94651383408572,
-6.76668023041484));
#28434=CARTESIAN_POINT('Ctrl Pts',(-0.840538191683147,-0.751460714065253,
-6.78816298471981));
#28435=CARTESIAN_POINT('Ctrl Pts',(-0.925588908242814,-0.636392952388519,
-6.79817506829455));
#28436=CARTESIAN_POINT('Ctrl Pts',(-1.02997735713431,-0.440477084842092,
-6.81398115683343));
#28437=CARTESIAN_POINT('Ctrl Pts',(-1.09418460733438,-0.296790717289793,
-6.82490307295328));
#28438=CARTESIAN_POINT('Ctrl Pts',(-1.1250370353998,0.0352369170928123,
-6.84869363425172));
#28439=CARTESIAN_POINT('Ctrl Pts',(-1.11066616674449,0.178042375581379,
-6.85873568069418));
#28440=CARTESIAN_POINT('Ctrl Pts',(-1.03703915589553,0.43114576827779,-6.87750619307247));
#28441=CARTESIAN_POINT('Ctrl Pts',(-0.977352549963096,0.567498199932421,
-6.88789720999858));
#28442=CARTESIAN_POINT('Ctrl Pts',(-0.780383055419192,0.811029500761444,
-6.91023501881583));
#28443=CARTESIAN_POINT('Ctrl Pts',(-0.668471432388746,0.904915646636041,
-6.92044423350163));
#28444=CARTESIAN_POINT('Ctrl Pts',(-0.461204333421732,1.02120384741813,
-6.93737444660179));
#28445=CARTESIAN_POINT('Ctrl Pts',(-0.372803144127186,1.05728937042922,
-6.94413017602258));
#28446=CARTESIAN_POINT('Ctrl Pts',(-0.189125242780074,1.10484915132565,
-6.95767267606297));
#28447=CARTESIAN_POINT('Ctrl Pts',(-0.0945470498259662,1.11645991446616,
-6.96441486355753));
#28448=CARTESIAN_POINT('Ctrl Pts',(-1.19666163152477E-10,1.11628565030996,
-6.97115102867089));
#28449=CARTESIAN_POINT('Ctrl Pts',(0.4696881186261,-0.9981380597272,-5.235864569721));
#28450=CARTESIAN_POINT('Ctrl Pts',(0.2318942596183,-1.110035356068,-5.254822903054));
#28451=CARTESIAN_POINT('Ctrl Pts',(-0.3258579542137,-1.155927922117,-5.292739569721));
#28452=CARTESIAN_POINT('Ctrl Pts',(-1.003936318643,-0.6594544137959,-5.349614569721));
#28453=CARTESIAN_POINT('Ctrl Pts',(-1.190400720751,0.1598981886148,-5.406489569721));
#28454=CARTESIAN_POINT('Ctrl Pts',(-0.7943069665412,0.9009591520544,-5.463364569721));
#28455=CARTESIAN_POINT('Ctrl Pts',(-0.009432467987834,1.201066414053,-5.520239569721));
#28456=CARTESIAN_POINT('Ctrl Pts',(0.7800537946193,0.9133258114035,-5.577114569721));
#28457=CARTESIAN_POINT('Ctrl Pts',(1.187754649245,0.1785709428966,-5.633989569721));
#28458=CARTESIAN_POINT('Ctrl Pts',(1.014124826746,-0.6435832038027,-5.690864569721));
#28459=CARTESIAN_POINT('Ctrl Pts',(0.3441455177085,-1.150744276231,-5.747739569721));
#28460=CARTESIAN_POINT('Ctrl Pts',(-0.4942711510281,-1.094689252768,-5.804614569721));
#28461=CARTESIAN_POINT('Ctrl Pts',(-1.090773532456,-0.5028534860695,-5.861489569721));
#28462=CARTESIAN_POINT('Ctrl Pts',(-1.153411671532,0.3350970673819,-5.918364569721));
#28463=CARTESIAN_POINT('Ctrl Pts',(-0.6515281822355,1.009038926982,-5.975239569721));
#28464=CARTESIAN_POINT('Ctrl Pts',(0.1692368989359,1.189120431432,-6.032114569721));
#28465=CARTESIAN_POINT('Ctrl Pts',(0.9071712857378,0.7872031419892,-6.088989569721));
#28466=CARTESIAN_POINT('Ctrl Pts',(1.201103046544,0.,-6.145864569721));
#28467=CARTESIAN_POINT('Ctrl Pts',(0.9071712857378,-0.7872031419892,-6.202739569721));
#28468=CARTESIAN_POINT('Ctrl Pts',(0.169236898936,-1.189120431432,-6.259614569721));
#28469=CARTESIAN_POINT('Ctrl Pts',(-0.6515281822355,-1.009038926982,-6.316489569721));
#28470=CARTESIAN_POINT('Ctrl Pts',(-1.153411671532,-0.3350970673819,-6.373364569721));
#28471=CARTESIAN_POINT('Ctrl Pts',(-1.090773532456,0.5028534860695,-6.430239569721));
#28472=CARTESIAN_POINT('Ctrl Pts',(-0.4942711510281,1.094689252768,-6.487114569721));
#28473=CARTESIAN_POINT('Ctrl Pts',(0.3441455177085,1.150744276231,-6.543989569721));
#28474=CARTESIAN_POINT('Ctrl Pts',(1.014124826746,0.6435832038027,-6.600864569721));
#28475=CARTESIAN_POINT('Ctrl Pts',(1.187754649245,-0.1785709428966,-6.657739569721));
#28476=CARTESIAN_POINT('Ctrl Pts',(0.7800537946193,-0.9133258114035,-6.714614569721));
#28477=CARTESIAN_POINT('Ctrl Pts',(-0.009432467987825,-1.201066414053,-6.771489569721));
#28478=CARTESIAN_POINT('Ctrl Pts',(-0.7943069665412,-0.9009591520544,-6.828364569721));
#28479=CARTESIAN_POINT('Ctrl Pts',(-1.190400720751,-0.1598981886148,-6.885239569721));
#28480=CARTESIAN_POINT('Ctrl Pts',(-1.003936318643,0.6594544137959,-6.942114569721));
#28481=CARTESIAN_POINT('Ctrl Pts',(-0.3258579542138,1.155927922117,-6.998989569721));
#28482=CARTESIAN_POINT('Ctrl Pts',(0.2318942596183,1.110035356068,-7.036906236387));
#28483=CARTESIAN_POINT('Ctrl Pts',(0.4696881186261,0.9981380597272,-7.055864569721));
#28484=CARTESIAN_POINT('Ctrl Pts',(0.5279823721497,-1.122019654338,-5.314910694393));
#28485=CARTESIAN_POINT('Ctrl Pts',(0.2606752788197,-1.247804824574,-5.333869027727));
#28486=CARTESIAN_POINT('Ctrl Pts',(-0.3663010598456,-1.299393240218,-5.371785694393));
#28487=CARTESIAN_POINT('Ctrl Pts',(-1.128537550737,-0.7413010717389,-5.428660694393));
#28488=CARTESIAN_POINT('Ctrl Pts',(-1.33814455045,0.1797435821333,-5.485535694393));
#28489=CARTESIAN_POINT('Ctrl Pts',(-0.892890536887,1.012779611507,-5.542410694393));
#28490=CARTESIAN_POINT('Ctrl Pts',(-0.01060315691615,1.350133991585,-5.599285694393));
#28491=CARTESIAN_POINT('Ctrl Pts',(0.8768683655278,1.026681130153,-5.656160694393));
#28492=CARTESIAN_POINT('Ctrl Pts',(1.335170067905,0.2007338620856,-5.713035694393));
#28493=CARTESIAN_POINT('Ctrl Pts',(1.139990581936,-0.723460043259,-5.769910694393));
#28494=CARTESIAN_POINT('Ctrl Pts',(0.3868583419482,-1.293566238123,-5.826785694393));
#28495=CARTESIAN_POINT('Ctrl Pts',(-0.555616470709,-1.230554075189,-5.883660694393));
#28496=CARTESIAN_POINT('Ctrl Pts',(-1.226152364316,-0.5652639823961,-5.940535694393));
#28497=CARTESIAN_POINT('Ctrl Pts',(-1.296564691016,0.3766868641562,-5.997410694393));
#28498=CARTESIAN_POINT('Ctrl Pts',(-0.7323910942975,1.134273457497,-6.054285694393));
#28499=CARTESIAN_POINT('Ctrl Pts',(0.190241344867,1.336705360987,-6.111160694393));
#28500=CARTESIAN_POINT('Ctrl Pts',(1.019762749782,0.8849050375959,-6.168035694393));
#28501=CARTESIAN_POINT('Ctrl Pts',(1.350175170634,0.,-6.224910694393));
#28502=CARTESIAN_POINT('Ctrl Pts',(1.019762749782,-0.8849050375959,-6.281785694393));
#28503=CARTESIAN_POINT('Ctrl Pts',(0.190241344867,-1.336705360987,-6.338660694393));
#28504=CARTESIAN_POINT('Ctrl Pts',(-0.7323910942975,-1.134273457497,-6.395535694393));
#28505=CARTESIAN_POINT('Ctrl Pts',(-1.296564691016,-0.3766868641562,-6.452410694393));
#28506=CARTESIAN_POINT('Ctrl Pts',(-1.226152364316,0.5652639823961,-6.509285694393));
#28507=CARTESIAN_POINT('Ctrl Pts',(-0.555616470709,1.230554075189,-6.566160694393));
#28508=CARTESIAN_POINT('Ctrl Pts',(0.3868583419481,1.293566238123,-6.623035694393));
#28509=CARTESIAN_POINT('Ctrl Pts',(1.139990581936,0.723460043259,-6.679910694393));
#28510=CARTESIAN_POINT('Ctrl Pts',(1.335170067905,-0.2007338620856,-6.736785694393));
#28511=CARTESIAN_POINT('Ctrl Pts',(0.8768683655278,-1.026681130153,-6.793660694393));
#28512=CARTESIAN_POINT('Ctrl Pts',(-0.01060315691614,-1.350133991585,-6.850535694393));
#28513=CARTESIAN_POINT('Ctrl Pts',(-0.892890536887,-1.012779611507,-6.907410694393));
#28514=CARTESIAN_POINT('Ctrl Pts',(-1.33814455045,-0.1797435821333,-6.964285694393));
#28515=CARTESIAN_POINT('Ctrl Pts',(-1.128537550737,0.7413010717389,-7.021160694393));
#28516=CARTESIAN_POINT('Ctrl Pts',(-0.3663010598456,1.299393240218,-7.078035694393));
#28517=CARTESIAN_POINT('Ctrl Pts',(0.2606752788197,1.247804824574,-7.11595236106));
#28518=CARTESIAN_POINT('Ctrl Pts',(0.5279823721497,1.122019654338,-7.134910694393));
#28519=CARTESIAN_POINT('Ctrl Pts',(0.5862766256734,-1.24590124895,-5.393956819066));
#28520=CARTESIAN_POINT('Ctrl Pts',(0.2894562980212,-1.38557429308,-5.412915152399));
#28521=CARTESIAN_POINT('Ctrl Pts',(-0.4067441654775,-1.442858558319,-5.450831819066));
#28522=CARTESIAN_POINT('Ctrl Pts',(-1.253138782831,-0.823147729682,-5.507706819066));
#28523=CARTESIAN_POINT('Ctrl Pts',(-1.48588838015,0.1995889756518,-5.564581819066));
#28524=CARTESIAN_POINT('Ctrl Pts',(-0.9914741072328,1.12460007096,-5.621456819066));
#28525=CARTESIAN_POINT('Ctrl Pts',(-0.01177384584446,1.499201569118,-5.678331819066));
#28526=CARTESIAN_POINT('Ctrl Pts',(0.9736829364363,1.140036448902,-5.735206819066));
#28527=CARTESIAN_POINT('Ctrl Pts',(1.482585486565,0.2228967812747,-5.792081819066));
#28528=CARTESIAN_POINT('Ctrl Pts',(1.265856337127,-0.8033368827153,-5.848956819066));
#28529=CARTESIAN_POINT('Ctrl Pts',(0.4295711661878,-1.436388200015,-5.905831819066));
#28530=CARTESIAN_POINT('Ctrl Pts',(-0.61696179039,-1.36641889761,-5.962706819066));
#28531=CARTESIAN_POINT('Ctrl Pts',(-1.361531196175,-0.6276744787227,-6.019581819066));
#28532=CARTESIAN_POINT('Ctrl Pts',(-1.439717710501,0.4182766609306,-6.076456819066));
#28533=CARTESIAN_POINT('Ctrl Pts',(-0.8132540063595,1.259507988013,-6.133331819066));
#28534=CARTESIAN_POINT('Ctrl Pts',(0.211245790798,1.484290290542,-6.190206819066));
#28535=CARTESIAN_POINT('Ctrl Pts',(1.132354213826,0.9826069332027,-6.247081819066));
#28536=CARTESIAN_POINT('Ctrl Pts',(1.499247294724,0.,-6.303956819066));
#28537=CARTESIAN_POINT('Ctrl Pts',(1.132354213826,-0.9826069332027,-6.360831819066));
#28538=CARTESIAN_POINT('Ctrl Pts',(0.211245790798,-1.484290290542,-6.417706819066));
#28539=CARTESIAN_POINT('Ctrl Pts',(-0.8132540063595,-1.259507988013,-6.474581819066));
#28540=CARTESIAN_POINT('Ctrl Pts',(-1.439717710501,-0.4182766609306,-6.531456819066));
#28541=CARTESIAN_POINT('Ctrl Pts',(-1.361531196175,0.6276744787227,-6.588331819066));
#28542=CARTESIAN_POINT('Ctrl Pts',(-0.61696179039,1.36641889761,-6.645206819066));
#28543=CARTESIAN_POINT('Ctrl Pts',(0.4295711661878,1.436388200015,-6.702081819066));
#28544=CARTESIAN_POINT('Ctrl Pts',(1.265856337127,0.8033368827153,-6.758956819066));
#28545=CARTESIAN_POINT('Ctrl Pts',(1.482585486565,-0.2228967812747,-6.815831819066));
#28546=CARTESIAN_POINT('Ctrl Pts',(0.9736829364363,-1.140036448902,-6.872706819066));
#28547=CARTESIAN_POINT('Ctrl Pts',(-0.01177384584445,-1.499201569118,-6.929581819066));
#28548=CARTESIAN_POINT('Ctrl Pts',(-0.9914741072328,-1.12460007096,-6.986456819066));
#28549=CARTESIAN_POINT('Ctrl Pts',(-1.48588838015,-0.1995889756518,-7.043331819066));
#28550=CARTESIAN_POINT('Ctrl Pts',(-1.253138782831,0.823147729682,-7.100206819066));
#28551=CARTESIAN_POINT('Ctrl Pts',(-0.4067441654775,1.442858558319,-7.157081819066));
#28552=CARTESIAN_POINT('Ctrl Pts',(0.2894562980212,1.38557429308,-7.194998485733));
#28553=CARTESIAN_POINT('Ctrl Pts',(0.5862766256734,1.24590124895,-7.213956819066));
#28554=CARTESIAN_POINT('Ctrl Pts',(0.644570879197,-1.369782843561,-5.473002943739));
#28555=CARTESIAN_POINT('Ctrl Pts',(0.3182373172226,-1.523343761587,-5.491961277072));
#28556=CARTESIAN_POINT('Ctrl Pts',(-0.4471872711094,-1.586323876419,-5.529877943739));
#28557=CARTESIAN_POINT('Ctrl Pts',(-1.377740014924,-0.904994387625,-5.586752943739));
#28558=CARTESIAN_POINT('Ctrl Pts',(-1.633632209849,0.2194343691702,-5.643627943739));
#28559=CARTESIAN_POINT('Ctrl Pts',(-1.090057677579,1.236420530413,-5.700502943739));
#28560=CARTESIAN_POINT('Ctrl Pts',(-0.01294453477278,1.648269146651,-5.757377943739));
#28561=CARTESIAN_POINT('Ctrl Pts',(1.070497507345,1.253391767652,-5.814252943739));
#28562=CARTESIAN_POINT('Ctrl Pts',(1.630000905225,0.2450597004638,-5.871127943739));
#28563=CARTESIAN_POINT('Ctrl Pts',(1.391722092318,-0.8832137221716,-5.928002943739));
#28564=CARTESIAN_POINT('Ctrl Pts',(0.4722839904274,-1.579210161907,-5.984877943739));
#28565=CARTESIAN_POINT('Ctrl Pts',(-0.6783071100709,-1.502283720031,-6.041752943739));
#28566=CARTESIAN_POINT('Ctrl Pts',(-1.496910028035,-0.6900849750494,-6.098627943739));
#28567=CARTESIAN_POINT('Ctrl Pts',(-1.582870729986,0.4598664577049,-6.155502943739));
#28568=CARTESIAN_POINT('Ctrl Pts',(-0.8941169184216,1.384742518528,-6.212377943739));
#28569=CARTESIAN_POINT('Ctrl Pts',(0.232250236729,1.631875220096,-6.269252943739));
#28570=CARTESIAN_POINT('Ctrl Pts',(1.24494567787,1.080308828809,-6.326127943739));
#28571=CARTESIAN_POINT('Ctrl Pts',(1.648319418813,0.,-6.383002943739));
#28572=CARTESIAN_POINT('Ctrl Pts',(1.24494567787,-1.080308828809,-6.439877943739));
#28573=CARTESIAN_POINT('Ctrl Pts',(0.232250236729,-1.631875220096,-6.496752943739));
#28574=CARTESIAN_POINT('Ctrl Pts',(-0.8941169184215,-1.384742518528,-6.553627943739));
#28575=CARTESIAN_POINT('Ctrl Pts',(-1.582870729986,-0.459866457705,-6.610502943739));
#28576=CARTESIAN_POINT('Ctrl Pts',(-1.496910028035,0.6900849750494,-6.667377943739));
#28577=CARTESIAN_POINT('Ctrl Pts',(-0.6783071100709,1.502283720031,-6.724252943739));
#28578=CARTESIAN_POINT('Ctrl Pts',(0.4722839904274,1.579210161907,-6.781127943739));
#28579=CARTESIAN_POINT('Ctrl Pts',(1.391722092317,0.8832137221716,-6.838002943739));
#28580=CARTESIAN_POINT('Ctrl Pts',(1.630000905225,-0.2450597004637,-6.894877943739));
#28581=CARTESIAN_POINT('Ctrl Pts',(1.070497507345,-1.253391767652,-6.951752943739));
#28582=CARTESIAN_POINT('Ctrl Pts',(-0.01294453477276,-1.648269146651,-7.008627943739));
#28583=CARTESIAN_POINT('Ctrl Pts',(-1.090057677579,-1.236420530413,-7.065502943739));
#28584=CARTESIAN_POINT('Ctrl Pts',(-1.633632209849,-0.2194343691702,-7.122377943739));
#28585=CARTESIAN_POINT('Ctrl Pts',(-1.377740014924,0.904994387625,-7.179252943739));
#28586=CARTESIAN_POINT('Ctrl Pts',(-0.4471872711094,1.586323876419,-7.236127943739));
#28587=CARTESIAN_POINT('Ctrl Pts',(0.3182373172226,1.523343761587,-7.274044610405));
#28588=CARTESIAN_POINT('Ctrl Pts',(0.644570879197,1.369782843561,-7.293002943739));
#28589=CARTESIAN_POINT('',(-1.20091586136076,0.574787353946053,-7.06327277934281));
#28590=CARTESIAN_POINT('',(-8.13146573628545E-11,1.31156054413043,-7.14169893232531));
#28591=CARTESIAN_POINT('Ctrl Pts',(-1.20088997011481,0.57477334405161,-7.06335361601562));
#28592=CARTESIAN_POINT('Ctrl Pts',(-1.14929466356377,0.677923899738821,
-7.06887533691862));
#28593=CARTESIAN_POINT('Ctrl Pts',(-1.08473705535376,0.773701846621558,
-7.07461408917595));
#28594=CARTESIAN_POINT('Ctrl Pts',(-0.921494131220331,0.958846554317305,
-7.08757779188294));
#28595=CARTESIAN_POINT('Ctrl Pts',(-0.820291380180567,1.04425249730464,
-7.09454782527836));
#28596=CARTESIAN_POINT('Ctrl Pts',(-0.616359073722479,1.17025704400948,
-7.10694522055062));
#28597=CARTESIAN_POINT('Ctrl Pts',(-0.517773004823371,1.21571828362488,
-7.11240671281841));
#28598=CARTESIAN_POINT('Ctrl Pts',(-0.280644665838941,1.29157780830749,
-7.12560673339976));
#28599=CARTESIAN_POINT('Ctrl Pts',(-0.140554389641116,1.31273804394784,
-7.13370645415391));
#28600=CARTESIAN_POINT('Ctrl Pts',(-1.12267799223797E-10,1.31156054441233,
-7.14169893291116));
#28601=CARTESIAN_POINT('Ctrl Pts',(-1.20091584568251,0.574787346442065,
-7.06327277301645));
#28602=CARTESIAN_POINT('Ctrl Pts',(-1.20141090039729,0.573775732839867,
-7.06324582956765));
#28603=CARTESIAN_POINT('Ctrl Pts',(-1.20190467690673,0.572763479868007,
-7.06321888611885));
#28604=CARTESIAN_POINT('Ctrl Pts',(-1.20239717356391,0.571750590758655,
-7.06319194267005));
#28605=CARTESIAN_POINT('Ctrl Pts',(-2.17187379192296E-14,-1.37969296796376,
-6.93054085392112));
#28606=CARTESIAN_POINT('Ctrl Pts',(0.133087605160917,-1.38199709859499,
-6.92421030704033));
#28607=CARTESIAN_POINT('Ctrl Pts',(0.265891834404468,-1.36490138125464,
-6.91827168076586));
#28608=CARTESIAN_POINT('Ctrl Pts',(0.564996978667766,-1.28167294134465,
-6.90378294700708));
#28609=CARTESIAN_POINT('Ctrl Pts',(0.725362476421252,-1.20192290452996,
-6.89502145187575));
#28610=CARTESIAN_POINT('Ctrl Pts',(1.0047343766773,-0.988626905368938,-6.87819012960697));
#28611=CARTESIAN_POINT('Ctrl Pts',(1.1219964500559,-0.857644336593423,-6.870640991457));
#28612=CARTESIAN_POINT('Ctrl Pts',(1.30451451661986,-0.557337293085704,
-6.85430581013491));
#28613=CARTESIAN_POINT('Ctrl Pts',(1.36739414126712,-0.389358231442156,
-6.84553910894255));
#28614=CARTESIAN_POINT('Ctrl Pts',(1.4117263467245,-0.129929452450397,-6.83326155787653));
#28615=CARTESIAN_POINT('Ctrl Pts',(1.41838750216727,-0.044275804343337,
-6.82944557901815));
#28616=CARTESIAN_POINT('Ctrl Pts',(1.41486309456447,0.228784682413614,-6.81720758348837));
#28617=CARTESIAN_POINT('Ctrl Pts',(1.37535002677926,0.414176360005993,-6.80856054737031));
#28618=CARTESIAN_POINT('Ctrl Pts',(1.26691849065933,0.666439120336986,-6.79547529965858));
#28619=CARTESIAN_POINT('Ctrl Pts',(1.22518517031265,0.743282809540594,-6.79134715792347));
#28620=CARTESIAN_POINT('Ctrl Pts',(1.07499110554378,0.967675000265378,-6.77913679426239));
#28621=CARTESIAN_POINT('Ctrl Pts',(0.944978158008963,1.09873235050051,-6.77131126083146));
#28622=CARTESIAN_POINT('Ctrl Pts',(0.641840694562588,1.30646779072398,-6.75429576162248));
#28623=CARTESIAN_POINT('Ctrl Pts',(0.47047451290788,1.38096292093851,-6.74542631518275));
#28624=CARTESIAN_POINT('Ctrl Pts',(0.200851080407334,1.44038429679966,-6.73326404861856));
#28625=CARTESIAN_POINT('Ctrl Pts',(0.110696145530379,1.45152859668681,-6.72934742419146));
#28626=CARTESIAN_POINT('Ctrl Pts',(-0.173735633177461,1.46004938761469,
-6.71675263066477));
#28627=CARTESIAN_POINT('Ctrl Pts',(-0.367192634459145,1.42716351269212,
-6.70761130652016));
#28628=CARTESIAN_POINT('Ctrl Pts',(-0.70587947037252,1.29691374915499,-6.69101716904001));
#28629=CARTESIAN_POINT('Ctrl Pts',(-0.851660931903767,1.20924258790853,
-6.68402027485137));
#28630=CARTESIAN_POINT('Ctrl Pts',(-1.12823162747451,0.970664562207185,
-6.6679529964483));
#28631=CARTESIAN_POINT('Ctrl Pts',(-1.25031504727381,0.813482669717336,
-6.65869106693004));
#28632=CARTESIAN_POINT('Ctrl Pts',(-1.41079480059823,0.490279494856505,
-6.64255921591799));
#28633=CARTESIAN_POINT('Ctrl Pts',(-1.45867635868021,0.33197073342751,-6.63583629784723));
#28634=CARTESIAN_POINT('Ctrl Pts',(-1.49310076179315,0.0682334676735931,
-6.62423350158303));
#28635=CARTESIAN_POINT('Ctrl Pts',(-1.4959309819233,-0.0339812777594436,
-6.61966622893598));
#28636=CARTESIAN_POINT('Ctrl Pts',(-1.48056746832713,-0.240323919983076,
-6.61025451548057));
#28637=CARTESIAN_POINT('Ctrl Pts',(-1.46177071919185,-0.344019227176078,
-6.60543234520265));
#28638=CARTESIAN_POINT('Ctrl Pts',(-1.43217561911113,-0.44490279967413,
-6.60085592339618));
#28639=CARTESIAN_POINT('',(6.96860469514013E-11,1.11628565060287,-7.02888605611368));
#28640=CARTESIAN_POINT('Ctrl Pts',(-1.88721574946309E-6,-1.11628565378659,
-5.27884910577848));
#28641=CARTESIAN_POINT('Ctrl Pts',(-0.0945476136912823,-1.11645975869105,
-5.28558517666919));
#28642=CARTESIAN_POINT('Ctrl Pts',(-0.189124462134144,-1.10484916429063,
-5.29232726977651));
#28643=CARTESIAN_POINT('Ctrl Pts',(-0.372801878429933,-1.05728988862636,
-5.30586972723854));
#28644=CARTESIAN_POINT('Ctrl Pts',(-0.461203748610719,-1.0212041755292,
-5.31262550562909));
#28645=CARTESIAN_POINT('Ctrl Pts',(-0.668471432388832,-0.904915646636021,
-5.32955576649842));
#28646=CARTESIAN_POINT('Ctrl Pts',(-0.780383055419245,-0.811029500761448,
-5.33976498118422));
#28647=CARTESIAN_POINT('Ctrl Pts',(-0.977352549963112,-0.56749819993246,
-5.36210279000144));
#28648=CARTESIAN_POINT('Ctrl Pts',(-1.03703915589554,-0.431145768277833,
-5.37249380692754));
#28649=CARTESIAN_POINT('Ctrl Pts',(-1.11066616674449,-0.178042375581417,
-5.39126431930582));
#28650=CARTESIAN_POINT('Ctrl Pts',(-1.1250370353998,-0.0352369170928276,
-5.40130636574828));
#28651=CARTESIAN_POINT('Ctrl Pts',(-1.09418460733438,0.2967907172898,-5.42509692704672));
#28652=CARTESIAN_POINT('Ctrl Pts',(-1.02997735713431,0.440477084842102,
-5.43601884316658));
#28653=CARTESIAN_POINT('Ctrl Pts',(-0.925588908242808,0.636392952388525,
-5.45182493170545));
#28654=CARTESIAN_POINT('Ctrl Pts',(-0.840538191683142,0.751460714065264,
-5.46183701528019));
#28655=CARTESIAN_POINT('Ctrl Pts',(-0.611182247799737,0.946513834085736,
-5.48331976958516));
#28656=CARTESIAN_POINT('Ctrl Pts',(-0.478234529751118,1.0191711099922,-5.49390080177507));
#28657=CARTESIAN_POINT('Ctrl Pts',(-0.222597234321242,1.1004636264182,-5.51300274809229));
#28658=CARTESIAN_POINT('Ctrl Pts',(-0.0794663775051934,1.12675755955542,
-5.52317074675688));
#28659=CARTESIAN_POINT('Ctrl Pts',(0.232981315456763,1.10176800386665,-5.54552756527266));
#28660=CARTESIAN_POINT('Ctrl Pts',(0.377700605109014,1.06037143957915,-5.5560369702747));
#28661=CARTESIAN_POINT('Ctrl Pts',(0.604852724324514,0.944731736167629,
-5.57419440550631));
#28662=CARTESIAN_POINT('Ctrl Pts',(0.731331226988442,0.863974006299961,
-5.58465639462863));
#28663=CARTESIAN_POINT('Ctrl Pts',(0.943397907937856,0.613934547621998,
-5.6080266301717));
#28664=CARTESIAN_POINT('Ctrl Pts',(1.01607631574406,0.484189787750186,-5.61841215189081));
#28665=CARTESIAN_POINT('Ctrl Pts',(1.11857306467121,0.173002860562979,-5.64176437012636));
#28666=CARTESIAN_POINT('Ctrl Pts',(1.12165266273671,0.0230529286473931,
-5.65222238737627));
#28667=CARTESIAN_POINT('Ctrl Pts',(1.10179845703878,-0.228016486144737,
-5.67016430609243));
#28668=CARTESIAN_POINT('Ctrl Pts',(1.06324590215937,-0.369253565391366,
-5.68039583379269));
#28669=CARTESIAN_POINT('Ctrl Pts',(0.924464855646201,-0.649976757040027,
-5.70272861706242));
#28670=CARTESIAN_POINT('Ctrl Pts',(0.825915661788616,-0.761161572818578,
-5.71310258159158));
#28671=CARTESIAN_POINT('Ctrl Pts',(0.626214316349858,-0.934430304671199,
-5.73193040825594));
#28672=CARTESIAN_POINT('Ctrl Pts',(0.502214996937545,-1.00732385711169,
-5.74199298816798));
#28673=CARTESIAN_POINT('Ctrl Pts',(0.19120199753373,-1.11682300306852,-5.76551693664133));
#28674=CARTESIAN_POINT('Ctrl Pts',(0.0349012702549799,-1.12007370080307,
-5.77638015858152));
#28675=CARTESIAN_POINT('Ctrl Pts',(-0.203851405860734,-1.1061171885703,
-5.79340869558083));
#28676=CARTESIAN_POINT('Ctrl Pts',(-0.341786112597023,-1.07261170247852,
-5.80334911559688));
#28677=CARTESIAN_POINT('Ctrl Pts',(-0.603413551668519,-0.951563052462849,
-5.82391815996146));
#28678=CARTESIAN_POINT('Ctrl Pts',(-0.72511338589894,-0.861211673415831,
-5.83450451982865));
#28679=CARTESIAN_POINT('Ctrl Pts',(-0.905273423514478,-0.663857977873336,
-5.85353245208202));
#28680=CARTESIAN_POINT('Ctrl Pts',(-0.989304020610893,-0.545163021076611,
-5.86369254095246));
#28681=CARTESIAN_POINT('Ctrl Pts',(-1.09791444748826,-0.250846118613204,
-5.88607028582539));
#28682=CARTESIAN_POINT('Ctrl Pts',(-1.12102369397598,-0.101931202388123,
-5.89659192327522));
#28683=CARTESIAN_POINT('Ctrl Pts',(-1.11127472608704,0.152382998725967,
-5.91472029922507));
#28684=CARTESIAN_POINT('Ctrl Pts',(-1.09120934524513,0.300938815206493,
-5.92517036237664));
#28685=CARTESIAN_POINT('Ctrl Pts',(-0.953355092950194,0.59848305772064,
-5.94854743454185));
#28686=CARTESIAN_POINT('Ctrl Pts',(-0.865889506205132,0.719096632405871,
-5.95895154517146));
#28687=CARTESIAN_POINT('Ctrl Pts',(-0.630908211369359,0.938430669099254,
-5.98186059631056));
#28688=CARTESIAN_POINT('Ctrl Pts',(-0.499473987912845,1.00559671816685,
-5.99216596514537));
#28689=CARTESIAN_POINT('Ctrl Pts',(-0.254954649474659,1.09592824110065,
-6.01073734053109));
#28690=CARTESIAN_POINT('Ctrl Pts',(-0.110233508147547,1.12012616746575,
-6.02099044678716));
#28691=CARTESIAN_POINT('Ctrl Pts',(0.202625788977274,1.11169037854405,-6.04330877782007));
#28692=CARTESIAN_POINT('Ctrl Pts',(0.344594062565003,1.06910154094398,-6.0536600973584));
#28693=CARTESIAN_POINT('Ctrl Pts',(0.58636306509553,0.959974916638413,-6.07255024413077));
#28694=CARTESIAN_POINT('Ctrl Pts',(0.704733656287601,0.877644037487909,
-6.08263575715877));
#28695=CARTESIAN_POINT('Ctrl Pts',(0.924445762809001,0.651144082671887,
-6.10514789486953));
#28696=CARTESIAN_POINT('Ctrl Pts',(0.995878303027181,0.517818669122219,
-6.11569215217414));
#28697=CARTESIAN_POINT('Ctrl Pts',(1.08982166380632,0.277939862987319,-6.13403504577381));
#28698=CARTESIAN_POINT('Ctrl Pts',(1.1169872981078,0.139044412854729,-6.14394629670335));
#28699=CARTESIAN_POINT('Ctrl Pts',(1.1169872981078,-0.139044412854725,-6.16378873021465));
#28700=CARTESIAN_POINT('Ctrl Pts',(1.08982166380632,-0.277939862987315,
-6.17369998114575));
#28701=CARTESIAN_POINT('Ctrl Pts',(0.995878303027181,-0.517818669122214,
-6.19204287474531));
#28702=CARTESIAN_POINT('Ctrl Pts',(0.924445762809002,-0.65114408267188,
-6.20258713204978));
#28703=CARTESIAN_POINT('Ctrl Pts',(0.704733656287603,-0.877644037487904,
-6.22509926976052));
#28704=CARTESIAN_POINT('Ctrl Pts',(0.586363065095529,-0.95997491663841,
-6.2351847827886));
#28705=CARTESIAN_POINT('Ctrl Pts',(0.344594062565005,-1.06910154094397,
-6.25407492956103));
#28706=CARTESIAN_POINT('Ctrl Pts',(0.202625788977278,-1.11169037854405,
-6.26442624909944));
#28707=CARTESIAN_POINT('Ctrl Pts',(-0.110233508147536,-1.12012616746575,
-6.28674458013225));
#28708=CARTESIAN_POINT('Ctrl Pts',(-0.254954649474642,-1.09592824110065,
-6.29699768638819));
#28709=CARTESIAN_POINT('Ctrl Pts',(-0.49947398791277,-1.00559671816688,
-6.31556906177377));
#28710=CARTESIAN_POINT('Ctrl Pts',(-0.630908211369293,-0.938430669099308,
-6.32587443060851));
#28711=CARTESIAN_POINT('Ctrl Pts',(-0.865889506205105,-0.719096632405904,
-6.34878348174746));
#28712=CARTESIAN_POINT('Ctrl Pts',(-0.953355092950167,-0.598483057720682,
-6.35918759237696));
#28713=CARTESIAN_POINT('Ctrl Pts',(-1.09120934524511,-0.300938815206565,
-6.38256466454204));
#28714=CARTESIAN_POINT('Ctrl Pts',(-1.11127472608703,-0.152382998726048,
-6.39301472769358));
#28715=CARTESIAN_POINT('Ctrl Pts',(-1.12102369397598,0.101931202388064,
-6.41114310364352));
#28716=CARTESIAN_POINT('Ctrl Pts',(-1.09791444748827,0.25084611861315,-6.42166474109352));
#28717=CARTESIAN_POINT('Ctrl Pts',(-0.989304020610917,0.545163021076569,
-6.44404248596658));
#28718=CARTESIAN_POINT('Ctrl Pts',(-0.905273423514503,0.663857977873303,
-6.45420257483704));
#28719=CARTESIAN_POINT('Ctrl Pts',(-0.725113385898966,0.861211673415812,
-6.47323050709036));
#28720=CARTESIAN_POINT('Ctrl Pts',(-0.603413551668548,0.951563052462836,
-6.48381686695739));
#28721=CARTESIAN_POINT('Ctrl Pts',(-0.341786112597061,1.07261170247852,
-6.50438591132201));
#28722=CARTESIAN_POINT('Ctrl Pts',(-0.203851405860781,1.10611718857029,
-6.5143263313382));
#28723=CARTESIAN_POINT('Ctrl Pts',(0.0349012702549208,1.12007370080308,
-6.5313548683377));
#28724=CARTESIAN_POINT('Ctrl Pts',(0.191201997533662,1.11682300306852,-6.54221809027818));
#28725=CARTESIAN_POINT('Ctrl Pts',(0.502214996937503,1.00732385711169,-6.56574203875153));
#28726=CARTESIAN_POINT('Ctrl Pts',(0.626214316349841,0.934430304671178,
-6.57580461866341));
#28727=CARTESIAN_POINT('Ctrl Pts',(0.825915661788616,0.761161572818541,
-6.59463244532758));
#28728=CARTESIAN_POINT('Ctrl Pts',(0.924464855646203,0.649976757039995,
-6.60500640985651));
#28729=CARTESIAN_POINT('Ctrl Pts',(1.06324590215937,0.369253565391355,-6.62733919312616));
#28730=CARTESIAN_POINT('Ctrl Pts',(1.10179845703877,0.228016486144744,-6.63757072082647));
#28731=CARTESIAN_POINT('Ctrl Pts',(1.12165266273671,-0.0230529286473764,
-6.65551263954268));
#28732=CARTESIAN_POINT('Ctrl Pts',(1.11857306467121,-0.173002860562959,
-6.66597065679268));
#28733=CARTESIAN_POINT('Ctrl Pts',(1.01607631574407,-0.484189787750162,
-6.68932287502831));
#28734=CARTESIAN_POINT('Ctrl Pts',(0.943397907937869,-0.613934547621979,
-6.69970839674746));
#28735=CARTESIAN_POINT('Ctrl Pts',(0.731331226988447,-0.863974006299962,
-6.72307863229059));
#28736=CARTESIAN_POINT('Ctrl Pts',(0.604852724324511,-0.944731736167631,
-6.73354062141294));
#28737=CARTESIAN_POINT('Ctrl Pts',(0.377700605109025,-1.06037143957915,
-6.75169805664457));
#28738=CARTESIAN_POINT('Ctrl Pts',(0.232981315456777,-1.10176800386664,
-6.76220746164662));
#28739=CARTESIAN_POINT('Ctrl Pts',(-0.0794663775051798,-1.12675755955542,
-6.78456428016241));
#28740=CARTESIAN_POINT('Ctrl Pts',(-0.222597234321231,-1.1004636264182,
-6.794732278827));
#28741=CARTESIAN_POINT('Ctrl Pts',(-0.478234529751108,-1.0191711099922,
-6.81383422514422));
#28742=CARTESIAN_POINT('Ctrl Pts',(-0.61118224779973,-0.946513834085739,
-6.82441525733414));
#28743=CARTESIAN_POINT('Ctrl Pts',(-0.840538191683137,-0.751460714065269,
-6.845898011639));
#28744=CARTESIAN_POINT('Ctrl Pts',(-0.925588908242802,-0.636392952388533,
-6.8559100952136));
#28745=CARTESIAN_POINT('Ctrl Pts',(-1.02997735713434,-0.440477084842058,
-6.87171618375233));
#28746=CARTESIAN_POINT('Ctrl Pts',(-1.09418460733438,-0.29679071728976,
-6.88263809987196));
#28747=CARTESIAN_POINT('Ctrl Pts',(-1.1250370353998,0.0352369170927682,
-6.90642866117045));
#28748=CARTESIAN_POINT('Ctrl Pts',(-1.11066616674449,0.178042375581336,
-6.91647070761312));
#28749=CARTESIAN_POINT('Ctrl Pts',(-1.03703915589555,0.431145768277744,
-6.93524121999159));
#28750=CARTESIAN_POINT('Ctrl Pts',(-0.977352549963121,0.56749819993238,
-6.94563223691791));
#28751=CARTESIAN_POINT('Ctrl Pts',(-0.780383055419225,0.811029500761411,
-6.96797004573509));
#28752=CARTESIAN_POINT('Ctrl Pts',(-0.668471432388786,0.904915646636011,
-6.97817926042072));
#28753=CARTESIAN_POINT('Ctrl Pts',(-0.461204214700216,1.02120391402741,
-6.99510948321823));
#28754=CARTESIAN_POINT('Ctrl Pts',(-0.372802887179955,1.05728947562774,
-7.00186522258021));
#28755=CARTESIAN_POINT('Ctrl Pts',(-0.189124960613764,1.10484918598421,
-7.0154077230962));
#28756=CARTESIAN_POINT('Ctrl Pts',(-0.0945469086635694,1.11645991422468,
-7.02214990053352));
#28757=CARTESIAN_POINT('Ctrl Pts',(1.05351468695941E-10,1.11628565030954,
-7.02888605560556));
#28758=CARTESIAN_POINT('Ctrl Pts',(1.89848396344249E-15,1.11628565075286,
-7.02888605585406));
#28759=CARTESIAN_POINT('Ctrl Pts',(-3.50013929086958E-15,1.14889336813908,
-7.04772396350255));
#28760=CARTESIAN_POINT('Ctrl Pts',(-2.79399731606342E-12,1.18150108552538,
-7.06656187115091));
#28761=CARTESIAN_POINT('Ctrl Pts',(-2.79399731606342E-12,1.24659271658915,
-7.10416616341545));
#28762=CARTESIAN_POINT('Ctrl Pts',(-1.24952051716895E-14,1.27907663026664,
-7.12293254803162));
#28763=CARTESIAN_POINT('Ctrl Pts',(2.20773575809264E-15,1.31156054394421,
-7.14169893264765));
#28764=CARTESIAN_POINT('Origin',(0.,0.,-7.2));
#28765=CARTESIAN_POINT('',(0.,1.331411920116,-7.06319194267));
#28766=CARTESIAN_POINT('Origin',(0.,1.707288968431,-7.2));
#28767=CARTESIAN_POINT('Origin',(0.,0.,-7.06319194267));
#28768=CARTESIAN_POINT('',(0.,-1.707288968431,-7.6));
#28769=CARTESIAN_POINT('Origin',(2.09082597040861E-16,-1.707288968431,-7.2));
#28770=CARTESIAN_POINT('Origin',(0.,0.,-7.6));
#28771=CARTESIAN_POINT('Origin',(0.,0.,-6.89357235801));
#28772=CARTESIAN_POINT('',(0.,1.331411920116,-7.06319194267));
#28773=CARTESIAN_POINT('Origin',(0.,1.5,-7.));
#28774=CARTESIAN_POINT('Ctrl Pts',(-2.59235181799925E-15,1.11628565030974,
-6.97115102811021));
#28775=CARTESIAN_POINT('Ctrl Pts',(-2.33645276180641E-15,1.11628565030974,
-6.98076735207347));
#28776=CARTESIAN_POINT('Ctrl Pts',(2.8796409701215E-15,1.11628565030974,
-6.99038367603674));
#28777=CARTESIAN_POINT('Ctrl Pts',(2.8796409701215E-15,1.11628565030974,
-7.00962868537123));
#28778=CARTESIAN_POINT('Ctrl Pts',(-2.34957117002464E-15,1.11628565030974,
-7.01925737074246));
#28779=CARTESIAN_POINT('Ctrl Pts',(-2.59329306483399E-15,1.11628565030974,
-7.02888605611369));
#28780=CARTESIAN_POINT('Ctrl Pts',(0.4755900604755,-1.010680324589,-5.170126599063));
#28781=CARTESIAN_POINT('Ctrl Pts',(0.2348081643589,-1.123983684464,-5.189084932396));
#28782=CARTESIAN_POINT('Ctrl Pts',(-0.329952574922,-1.170452920957,-5.227001599063));
#28783=CARTESIAN_POINT('Ctrl Pts',(-1.016551442463,-0.6677408946504,-5.283876599063));
#28784=CARTESIAN_POINT('Ctrl Pts',(-1.205358893105,0.1619074151071,-5.340751599063));
#28785=CARTESIAN_POINT('Ctrl Pts',(-0.8042879589087,0.9122802996697,-5.397626599063));
#28786=CARTESIAN_POINT('Ctrl Pts',(-0.009550993186477,1.216158607898,-5.454501599063));
#28787=CARTESIAN_POINT('Ctrl Pts',(0.7898556864549,0.9248023542725,-5.511376599063));
#28788=CARTESIAN_POINT('Ctrl Pts',(1.202679571961,0.180814804896,-5.568251599063));
#28789=CARTESIAN_POINT('Ctrl Pts',(1.026867975908,-0.6516702524068,-5.625126599063));
#28790=CARTESIAN_POINT('Ctrl Pts',(0.348469933747,-1.165204139133,-5.682001599063));
#28791=CARTESIAN_POINT('Ctrl Pts',(-0.5004819949382,-1.108444747226,-5.738876599063));
#28792=CARTESIAN_POINT('Ctrl Pts',(-1.104479823299,-0.5091721726955,-5.795751599063));
#28793=CARTESIAN_POINT('Ctrl Pts',(-1.167905052019,0.3393077836576,-5.852626599063));
#28794=CARTESIAN_POINT('Ctrl Pts',(-0.6597150647482,1.02171816845,-5.909501599063));
#28795=CARTESIAN_POINT('Ctrl Pts',(0.1713634724997,1.204062516105,-5.966376599063));
#28796=CARTESIAN_POINT('Ctrl Pts',(0.9185704929214,0.7970948701029,-6.023251599063));
#28797=CARTESIAN_POINT('Ctrl Pts',(1.216195700701,0.,-6.080126599063));
#28798=CARTESIAN_POINT('Ctrl Pts',(0.9185704929214,-0.7970948701029,-6.137001599063));
#28799=CARTESIAN_POINT('Ctrl Pts',(0.1713634724997,-1.204062516105,-6.193876599063));
#28800=CARTESIAN_POINT('Ctrl Pts',(-0.6597150647482,-1.02171816845,-6.250751599063));
#28801=CARTESIAN_POINT('Ctrl Pts',(-1.167905052019,-0.3393077836576,-6.307626599063));
#28802=CARTESIAN_POINT('Ctrl Pts',(-1.104479823299,0.5091721726955,-6.364501599063));
#28803=CARTESIAN_POINT('Ctrl Pts',(-0.5004819949382,1.108444747226,-6.421376599063));
#28804=CARTESIAN_POINT('Ctrl Pts',(0.3484699337469,1.165204139133,-6.478251599063));
#28805=CARTESIAN_POINT('Ctrl Pts',(1.026867975908,0.6516702524068,-6.535126599063));
#28806=CARTESIAN_POINT('Ctrl Pts',(1.202679571961,-0.180814804896,-6.592001599063));
#28807=CARTESIAN_POINT('Ctrl Pts',(0.7898556864549,-0.9248023542725,-6.648876599063));
#28808=CARTESIAN_POINT('Ctrl Pts',(-0.009550993186468,-1.216158607898,-6.705751599063));
#28809=CARTESIAN_POINT('Ctrl Pts',(-0.8042879589087,-0.9122802996697,-6.762626599063));
#28810=CARTESIAN_POINT('Ctrl Pts',(-1.205358893105,-0.1619074151071,-6.819501599063));
#28811=CARTESIAN_POINT('Ctrl Pts',(-1.016551442463,0.6677408946503,-6.876376599063));
#28812=CARTESIAN_POINT('Ctrl Pts',(-0.329952574922,1.170452920957,-6.933251599063));
#28813=CARTESIAN_POINT('Ctrl Pts',(0.2348081643589,1.123983684464,-6.97116826573));
#28814=CARTESIAN_POINT('Ctrl Pts',(0.4755900604755,1.010680324589,-6.990126599063));
#28815=CARTESIAN_POINT('Ctrl Pts',(0.4755900604755,-1.010680324589,-5.200042199688));
#28816=CARTESIAN_POINT('Ctrl Pts',(0.2348081643589,-1.123983684464,-5.219000533021));
#28817=CARTESIAN_POINT('Ctrl Pts',(-0.329952574922,-1.170452920957,-5.256917199688));
#28818=CARTESIAN_POINT('Ctrl Pts',(-1.016551442463,-0.6677408946504,-5.313792199688));
#28819=CARTESIAN_POINT('Ctrl Pts',(-1.205358893105,0.1619074151071,-5.370667199688));
#28820=CARTESIAN_POINT('Ctrl Pts',(-0.8042879589087,0.9122802996697,-5.427542199688));
#28821=CARTESIAN_POINT('Ctrl Pts',(-0.009550993186478,1.216158607898,-5.484417199688));
#28822=CARTESIAN_POINT('Ctrl Pts',(0.7898556864549,0.9248023542725,-5.541292199688));
#28823=CARTESIAN_POINT('Ctrl Pts',(1.202679571961,0.180814804896,-5.598167199688));
#28824=CARTESIAN_POINT('Ctrl Pts',(1.026867975908,-0.6516702524068,-5.655042199688));
#28825=CARTESIAN_POINT('Ctrl Pts',(0.348469933747,-1.165204139133,-5.711917199688));
#28826=CARTESIAN_POINT('Ctrl Pts',(-0.5004819949382,-1.108444747226,-5.768792199688));
#28827=CARTESIAN_POINT('Ctrl Pts',(-1.104479823299,-0.5091721726955,-5.825667199688));
#28828=CARTESIAN_POINT('Ctrl Pts',(-1.167905052019,0.3393077836576,-5.882542199688));
#28829=CARTESIAN_POINT('Ctrl Pts',(-0.6597150647482,1.02171816845,-5.939417199688));
#28830=CARTESIAN_POINT('Ctrl Pts',(0.1713634724997,1.204062516105,-5.996292199688));
#28831=CARTESIAN_POINT('Ctrl Pts',(0.9185704929214,0.797094870103,-6.053167199688));
#28832=CARTESIAN_POINT('Ctrl Pts',(1.216195700701,0.,-6.110042199688));
#28833=CARTESIAN_POINT('Ctrl Pts',(0.9185704929214,-0.7970948701029,-6.166917199688));
#28834=CARTESIAN_POINT('Ctrl Pts',(0.1713634724997,-1.204062516105,-6.223792199688));
#28835=CARTESIAN_POINT('Ctrl Pts',(-0.6597150647482,-1.02171816845,-6.280667199688));
#28836=CARTESIAN_POINT('Ctrl Pts',(-1.167905052019,-0.3393077836576,-6.337542199688));
#28837=CARTESIAN_POINT('Ctrl Pts',(-1.104479823299,0.5091721726955,-6.394417199688));
#28838=CARTESIAN_POINT('Ctrl Pts',(-0.5004819949382,1.108444747226,-6.451292199688));
#28839=CARTESIAN_POINT('Ctrl Pts',(0.3484699337469,1.165204139133,-6.508167199688));
#28840=CARTESIAN_POINT('Ctrl Pts',(1.026867975908,0.6516702524068,-6.565042199688));
#28841=CARTESIAN_POINT('Ctrl Pts',(1.202679571961,-0.180814804896,-6.621917199688));
#28842=CARTESIAN_POINT('Ctrl Pts',(0.7898556864549,-0.9248023542725,-6.678792199688));
#28843=CARTESIAN_POINT('Ctrl Pts',(-0.009550993186468,-1.216158607898,-6.735667199688));
#28844=CARTESIAN_POINT('Ctrl Pts',(-0.8042879589087,-0.9122802996697,-6.792542199688));
#28845=CARTESIAN_POINT('Ctrl Pts',(-1.205358893105,-0.1619074151071,-6.849417199688));
#28846=CARTESIAN_POINT('Ctrl Pts',(-1.016551442463,0.6677408946503,-6.906292199688));
#28847=CARTESIAN_POINT('Ctrl Pts',(-0.329952574922,1.170452920957,-6.963167199688));
#28848=CARTESIAN_POINT('Ctrl Pts',(0.2348081643589,1.123983684464,-7.001083866354));
#28849=CARTESIAN_POINT('Ctrl Pts',(0.4755900604755,1.010680324589,-7.020042199688));
#28850=CARTESIAN_POINT('Ctrl Pts',(0.4755900604755,-1.010680324589,-5.229957800312));
#28851=CARTESIAN_POINT('Ctrl Pts',(0.2348081643589,-1.123983684464,-5.248916133646));
#28852=CARTESIAN_POINT('Ctrl Pts',(-0.329952574922,-1.170452920957,-5.286832800312));
#28853=CARTESIAN_POINT('Ctrl Pts',(-1.016551442463,-0.6677408946504,-5.343707800312));
#28854=CARTESIAN_POINT('Ctrl Pts',(-1.205358893105,0.1619074151071,-5.400582800312));
#28855=CARTESIAN_POINT('Ctrl Pts',(-0.8042879589087,0.9122802996697,-5.457457800312));
#28856=CARTESIAN_POINT('Ctrl Pts',(-0.009550993186477,1.216158607898,-5.514332800312));
#28857=CARTESIAN_POINT('Ctrl Pts',(0.7898556864549,0.9248023542725,-5.571207800312));
#28858=CARTESIAN_POINT('Ctrl Pts',(1.202679571961,0.180814804896,-5.628082800312));
#28859=CARTESIAN_POINT('Ctrl Pts',(1.026867975908,-0.6516702524068,-5.684957800312));
#28860=CARTESIAN_POINT('Ctrl Pts',(0.348469933747,-1.165204139133,-5.741832800312));
#28861=CARTESIAN_POINT('Ctrl Pts',(-0.5004819949382,-1.108444747226,-5.798707800312));
#28862=CARTESIAN_POINT('Ctrl Pts',(-1.104479823299,-0.5091721726955,-5.855582800312));
#28863=CARTESIAN_POINT('Ctrl Pts',(-1.167905052019,0.3393077836576,-5.912457800312));
#28864=CARTESIAN_POINT('Ctrl Pts',(-0.6597150647482,1.02171816845,-5.969332800312));
#28865=CARTESIAN_POINT('Ctrl Pts',(0.1713634724997,1.204062516105,-6.026207800312));
#28866=CARTESIAN_POINT('Ctrl Pts',(0.9185704929214,0.7970948701029,-6.083082800312));
#28867=CARTESIAN_POINT('Ctrl Pts',(1.216195700701,0.,-6.139957800312));
#28868=CARTESIAN_POINT('Ctrl Pts',(0.9185704929214,-0.7970948701029,-6.196832800312));
#28869=CARTESIAN_POINT('Ctrl Pts',(0.1713634724997,-1.204062516105,-6.253707800312));
#28870=CARTESIAN_POINT('Ctrl Pts',(-0.6597150647482,-1.02171816845,-6.310582800312));
#28871=CARTESIAN_POINT('Ctrl Pts',(-1.167905052019,-0.3393077836576,-6.367457800312));
#28872=CARTESIAN_POINT('Ctrl Pts',(-1.104479823299,0.5091721726955,-6.424332800312));
#28873=CARTESIAN_POINT('Ctrl Pts',(-0.5004819949382,1.108444747226,-6.481207800312));
#28874=CARTESIAN_POINT('Ctrl Pts',(0.3484699337469,1.165204139133,-6.538082800312));
#28875=CARTESIAN_POINT('Ctrl Pts',(1.026867975908,0.6516702524068,-6.594957800312));
#28876=CARTESIAN_POINT('Ctrl Pts',(1.202679571961,-0.180814804896,-6.651832800312));
#28877=CARTESIAN_POINT('Ctrl Pts',(0.7898556864549,-0.9248023542725,-6.708707800312));
#28878=CARTESIAN_POINT('Ctrl Pts',(-0.009550993186468,-1.216158607898,-6.765582800312));
#28879=CARTESIAN_POINT('Ctrl Pts',(-0.8042879589087,-0.9122802996697,-6.822457800312));
#28880=CARTESIAN_POINT('Ctrl Pts',(-1.205358893105,-0.1619074151071,-6.879332800312));
#28881=CARTESIAN_POINT('Ctrl Pts',(-1.016551442463,0.6677408946503,-6.936207800312));
#28882=CARTESIAN_POINT('Ctrl Pts',(-0.329952574922,1.170452920957,-6.993082800312));
#28883=CARTESIAN_POINT('Ctrl Pts',(0.2348081643589,1.123983684464,-7.030999466979));
#28884=CARTESIAN_POINT('Ctrl Pts',(0.4755900604755,1.010680324589,-7.049957800312));
#28885=CARTESIAN_POINT('Ctrl Pts',(0.4755900604755,-1.010680324589,-5.259873400937));
#28886=CARTESIAN_POINT('Ctrl Pts',(0.2348081643589,-1.123983684464,-5.27883173427));
#28887=CARTESIAN_POINT('Ctrl Pts',(-0.329952574922,-1.170452920957,-5.316748400937));
#28888=CARTESIAN_POINT('Ctrl Pts',(-1.016551442463,-0.6677408946504,-5.373623400937));
#28889=CARTESIAN_POINT('Ctrl Pts',(-1.205358893105,0.1619074151071,-5.430498400937));
#28890=CARTESIAN_POINT('Ctrl Pts',(-0.8042879589087,0.9122802996697,-5.487373400937));
#28891=CARTESIAN_POINT('Ctrl Pts',(-0.009550993186477,1.216158607898,-5.544248400937));
#28892=CARTESIAN_POINT('Ctrl Pts',(0.7898556864549,0.9248023542725,-5.601123400937));
#28893=CARTESIAN_POINT('Ctrl Pts',(1.202679571961,0.180814804896,-5.657998400937));
#28894=CARTESIAN_POINT('Ctrl Pts',(1.026867975908,-0.6516702524068,-5.714873400937));
#28895=CARTESIAN_POINT('Ctrl Pts',(0.348469933747,-1.165204139133,-5.771748400937));
#28896=CARTESIAN_POINT('Ctrl Pts',(-0.5004819949382,-1.108444747226,-5.828623400937));
#28897=CARTESIAN_POINT('Ctrl Pts',(-1.104479823299,-0.5091721726955,-5.885498400937));
#28898=CARTESIAN_POINT('Ctrl Pts',(-1.167905052019,0.3393077836576,-5.942373400937));
#28899=CARTESIAN_POINT('Ctrl Pts',(-0.6597150647482,1.02171816845,-5.999248400937));
#28900=CARTESIAN_POINT('Ctrl Pts',(0.1713634724997,1.204062516105,-6.056123400937));
#28901=CARTESIAN_POINT('Ctrl Pts',(0.9185704929214,0.7970948701029,-6.112998400937));
#28902=CARTESIAN_POINT('Ctrl Pts',(1.216195700701,0.,-6.169873400937));
#28903=CARTESIAN_POINT('Ctrl Pts',(0.9185704929214,-0.7970948701029,-6.226748400937));
#28904=CARTESIAN_POINT('Ctrl Pts',(0.1713634724997,-1.204062516105,-6.283623400937));
#28905=CARTESIAN_POINT('Ctrl Pts',(-0.6597150647482,-1.02171816845,-6.340498400937));
#28906=CARTESIAN_POINT('Ctrl Pts',(-1.167905052019,-0.3393077836576,-6.397373400937));
#28907=CARTESIAN_POINT('Ctrl Pts',(-1.104479823299,0.5091721726955,-6.454248400937));
#28908=CARTESIAN_POINT('Ctrl Pts',(-0.5004819949382,1.108444747226,-6.511123400937));
#28909=CARTESIAN_POINT('Ctrl Pts',(0.3484699337469,1.165204139133,-6.567998400937));
#28910=CARTESIAN_POINT('Ctrl Pts',(1.026867975908,0.6516702524068,-6.624873400937));
#28911=CARTESIAN_POINT('Ctrl Pts',(1.202679571961,-0.180814804896,-6.681748400937));
#28912=CARTESIAN_POINT('Ctrl Pts',(0.7898556864549,-0.9248023542725,-6.738623400937));
#28913=CARTESIAN_POINT('Ctrl Pts',(-0.009550993186468,-1.216158607898,-6.795498400937));
#28914=CARTESIAN_POINT('Ctrl Pts',(-0.8042879589087,-0.9122802996697,-6.852373400937));
#28915=CARTESIAN_POINT('Ctrl Pts',(-1.205358893105,-0.1619074151071,-6.909248400937));
#28916=CARTESIAN_POINT('Ctrl Pts',(-1.016551442463,0.6677408946503,-6.966123400937));
#28917=CARTESIAN_POINT('Ctrl Pts',(-0.329952574922,1.170452920957,-7.022998400937));
#28918=CARTESIAN_POINT('Ctrl Pts',(0.2348081643589,1.123983684464,-7.060915067604));
#28919=CARTESIAN_POINT('Ctrl Pts',(0.4755900604755,1.010680324589,-7.079873400937));
#28920=CARTESIAN_POINT('Origin',(0.,0.,-7.6));
#28921=CARTESIAN_POINT('',(0.,-3.,-7.6));
#28922=CARTESIAN_POINT('Origin',(0.,0.,-7.6));
#28923=CARTESIAN_POINT('Origin',(0.,0.,-10.5));
#28924=CARTESIAN_POINT('',(0.,-3.,-8.6));
#28925=CARTESIAN_POINT('',(3.67394039744206E-16,-3.,-10.5));
#28926=CARTESIAN_POINT('',(3.,7.14126831766994E-13,-8.6));
#28927=CARTESIAN_POINT('Origin',(0.,0.,-8.6));
#28928=CARTESIAN_POINT('Origin',(0.,0.,-8.6));
#28929=CARTESIAN_POINT('Ctrl Pts',(3.00000000000014,7.14494225807769E-13,
-8.59999999999797));
#28930=CARTESIAN_POINT('Ctrl Pts',(3.00000000000014,-3.00000000000558,-8.59999999999645));
#28931=CARTESIAN_POINT('Ctrl Pts',(-6.16031515686365E-12,-3.00000000000558,
-8.59999999999894));
#28932=CARTESIAN_POINT('Ctrl Pts',(-3.00000000001246,-3.00000000000558,
-8.60000000000143));
#28933=CARTESIAN_POINT('Ctrl Pts',(-3.00000000001246,7.1449422580777E-13,
-8.60000000000295));
#28934=CARTESIAN_POINT('Ctrl Pts',(-3.00000000001246,3.00000000000701,-8.60000000000448));
#28935=CARTESIAN_POINT('Ctrl Pts',(-6.16031515686112E-12,3.00000000000701,
-8.60000000000199));
#28936=CARTESIAN_POINT('Ctrl Pts',(3.00000000000014,3.00000000000701,-8.5999999999995));
#28937=CARTESIAN_POINT('Ctrl Pts',(3.00000000000014,7.14494225807769E-13,
-8.59999999999797));
#28938=CARTESIAN_POINT('Ctrl Pts',(2.55972036857699,2.46694403342024E-15,
-10.0000000000082));
#28939=CARTESIAN_POINT('Ctrl Pts',(2.55972036857699,-2.55972036858199,-10.0000000000069));
#28940=CARTESIAN_POINT('Ctrl Pts',(-4.99935688766318E-12,-2.55972036858199,
-10.000000000009));
#28941=CARTESIAN_POINT('Ctrl Pts',(-2.55972036858699,-2.55972036858199,
-10.0000000000112));
#28942=CARTESIAN_POINT('Ctrl Pts',(-2.55972036858699,2.4669440334204E-15,
-10.0000000000125));
#28943=CARTESIAN_POINT('Ctrl Pts',(-2.55972036858699,2.55972036858199,-10.0000000000138));
#28944=CARTESIAN_POINT('Ctrl Pts',(-4.99935688766102E-12,2.55972036858199,
-10.0000000000116));
#28945=CARTESIAN_POINT('Ctrl Pts',(2.55972036857699,2.55972036858199,-10.0000000000095));
#28946=CARTESIAN_POINT('Ctrl Pts',(2.55972036857699,2.46694403342024E-15,
-10.0000000000082));
#28947=CARTESIAN_POINT('Ctrl Pts',(1.09212159715655,2.46694403834357E-15,
-9.99999999999975));
#28948=CARTESIAN_POINT('Ctrl Pts',(1.09212159715655,-1.09212159716155,-9.9999999999992));
#28949=CARTESIAN_POINT('Ctrl Pts',(-4.99935688767059E-12,-1.09212159716155,
-10.0000000000001));
#28950=CARTESIAN_POINT('Ctrl Pts',(-1.09212159716655,-1.09212159716155,
-10.000000000001));
#28951=CARTESIAN_POINT('Ctrl Pts',(-1.09212159716655,2.46694403834408E-15,
-10.0000000000016));
#28952=CARTESIAN_POINT('Ctrl Pts',(-1.09212159716655,1.09212159716156,-10.0000000000021));
#28953=CARTESIAN_POINT('Ctrl Pts',(-4.99935688766966E-12,1.09212159716156,
-10.0000000000012));
#28954=CARTESIAN_POINT('Ctrl Pts',(1.09212159715655,1.09212159716156,-10.0000000000003));
#28955=CARTESIAN_POINT('Ctrl Pts',(1.09212159715655,2.46694403834357E-15,
-9.99999999999975));
#28956=CARTESIAN_POINT('',(-0.2485901447084,-1.397638819231,-9.973011580318));
#28957=CARTESIAN_POINT('',(0.2485901447084,-1.397638819231,-9.973011580318));
#28958=CARTESIAN_POINT('Ctrl Pts',(0.24859014470844,-1.39763881923147,-9.97301158031942));
#28959=CARTESIAN_POINT('Ctrl Pts',(0.163988452831422,-1.39785090473685,
-9.97543572873859));
#28960=CARTESIAN_POINT('Ctrl Pts',(0.0808409165723131,-1.39794227815784,
-9.97648013171962));
#28961=CARTESIAN_POINT('Ctrl Pts',(-0.0808409165790198,-1.39794227815785,
-9.97648013171975));
#28962=CARTESIAN_POINT('Ctrl Pts',(-0.163988452834823,-1.39785090473688,
-9.97543572873894));
#28963=CARTESIAN_POINT('Ctrl Pts',(-0.24859014470846,-1.39763881923153,
-9.97301158032012));
#28964=CARTESIAN_POINT('',(0.4994251259956,-1.150376451473,-9.993429160062));
#28965=CARTESIAN_POINT('Ctrl Pts',(0.248590144708445,-1.39763881923184,
-9.97301158031936));
#28966=CARTESIAN_POINT('Ctrl Pts',(0.266345257726262,-1.39759430945868,
-9.97250283128374));
#28967=CARTESIAN_POINT('Ctrl Pts',(0.284094629964267,-1.39567756906844,
-9.97224058239354));
#28968=CARTESIAN_POINT('Ctrl Pts',(0.301536754642562,-1.39189823089679,
-9.97224070208607));
#28969=CARTESIAN_POINT('Ctrl Pts',(0.310675342511096,-1.38991809289162,
-9.9722407647975));
#28970=CARTESIAN_POINT('Ctrl Pts',(0.319697231577847,-1.38743358849169,
-9.9723125850535));
#28971=CARTESIAN_POINT('Ctrl Pts',(0.360053184989107,-1.37387856724409,
-9.97296163608247));
#28972=CARTESIAN_POINT('Ctrl Pts',(0.389149980282598,-1.35721565994091,
-9.97436868233086));
#28973=CARTESIAN_POINT('Ctrl Pts',(0.438990275319011,-1.31376842357764,
-9.97850849048035));
#28974=CARTESIAN_POINT('Ctrl Pts',(0.459310846586711,-1.28745433645393,
-9.98118840839364));
#28975=CARTESIAN_POINT('Ctrl Pts',(0.488183202022476,-1.2290475577898,-9.98684098470683));
#28976=CARTESIAN_POINT('Ctrl Pts',(0.496681676024958,-1.19763175363616,
-9.98974371060822));
#28977=CARTESIAN_POINT('Ctrl Pts',(0.499206546933211,-1.16041155214929,
-9.99267187288286));
#28978=CARTESIAN_POINT('Ctrl Pts',(0.49939251014142,-1.15539199227997,-9.99305635913868));
#28979=CARTESIAN_POINT('Ctrl Pts',(0.499425125995968,-1.15037645147301,
-9.99342916006207));
#28980=CARTESIAN_POINT('',(0.5,-0.9709426260066,-10.));
#28981=CARTESIAN_POINT('Ctrl Pts',(0.499425125995589,-1.15037645147301,
-9.99342916006209));
#28982=CARTESIAN_POINT('Ctrl Pts',(0.499823732040743,-1.08908034523772,
-9.99798524800639));
#28983=CARTESIAN_POINT('Ctrl Pts',(0.499999999999975,-1.02886065465466,
-9.99999999999972));
#28984=CARTESIAN_POINT('Ctrl Pts',(0.499999999999978,-0.970942626013781,
-9.99999999999975));
#28985=CARTESIAN_POINT('',(0.9709426260066,-0.5,-10.));
#28986=CARTESIAN_POINT('Origin',(0.,0.,-10.));
#28987=CARTESIAN_POINT('',(1.150376451473,-0.4994251259956,-9.993429160062));
#28988=CARTESIAN_POINT('Ctrl Pts',(0.970942626011364,-0.499999999999965,
-9.99999999999959));
#28989=CARTESIAN_POINT('Ctrl Pts',(1.02886065465299,-0.49999999999997,-9.99999999999966));
#28990=CARTESIAN_POINT('Ctrl Pts',(1.08908034523686,-0.49982373204072,-9.99798524800613));
#28991=CARTESIAN_POINT('Ctrl Pts',(1.15037645147297,-0.499425125995553,
-9.99342916006167));
#28992=CARTESIAN_POINT('',(1.397638819231,-0.2485901447084,-9.973011580318));
#28993=CARTESIAN_POINT('Ctrl Pts',(1.15037645147297,-0.499425125995932,
-9.99342916006166));
#28994=CARTESIAN_POINT('Ctrl Pts',(1.16585150547838,-0.4993244923594,-9.99227891233267));
#28995=CARTESIAN_POINT('Ctrl Pts',(1.1813119375003,-0.497764366616508,-9.99102091698527));
#28996=CARTESIAN_POINT('Ctrl Pts',(1.22820384051413,-0.488479515534905,
-9.98696801305249));
#28997=CARTESIAN_POINT('Ctrl Pts',(1.2582878105144,-0.476056452234761,-9.98403403393921));
#28998=CARTESIAN_POINT('Ctrl Pts',(1.3120898695489,-0.440364616164326,-9.9787167926228));
#28999=CARTESIAN_POINT('Ctrl Pts',(1.33530269455742,-0.417419016315832,
-9.97639129073107));
#29000=CARTESIAN_POINT('Ctrl Pts',(1.37195593643593,-0.363749347026123,
-9.97313064215981));
#29001=CARTESIAN_POINT('Ctrl Pts',(1.38498091076259,-0.333461063805117,
-9.97224092115826));
#29002=CARTESIAN_POINT('Ctrl Pts',(1.39189823089696,-0.301536754641286,
-9.97224070208509));
#29003=CARTESIAN_POINT('Ctrl Pts',(1.39413558307741,-0.291211090752747,
-9.97224063122762));
#29004=CARTESIAN_POINT('Ctrl Pts',(1.39572483998331,-0.280755792323049,
-9.97233220873014));
#29005=CARTESIAN_POINT('Ctrl Pts',(1.39729372860019,-0.263023020533822,
-9.97263847784447));
#29006=CARTESIAN_POINT('Ctrl Pts',(1.39762074000317,-0.255802015808498,
-9.9728049337899));
#29007=CARTESIAN_POINT('Ctrl Pts',(1.39763881923175,-0.248590144708412,
-9.97301158031834));
#29008=CARTESIAN_POINT('',(1.39794229184068,1.42576569662847E-14,-9.97648028811549));
#29009=CARTESIAN_POINT('Origin',(1.39225353644748,-1.10267882883625E-6,
-9.91145751650082));
#29010=CARTESIAN_POINT('Ctrl Pts',(1.39794226787512,1.44289345718086E-14,
-9.97648013330951));
#29011=CARTESIAN_POINT('Ctrl Pts',(2.62691944453891,1.11142367514289E-13,
-9.78632055714307));
#29012=CARTESIAN_POINT('Ctrl Pts',(3.00000000000014,7.14494225807769E-13,
-8.59999999999797));
#29013=CARTESIAN_POINT('',(1.397638819231,0.2485901447084,-9.973011580318));
#29014=CARTESIAN_POINT('Origin',(1.39225353644748,-1.10267882883625E-6,
-9.91145751650082));
#29015=CARTESIAN_POINT('',(1.150376451473,0.4994251259956,-9.993429160062));
#29016=CARTESIAN_POINT('Ctrl Pts',(1.39763881923178,0.248590144708423,-9.97301158031859));
#29017=CARTESIAN_POINT('Ctrl Pts',(1.39759430945861,0.266345257725831,-9.972502831283));
#29018=CARTESIAN_POINT('Ctrl Pts',(1.39567756906846,0.284094629963428,-9.97224058239284));
#29019=CARTESIAN_POINT('Ctrl Pts',(1.39189823089698,0.301536754641337,-9.97224070208539));
#29020=CARTESIAN_POINT('Ctrl Pts',(1.38991809289194,0.310675342509477,-9.97224076479684));
#29021=CARTESIAN_POINT('Ctrl Pts',(1.38743358849219,0.319697231575848,-9.97231258505284));
#29022=CARTESIAN_POINT('Ctrl Pts',(1.3738785672451,0.360053184986904,-9.97296163608185));
#29023=CARTESIAN_POINT('Ctrl Pts',(1.35721565994219,0.38914998028057,-9.97436868233028));
#29024=CARTESIAN_POINT('Ctrl Pts',(1.31376842357938,0.438990275317438,-9.97850849047988));
#29025=CARTESIAN_POINT('Ctrl Pts',(1.28745433645583,0.459310846585399,-9.98118840839324));
#29026=CARTESIAN_POINT('Ctrl Pts',(1.22904755779197,0.488183202021726,-9.98684098470657));
#29027=CARTESIAN_POINT('Ctrl Pts',(1.1976317536384,0.49668167602451,-9.98974371060802));
#29028=CARTESIAN_POINT('Ctrl Pts',(1.1604115521508,0.499206546933161,-9.99267187288281));
#29029=CARTESIAN_POINT('Ctrl Pts',(1.15539199228073,0.499392510141422,-9.99305635913871));
#29030=CARTESIAN_POINT('Ctrl Pts',(1.15037645147301,0.499425125995976,-9.99342916006216));
#29031=CARTESIAN_POINT('',(0.9709426260066,0.5,-10.));
#29032=CARTESIAN_POINT('Ctrl Pts',(1.15037645147301,0.499425125995597,-9.99342916006217));
#29033=CARTESIAN_POINT('Ctrl Pts',(1.08908034523688,0.499823732040765,-9.99798524800664));
#29034=CARTESIAN_POINT('Ctrl Pts',(1.02886065465299,0.500000000000005,-10.0000000000001));
#29035=CARTESIAN_POINT('Ctrl Pts',(0.970942626011344,0.500000000000009,
-10.0000000000001));
#29036=CARTESIAN_POINT('',(0.5,0.9709426260066,-10.));
#29037=CARTESIAN_POINT('Origin',(0.,0.,-10.));
#29038=CARTESIAN_POINT('',(0.4994251259956,1.150376451473,-9.993429160062));
#29039=CARTESIAN_POINT('Ctrl Pts',(0.500000000000065,0.970942626013742,
-10.0000000000007));
#29040=CARTESIAN_POINT('Ctrl Pts',(0.500000000000081,1.02886065465465,-10.0000000000009));
#29041=CARTESIAN_POINT('Ctrl Pts',(0.499823732040839,1.08908034523776,-9.99798524800749));
#29042=CARTESIAN_POINT('Ctrl Pts',(0.499425125995691,1.15037645147309,-9.99342916006325));
#29043=CARTESIAN_POINT('',(0.2485901447084,1.397638819231,-9.973011580318));
#29044=CARTESIAN_POINT('Ctrl Pts',(0.49942512599607,1.15037645147309,-9.99342916006323));
#29045=CARTESIAN_POINT('Ctrl Pts',(0.499324492359546,1.1658515054781,-9.99227891233432));
#29046=CARTESIAN_POINT('Ctrl Pts',(0.497764366616736,1.18131193749962,-9.99102091698699));
#29047=CARTESIAN_POINT('Ctrl Pts',(0.48847951553546,1.2282038405131,-9.98696801305439));
#29048=CARTESIAN_POINT('Ctrl Pts',(0.476056452235479,1.25828781051344,-9.9840340339412));
#29049=CARTESIAN_POINT('Ctrl Pts',(0.440364616165319,1.31208986954814,-9.97871679262494));
#29050=CARTESIAN_POINT('Ctrl Pts',(0.417419016316943,1.33530269455678,-9.97639129073328));
#29051=CARTESIAN_POINT('Ctrl Pts',(0.363749347027429,1.37195593643556,-9.97313064216213));
#29052=CARTESIAN_POINT('Ctrl Pts',(0.333461063806484,1.38498091076238,-9.97224092116061));
#29053=CARTESIAN_POINT('Ctrl Pts',(0.30153675464268,1.39189823089692,-9.97224070208747));
#29054=CARTESIAN_POINT('Ctrl Pts',(0.291211090753734,1.3941355830775,-9.97224063123));
#29055=CARTESIAN_POINT('Ctrl Pts',(0.280755792323659,1.39572483998349,-9.97233220873254));
#29056=CARTESIAN_POINT('Ctrl Pts',(0.263023020533999,1.39729372860041,-9.97263847784689));
#29057=CARTESIAN_POINT('Ctrl Pts',(0.255802015808621,1.39762074000339,-9.97280493379232));
#29058=CARTESIAN_POINT('Ctrl Pts',(0.248590144708482,1.39763881923197,-9.97301158032077));
#29059=CARTESIAN_POINT('',(-0.2485901447084,1.397638819231,-9.973011580318));
#29060=CARTESIAN_POINT('Ctrl Pts',(0.24859014470848,1.39763881923159,-9.97301158032083));
#29061=CARTESIAN_POINT('Ctrl Pts',(0.163988452831448,1.39785090473697,-9.97543572874));
#29062=CARTESIAN_POINT('Ctrl Pts',(0.080840916572326,1.39794227815797,-9.97648013172102));
#29063=CARTESIAN_POINT('Ctrl Pts',(-0.0808409165790325,1.39794227815798,
-9.97648013172116));
#29064=CARTESIAN_POINT('Ctrl Pts',(-0.163988452834849,1.397850904737,-9.97543572874035));
#29065=CARTESIAN_POINT('Ctrl Pts',(-0.248590144708499,1.39763881923165,
-9.97301158032152));
#29066=CARTESIAN_POINT('',(-0.4994251259956,1.150376451473,-9.993429160062));
#29067=CARTESIAN_POINT('Ctrl Pts',(-0.248590144708506,1.39763881923203,
-9.97301158032146));
#29068=CARTESIAN_POINT('Ctrl Pts',(-0.266345257725687,1.39759430945888,
-9.9725028312859));
#29069=CARTESIAN_POINT('Ctrl Pts',(-0.284094629963059,1.39567756906879,
-9.97224058239576));
#29070=CARTESIAN_POINT('Ctrl Pts',(-0.301536754640759,1.39189823089742,
-9.97224070208831));
#29071=CARTESIAN_POINT('Ctrl Pts',(-0.310675342509529,1.38991809289227,
-9.97224076479976));
#29072=CARTESIAN_POINT('Ctrl Pts',(-0.319697231576514,1.38743358849235,
-9.97231258505576));
#29073=CARTESIAN_POINT('Ctrl Pts',(-0.360053184988087,1.3738785672449,-9.97296163608481));
#29074=CARTESIAN_POINT('Ctrl Pts',(-0.389149980281671,1.35721565994188,
-9.97436868233322));
#29075=CARTESIAN_POINT('Ctrl Pts',(-0.438990275318315,1.3137684235789,-9.97850849048274));
#29076=CARTESIAN_POINT('Ctrl Pts',(-0.459310846586145,1.28745433645531,
-9.98118840839603));
#29077=CARTESIAN_POINT('Ctrl Pts',(-0.488183202022219,1.22904755779138,
-9.98684098470917));
#29078=CARTESIAN_POINT('Ctrl Pts',(-0.496681676024877,1.19763175363781,
-9.9897437106105));
#29079=CARTESIAN_POINT('Ctrl Pts',(-0.499206546933379,1.16041155215047,
-9.99267187288511));
#29080=CARTESIAN_POINT('Ctrl Pts',(-0.49939251014162,1.15539199228065,-9.99305635914096));
#29081=CARTESIAN_POINT('Ctrl Pts',(-0.49942512599617,1.15037645147318,-9.99342916006438));
#29082=CARTESIAN_POINT('',(-0.5,0.9709426260066,-10.));
#29083=CARTESIAN_POINT('Ctrl Pts',(-0.499425125995791,1.15037645147318,
-9.99342916006439));
#29084=CARTESIAN_POINT('Ctrl Pts',(-0.49982373204092,1.08908034523958,-9.99798524800841));
#29085=CARTESIAN_POINT('Ctrl Pts',(-0.500000000000139,1.02886065465818,
-10.0000000000016));
#29086=CARTESIAN_POINT('Ctrl Pts',(-0.500000000000137,0.970942626018854,
-10.0000000000016));
#29087=CARTESIAN_POINT('',(-0.9709426260066,0.5,-10.));
#29088=CARTESIAN_POINT('Origin',(0.,0.,-10.));
#29089=CARTESIAN_POINT('',(-1.150376451473,0.4994251259956,-9.993429160062));
#29090=CARTESIAN_POINT('Ctrl Pts',(-0.97094262602127,0.50000000000015,-10.0000000000017));
#29091=CARTESIAN_POINT('Ctrl Pts',(-1.02886065465985,0.500000000000184,
-10.0000000000021));
#29092=CARTESIAN_POINT('Ctrl Pts',(-1.08908034524044,0.499823732040942,
-9.99798524800866));
#29093=CARTESIAN_POINT('Ctrl Pts',(-1.15037645147321,0.499425125995827,
-9.99342916006481));
#29094=CARTESIAN_POINT('',(-1.397638819231,0.2485901447084,-9.973011580318));
#29095=CARTESIAN_POINT('Ctrl Pts',(-1.1503764514732,0.499425125996206,-9.99342916006479));
#29096=CARTESIAN_POINT('Ctrl Pts',(-1.16585150547846,0.499324492359686,
-9.99227891233591));
#29097=CARTESIAN_POINT('Ctrl Pts',(-1.18131193750023,0.497764366616836,
-9.9910209169886));
#29098=CARTESIAN_POINT('Ctrl Pts',(-1.22820384051396,0.488479515535382,
-9.9869680130561));
#29099=CARTESIAN_POINT('Ctrl Pts',(-1.25828781051428,0.476056452235305,
-9.98403403394297));
#29100=CARTESIAN_POINT('Ctrl Pts',(-1.31208986954888,0.440364616164987,
-9.9787167926268));
#29101=CARTESIAN_POINT('Ctrl Pts',(-1.33530269455747,0.417419016316536,
-9.97639129073516));
#29102=CARTESIAN_POINT('Ctrl Pts',(-1.3719559364361,0.363749347026876,-9.97313064216401));
#29103=CARTESIAN_POINT('Ctrl Pts',(-1.38498091076282,0.333461063805877,
-9.97224092116247));
#29104=CARTESIAN_POINT('Ctrl Pts',(-1.39189823089725,0.301536754642035,
-9.97224070208929));
#29105=CARTESIAN_POINT('Ctrl Pts',(-1.39413558307793,0.29121109075249,-9.97224063123181));
#29106=CARTESIAN_POINT('Ctrl Pts',(-1.39572483998393,0.280755792321815,
-9.97233220873434));
#29107=CARTESIAN_POINT('Ctrl Pts',(-1.39729372860064,0.263023020532381,
-9.97263847784868));
#29108=CARTESIAN_POINT('Ctrl Pts',(-1.39762074000354,0.255802015807838,
-9.97280493379408));
#29109=CARTESIAN_POINT('Ctrl Pts',(-1.39763881923212,0.248590144708531,
-9.97301158032249));
#29110=CARTESIAN_POINT('',(-1.397638819231,-0.2485901447085,-9.973011580318));
#29111=CARTESIAN_POINT('Origin',(-1.39225353644736,1.10267764200783E-6,
-9.91145751649949));
#29112=CARTESIAN_POINT('',(-1.150376451473,-0.4994251259956,-9.993429160062));
#29113=CARTESIAN_POINT('Ctrl Pts',(-1.3976388192321,-0.248590144708628,
-9.97301158032223));
#29114=CARTESIAN_POINT('Ctrl Pts',(-1.39759430945894,-0.266345257726185,
-9.97250283128663));
#29115=CARTESIAN_POINT('Ctrl Pts',(-1.39567756906876,-0.284094629963931,
-9.97224058239646));
#29116=CARTESIAN_POINT('Ctrl Pts',(-1.39189823089723,-0.301536754641984,
-9.97224070208898));
#29117=CARTESIAN_POINT('Ctrl Pts',(-1.38991809289195,-0.310675342511139,
-9.97224076480042));
#29118=CARTESIAN_POINT('Ctrl Pts',(-1.38743358849185,-0.319697231578498,
-9.97231258505642));
#29119=CARTESIAN_POINT('Ctrl Pts',(-1.37387856724389,-0.360053184990289,
-9.97296163608543));
#29120=CARTESIAN_POINT('Ctrl Pts',(-1.3572156599406,-0.389149980283697,
-9.9743686823338));
#29121=CARTESIAN_POINT('Ctrl Pts',(-1.31376842357717,-0.438990275319886,
-9.97850849048321));
#29122=CARTESIAN_POINT('Ctrl Pts',(-1.2874543364534,-0.459310846587456,
-9.98118840839643));
#29123=CARTESIAN_POINT('Ctrl Pts',(-1.22904755778921,-0.488183202022969,
-9.98684098470943));
#29124=CARTESIAN_POINT('Ctrl Pts',(-1.19763175363558,-0.496681676025323,
-9.98974371061069));
#29125=CARTESIAN_POINT('Ctrl Pts',(-1.16041155214897,-0.499206546933428,
-9.99267187288515));
#29126=CARTESIAN_POINT('Ctrl Pts',(-1.15539199227989,-0.499392510141618,
-9.99305635914094));
#29127=CARTESIAN_POINT('Ctrl Pts',(-1.15037645147317,-0.499425125996162,
-9.99342916006429));
#29128=CARTESIAN_POINT('',(-0.9709426260066,-0.5,-10.));
#29129=CARTESIAN_POINT('Ctrl Pts',(-1.15037645147317,-0.499425125995783,
-9.9934291600643));
#29130=CARTESIAN_POINT('Ctrl Pts',(-1.08908034524041,-0.499823732040897,
-9.99798524800816));
#29131=CARTESIAN_POINT('Ctrl Pts',(-1.02886065465985,-0.50000000000011,
-10.0000000000013));
#29132=CARTESIAN_POINT('Ctrl Pts',(-0.970942626021291,-0.500000000000106,
-10.0000000000012));
#29133=CARTESIAN_POINT('',(-0.5,-0.9709426260066,-10.));
#29134=CARTESIAN_POINT('Origin',(0.,0.,-10.));
#29135=CARTESIAN_POINT('',(-0.4994251259956,-1.150376451473,-9.993429160062));
#29136=CARTESIAN_POINT('Ctrl Pts',(-0.500000000000051,-0.970942626018893,
-10.0000000000006));
#29137=CARTESIAN_POINT('Ctrl Pts',(-0.500000000000073,-1.02886065465818,
-10.0000000000008));
#29138=CARTESIAN_POINT('Ctrl Pts',(-0.499823732040823,-1.08908034523954,
-9.99798524800731));
#29139=CARTESIAN_POINT('Ctrl Pts',(-0.499425125995689,-1.15037645147309,
-9.99342916006323));
#29140=CARTESIAN_POINT('Ctrl Pts',(-0.499425125996068,-1.15037645147309,
-9.99342916006322));
#29141=CARTESIAN_POINT('Ctrl Pts',(-0.49932449235954,-1.16585150547875,
-9.99227891233426));
#29142=CARTESIAN_POINT('Ctrl Pts',(-0.497764366616606,-1.18131193750091,
-9.99102091698688));
#29143=CARTESIAN_POINT('Ctrl Pts',(-0.488479515534827,-1.22820384051498,
-9.9869680130542));
#29144=CARTESIAN_POINT('Ctrl Pts',(-0.476056452234594,-1.25828781051522,
-9.98403403394099));
#29145=CARTESIAN_POINT('Ctrl Pts',(-0.440364616163992,-1.31208986954964,
-9.97871679262466));
#29146=CARTESIAN_POINT('Ctrl Pts',(-0.417419016315419,-1.33530269455811,
-9.97639129073295));
#29147=CARTESIAN_POINT('Ctrl Pts',(-0.363749347025575,-1.37195593643646,
-9.97313064216169));
#29148=CARTESIAN_POINT('Ctrl Pts',(-0.333461063804512,-1.38498091076303,
-9.97224092116012));
#29149=CARTESIAN_POINT('Ctrl Pts',(-0.301536754640641,-1.3918982308973,
-9.97224070208691));
#29150=CARTESIAN_POINT('Ctrl Pts',(-0.291211090751498,-1.39413558307784,
-9.97224063122943));
#29151=CARTESIAN_POINT('Ctrl Pts',(-0.280755792321202,-1.39572483998376,
-9.97233220873195));
#29152=CARTESIAN_POINT('Ctrl Pts',(-0.263023020532205,-1.39729372860043,
-9.97263847784626));
#29153=CARTESIAN_POINT('Ctrl Pts',(-0.255802015807715,-1.39762074000333,
-9.97280493379166));
#29154=CARTESIAN_POINT('Ctrl Pts',(-0.248590144708461,-1.39763881923191,
-9.97301158032005));
#29155=CARTESIAN_POINT('Origin',(1.4,0.6599764278095,-10.));
#29156=CARTESIAN_POINT('',(1.268767004711,-0.1197183301882,-8.5));
#29157=CARTESIAN_POINT('',(1.397638819231,-0.2485901447084,-9.973011580318));
#29158=CARTESIAN_POINT('',(1.268767004711,0.1197183301882,-8.5));
#29159=CARTESIAN_POINT('',(1.268767004711,0.1197183301882,-8.5));
#29160=CARTESIAN_POINT('',(1.397638819231,0.2485901447084,-9.973011580318));
#29161=CARTESIAN_POINT('Origin',(2.321412939997,-1.421412939997,-23.40022640802));
#29162=CARTESIAN_POINT('',(1.019718330188,-0.3687670047111,-8.5));
#29163=CARTESIAN_POINT('Origin',(1.01781204532566,-0.117812045325658,-8.5));
#29164=CARTESIAN_POINT('',(1.150376451473,-0.4994251259956,-9.993429160062));
#29165=CARTESIAN_POINT('Origin',(0.,0.,-8.5));
#29166=CARTESIAN_POINT('',(-0.3687670047111,0.617815679234,-8.5));
#29167=CARTESIAN_POINT('',(-0.3687670047111,1.019718330188,-8.5));
#29168=CARTESIAN_POINT('',(-0.3687670047111,0.617815679234,-8.5));
#29169=CARTESIAN_POINT('',(-0.1197183301882,1.268767004711,-8.5));
#29170=CARTESIAN_POINT('Origin',(-0.117812045325658,1.01781204532566,-8.5));
#29171=CARTESIAN_POINT('',(0.1197183301882,1.268767004711,-8.5));
#29172=CARTESIAN_POINT('',(-0.1197183301882,1.268767004711,-8.5));
#29173=CARTESIAN_POINT('',(0.3687670047111,1.019718330188,-8.5));
#29174=CARTESIAN_POINT('Origin',(0.117812045325658,1.01781204532566,-8.5));
#29175=CARTESIAN_POINT('',(0.3687670047111,0.617815679234,-8.5));
#29176=CARTESIAN_POINT('',(0.3687670047111,1.019718330188,-8.5));
#29177=CARTESIAN_POINT('',(0.617815679234,0.3687670047111,-8.5));
#29178=CARTESIAN_POINT('Origin',(0.619721964096652,0.619721964096652,-8.5));
#29179=CARTESIAN_POINT('',(1.019718330188,0.3687670047111,-8.5));
#29180=CARTESIAN_POINT('',(0.617815679234,0.3687670047111,-8.5));
#29181=CARTESIAN_POINT('Origin',(1.01781204532566,0.117812045325658,-8.5));
#29182=CARTESIAN_POINT('',(0.6178156792341,-0.3687670047111,-8.5));
#29183=CARTESIAN_POINT('',(1.019718330188,-0.3687670047111,-8.5));
#29184=CARTESIAN_POINT('',(0.3687670047111,-0.6178156792341,-8.5));
#29185=CARTESIAN_POINT('Origin',(0.619721964096385,-0.619721964096385,-8.5));
#29186=CARTESIAN_POINT('',(0.3687670047111,-1.019718330188,-8.5));
#29187=CARTESIAN_POINT('',(0.3687670047111,-0.6178156792341,-8.5));
#29188=CARTESIAN_POINT('',(0.1197183301882,-1.268767004711,-8.5));
#29189=CARTESIAN_POINT('Origin',(0.117812045325658,-1.01781204532566,-8.5));
#29190=CARTESIAN_POINT('',(-0.1197183301882,-1.268767004711,-8.5));
#29191=CARTESIAN_POINT('',(0.1197183301882,-1.268767004711,-8.5));
#29192=CARTESIAN_POINT('',(-0.3687670047111,-1.019718330188,-8.5));
#29193=CARTESIAN_POINT('Origin',(-0.117812045325658,-1.01781204532566,-8.5));
#29194=CARTESIAN_POINT('',(-0.3687670047111,-0.6178156792341,-8.5));
#29195=CARTESIAN_POINT('',(-0.3687670047111,-1.019718330188,-8.5));
#29196=CARTESIAN_POINT('',(-0.6178156792341,-0.3687670047111,-8.5));
#29197=CARTESIAN_POINT('Origin',(-0.619721964096385,-0.619721964096385,
-8.5));
#29198=CARTESIAN_POINT('',(-1.019718330188,-0.3687670047111,-8.5));
#29199=CARTESIAN_POINT('',(-0.6178156792341,-0.3687670047111,-8.5));
#29200=CARTESIAN_POINT('',(-1.268767004711,-0.1197183301882,-8.5));
#29201=CARTESIAN_POINT('Origin',(-1.01781204532566,-0.117812045325658,-8.5));
#29202=CARTESIAN_POINT('',(-1.268767004711,0.1197183301882,-8.5));
#29203=CARTESIAN_POINT('',(-1.268767004711,-0.1197183301882,-8.5));
#29204=CARTESIAN_POINT('',(-1.019718330188,0.3687670047111,-8.5));
#29205=CARTESIAN_POINT('Origin',(-1.01781204532566,0.117812045325658,-8.5));
#29206=CARTESIAN_POINT('',(-0.6178156792341,0.3687670047111,-8.5));
#29207=CARTESIAN_POINT('',(-1.019718330188,0.3687670047111,-8.5));
#29208=CARTESIAN_POINT('Origin',(-0.619721964096385,0.619721964096385,-8.5));
#29209=CARTESIAN_POINT('Origin',(-0.5,0.3400235721905,-10.));
#29210=CARTESIAN_POINT('',(-0.5,0.7490486745229,-10.));
#29211=CARTESIAN_POINT('',(-0.5,0.7490486745229,-10.));
#29212=CARTESIAN_POINT('',(-0.4994251259956,1.150376451473,-9.993429160062));
#29213=CARTESIAN_POINT('',(-0.3687670047111,0.617815679234,-8.5));
#29214=CARTESIAN_POINT('Origin',(0.,0.,-10.));
#29215=CARTESIAN_POINT('',(0.5,0.7490486745229,-10.));
#29216=CARTESIAN_POINT('',(0.5,0.9709426260066,-10.));
#29217=CARTESIAN_POINT('',(0.7490486745229,0.5,-10.));
#29218=CARTESIAN_POINT('',(0.7490486745229,0.5,-10.));
#29219=CARTESIAN_POINT('Origin',(0.750954959385537,0.750954959385537,-10.));
#29220=CARTESIAN_POINT('Origin',(0.,0.,-10.));
#29221=CARTESIAN_POINT('',(0.7490486745229,-0.5,-10.));
#29222=CARTESIAN_POINT('',(0.9709426260066,-0.5,-10.));
#29223=CARTESIAN_POINT('',(0.5,-0.7490486745229,-10.));
#29224=CARTESIAN_POINT('',(0.5,-0.7490486745229,-10.));
#29225=CARTESIAN_POINT('Origin',(0.75095495938527,-0.75095495938527,-10.));
#29226=CARTESIAN_POINT('Origin',(0.,0.,-10.));
#29227=CARTESIAN_POINT('',(-0.5,-0.7490486745229,-10.));
#29228=CARTESIAN_POINT('',(-0.5,-0.9709426260066,-10.));
#29229=CARTESIAN_POINT('',(-0.7490486745229,-0.5,-10.));
#29230=CARTESIAN_POINT('',(-0.7490486745229,-0.5,-10.));
#29231=CARTESIAN_POINT('Origin',(-0.75095495938527,-0.75095495938527,-10.));
#29232=CARTESIAN_POINT('Origin',(0.,0.,-10.));
#29233=CARTESIAN_POINT('',(-0.7490486745229,0.5,-10.));
#29234=CARTESIAN_POINT('',(-0.9709426260066,0.5,-10.));
#29235=CARTESIAN_POINT('Origin',(-0.75095495938527,0.75095495938527,-10.));
#29236=CARTESIAN_POINT('Origin',(0.5,1.559976427809,-10.));
#29237=CARTESIAN_POINT('',(0.3687670047111,0.617815679234,-8.5));
#29238=CARTESIAN_POINT('',(0.4994251259956,1.150376451473,-9.993429160062));
#29239=CARTESIAN_POINT('Origin',(1.421412939997,2.321412939997,-23.40022640802));
#29240=CARTESIAN_POINT('',(0.2485901447084,1.397638819231,-9.973011580318));
#29241=CARTESIAN_POINT('Origin',(-0.6599764278095,1.4,-10.));
#29242=CARTESIAN_POINT('',(-0.2485901447084,1.397638819231,-9.973011580318));
#29243=CARTESIAN_POINT('Origin',(-1.421412939997,2.321412939997,-23.40022640802));
#29244=CARTESIAN_POINT('Origin',(-1.4,-0.6599764278095,-10.));
#29245=CARTESIAN_POINT('',(-1.397638819231,0.2485901447084,-9.973011580318));
#29246=CARTESIAN_POINT('',(-1.397638819231,-0.2485901447085,-9.973011580318));
#29247=CARTESIAN_POINT('Origin',(-2.321412939997,1.421412939997,-23.40022640802));
#29248=CARTESIAN_POINT('',(-1.150376451473,0.4994251259956,-9.993429160062));
#29249=CARTESIAN_POINT('Origin',(-1.559976427809,0.5,-10.));
#29250=CARTESIAN_POINT('',(-0.6178156792341,0.3687670047111,-8.5));
#29251=CARTESIAN_POINT('Origin',(1.320743945967,-1.320743945967,13.67962684375));
#29252=CARTESIAN_POINT('Origin',(-2.321412939997,-1.421412939997,-23.40022640802));
#29253=CARTESIAN_POINT('',(-1.150376451473,-0.4994251259956,-9.993429160062));
#29254=CARTESIAN_POINT('Origin',(-0.3400235721905,-0.5,-10.));
#29255=CARTESIAN_POINT('',(-0.6178156792341,-0.3687670047111,-8.5));
#29256=CARTESIAN_POINT('Origin',(1.320743945967,1.320743945967,13.67962684375));
#29257=CARTESIAN_POINT('',(-0.3687670047111,-0.6178156792341,-8.5));
#29258=CARTESIAN_POINT('Origin',(-0.5,-1.559976427809,-10.));
#29259=CARTESIAN_POINT('',(-0.4994251259956,-1.150376451473,-9.993429160062));
#29260=CARTESIAN_POINT('Origin',(-1.421412939997,-2.321412939997,-23.40022640802));
#29261=CARTESIAN_POINT('',(-0.2485901447084,-1.397638819231,-9.973011580318));
#29262=CARTESIAN_POINT('Origin',(0.6599764278095,-1.4,-10.));
#29263=CARTESIAN_POINT('',(0.2485901447084,-1.397638819231,-9.973011580318));
#29264=CARTESIAN_POINT('Origin',(1.421412939997,-2.321412939997,-23.40022640802));
#29265=CARTESIAN_POINT('',(0.4994251259956,-1.150376451473,-9.993429160062));
#29266=CARTESIAN_POINT('Origin',(0.5,-0.3400235721905,-10.));
#29267=CARTESIAN_POINT('',(0.3687670047111,-0.6178156792341,-8.5));
#29268=CARTESIAN_POINT('Origin',(-1.320743945967,1.320743945967,13.67962684375));
#29269=CARTESIAN_POINT('',(0.6178156792341,-0.3687670047111,-8.5));
#29270=CARTESIAN_POINT('Origin',(1.559976427809,-0.5,-10.));
#29271=CARTESIAN_POINT('Origin',(-1.293999677209,-1.293999677209,13.37393845305));
#29272=CARTESIAN_POINT('',(0.617815679234,0.3687670047111,-8.5));
#29273=CARTESIAN_POINT('Origin',(0.3400235721905,0.5,-10.));
#29274=CARTESIAN_POINT('',(1.150376451473,0.4994251259956,-9.993429160062));
#29275=CARTESIAN_POINT('Origin',(2.321412939997,1.421412939997,-23.40022640802));
#29276=CARTESIAN_POINT('',(0.,0.,0.));
#29277=CARTESIAN_POINT('Origin',(0.,0.,3.8));
#29278=CARTESIAN_POINT('',(0.133974596216,1.34752837055,4.03205080757));
#29279=CARTESIAN_POINT('',(0.133975838235341,0.664859028439009,4.03205295596885));
#29280=CARTESIAN_POINT('',(0.133974596216,1.34752837055,4.03205080757));
#29281=CARTESIAN_POINT('',(2.71354627738384,1.30409337481055,8.50000002111664));
#29282=CARTESIAN_POINT('Ctrl Pts',(0.133975839160916,0.664858977042815,
4.03205296041379));
#29283=CARTESIAN_POINT('Ctrl Pts',(0.247132282736217,0.683846965301094,
4.22804566988996));
#29284=CARTESIAN_POINT('Ctrl Pts',(0.36075899558286,0.704110746029599,4.42485290926822));
#29285=CARTESIAN_POINT('Ctrl Pts',(0.47425093097406,0.725533099101974,4.621426707294));
#29286=CARTESIAN_POINT('Ctrl Pts',(0.561430823810993,0.741988880199786,
4.77242671083931));
#29287=CARTESIAN_POINT('Ctrl Pts',(0.648531228319088,0.759127295663591,
4.92328903774398));
#29288=CARTESIAN_POINT('Ctrl Pts',(0.735278965462407,0.77687530163016,5.07354052591786));
#29289=CARTESIAN_POINT('Ctrl Pts',(0.821592229549516,0.794534417319612,
5.22303948468387));
#29290=CARTESIAN_POINT('Ctrl Pts',(0.907554962852823,0.812822098130855,
5.37193130515576));
#29291=CARTESIAN_POINT('Ctrl Pts',(0.993977273034051,0.831907903641516,
5.52161913744188));
#29292=CARTESIAN_POINT('Ctrl Pts',(1.04856084276224,0.843962330255724,5.61616065356101));
#29293=CARTESIAN_POINT('Ctrl Pts',(1.1033276922141,0.85633615357053,5.71101961970344));
#29294=CARTESIAN_POINT('Ctrl Pts',(1.15848133271126,0.869082750270139,5.80654852750131));
#29295=CARTESIAN_POINT('Ctrl Pts',(1.2180206215764,0.882842917252854,5.90967360111531));
#29296=CARTESIAN_POINT('Ctrl Pts',(1.27801067445639,0.897037334625361,6.01357942077414));
#29297=CARTESIAN_POINT('Ctrl Pts',(1.3387068707796,0.91174429412865,6.11870831663208));
#29298=CARTESIAN_POINT('Ctrl Pts',(1.43336285608852,0.934679862203939,6.28265729242754));
#29299=CARTESIAN_POINT('Ctrl Pts',(1.52973609727286,0.958853710900147,6.44958064268732));
#29300=CARTESIAN_POINT('Ctrl Pts',(1.62843729109613,0.984543986523405,6.62053612509274));
#29301=CARTESIAN_POINT('Ctrl Pts',(1.71302174746797,1.00655991068261,6.76704070100435));
#29302=CARTESIAN_POINT('Ctrl Pts',(1.79931583017353,1.02969013216229,6.91650643650829));
#29303=CARTESIAN_POINT('Ctrl Pts',(1.8877011757851,1.05413975161752,7.06959434585853));
#29304=CARTESIAN_POINT('Ctrl Pts',(1.92057356758229,1.06323308563645,7.12653099865718));
#29305=CARTESIAN_POINT('Ctrl Pts',(1.95373520706313,1.07250921588961,7.18396864316921));
#29306=CARTESIAN_POINT('Ctrl Pts',(1.98720558499433,1.08197974195953,7.24194103829456));
#29307=CARTESIAN_POINT('Ctrl Pts',(2.1539401013221,1.12915768500172,7.53073369194964));
#29308=CARTESIAN_POINT('Ctrl Pts',(2.32834097569438,1.18110458813524,7.83280486711957));
#29309=CARTESIAN_POINT('Ctrl Pts',(2.50952487075871,1.2383290506724,8.14662457897929));
#29310=CARTESIAN_POINT('Ctrl Pts',(2.5766171014717,1.25951921683814,8.26283173140252));
#29311=CARTESIAN_POINT('Ctrl Pts',(2.64463931462142,1.28143262361183,8.38064966061838));
#29312=CARTESIAN_POINT('Ctrl Pts',(2.71354626506708,1.304093369936,8.49999999978495));
#29313=CARTESIAN_POINT('',(2.713546265065,6.295906630064,8.499999999781));
#29314=CARTESIAN_POINT('',(2.713546265065,6.295906630064,8.499999999781));
#29315=CARTESIAN_POINT('',(0.133974546587078,6.93514124142996,4.03205068645143));
#29316=CARTESIAN_POINT('Ctrl Pts',(2.71354626506511,6.295906630064,8.49999999978094));
#29317=CARTESIAN_POINT('Ctrl Pts',(2.61139186763909,6.32950114282925,8.32306339322283));
#29318=CARTESIAN_POINT('Ctrl Pts',(2.50870084894661,6.36224673356896,8.14519733060976));
#29319=CARTESIAN_POINT('Ctrl Pts',(2.40615912187201,6.3939534451709,7.96758984811973));
#29320=CARTESIAN_POINT('Ctrl Pts',(2.3086542390515,6.42410272476244,7.79870643585148));
#29321=CARTESIAN_POINT('Ctrl Pts',(2.21128440432946,6.4533130808905,7.63005693828328));
#29322=CARTESIAN_POINT('Ctrl Pts',(2.11464207311449,6.48146460959975,7.46266751045704));
#29323=CARTESIAN_POINT('Ctrl Pts',(2.09163285950551,6.48816710248612,7.42281438344407));
#29324=CARTESIAN_POINT('Ctrl Pts',(2.06866466968897,6.49480642163638,7.38303231116932));
#29325=CARTESIAN_POINT('Ctrl Pts',(2.04571368948606,6.50138989845776,7.34328004662047));
#29326=CARTESIAN_POINT('Ctrl Pts',(1.96873400784639,6.52347148039071,7.20994732434137));
#29327=CARTESIAN_POINT('Ctrl Pts',(1.89194820262661,6.54492874953572,7.07695040454043));
#29328=CARTESIAN_POINT('Ctrl Pts',(1.81445492386495,6.56600503948902,6.94272810863974));
#29329=CARTESIAN_POINT('Ctrl Pts',(1.73791067961232,6.5868232151025,6.81014958872486));
#29330=CARTESIAN_POINT('Ctrl Pts',(1.66067615707177,6.60726972394034,6.67637547553564));
#29331=CARTESIAN_POINT('Ctrl Pts',(1.58187949656786,6.62752885128245,6.53989565838102));
#29332=CARTESIAN_POINT('Ctrl Pts',(1.55928046578883,6.63333920719643,6.50075298953098));
#29333=CARTESIAN_POINT('Ctrl Pts',(1.53655292167311,6.63913382699167,6.46138772885641));
#29334=CARTESIAN_POINT('Ctrl Pts',(1.51367625064916,6.64491626389417,6.42176417233491));
#29335=CARTESIAN_POINT('Ctrl Pts',(1.46609117940512,6.65694413594258,6.33934441125846));
#29336=CARTESIAN_POINT('Ctrl Pts',(1.417861702161,6.66892999551049,6.25580850454491));
#29337=CARTESIAN_POINT('Ctrl Pts',(1.36900976236698,6.68084982723003,6.17119446184299));
#29338=CARTESIAN_POINT('Ctrl Pts',(1.21594957699074,6.7181963821537,5.9060864412404));
#29339=CARTESIAN_POINT('Ctrl Pts',(1.05677805398043,6.75489136322574,5.63039328136468));
#29340=CARTESIAN_POINT('Ctrl Pts',(0.892178373440007,6.79022340698429,5.34529827216908));
#29341=CARTESIAN_POINT('Ctrl Pts',(0.880260159593054,6.79278170388852,5.32465532028037));
#29342=CARTESIAN_POINT('Ctrl Pts',(0.86831349204015,6.79533287580036,5.30396308511113));
#29343=CARTESIAN_POINT('Ctrl Pts',(0.856338632539872,6.79787666269458,5.28322202004314));
#29344=CARTESIAN_POINT('Ctrl Pts',(0.777345203864997,6.81465702229612,5.14640138811414));
#29345=CARTESIAN_POINT('Ctrl Pts',(0.697124668072234,6.83111225314263,5.00745534397502));
#29346=CARTESIAN_POINT('Ctrl Pts',(0.615648984965793,6.84719804282709,4.86633532126311));
#29347=CARTESIAN_POINT('Ctrl Pts',(0.459751271772893,6.87797701553522,4.59631256124802));
#29348=CARTESIAN_POINT('Ctrl Pts',(0.299258018817764,6.90740619144373,4.31833009316456));
#29349=CARTESIAN_POINT('Ctrl Pts',(0.133974596321897,6.935141228052,4.03205080775324));
#29350=CARTESIAN_POINT('',(0.133974596215585,6.25247165111742,4.03205080756906));
#29351=CARTESIAN_POINT('',(0.1339746084865,6.935141228052,4.03205080073));
#29352=CARTESIAN_POINT('',(0.0734244918642833,5.61500841690498,3.92717512466558));
#29353=CARTESIAN_POINT('Ctrl Pts',(0.1339745962156,6.252471629351,4.032050807569));
#29354=CARTESIAN_POINT('Ctrl Pts',(0.1339743516313,6.210070040294,4.032050175084));
#29355=CARTESIAN_POINT('Ctrl Pts',(0.1327751855236,6.126676439139,4.029973442397));
#29356=CARTESIAN_POINT('Ctrl Pts',(0.1277364860869,6.010122770097,4.021246134362));
#29357=CARTESIAN_POINT('Ctrl Pts',(0.1185452327114,5.889181793142,4.005326089051));
#29358=CARTESIAN_POINT('Ctrl Pts',(0.103261617757799,5.76029299121146,3.97885542594176));
#29359=CARTESIAN_POINT('Ctrl Pts',(0.0855624395784293,5.66383148718846,
3.94819620974927));
#29360=CARTESIAN_POINT('Ctrl Pts',(0.0734243412793448,5.61500841659961,
3.92717521231643));
#29361=CARTESIAN_POINT('',(-1.29316404762894E-8,5.24481852459253,3.79999997760173));
#29362=CARTESIAN_POINT('Origin',(-0.198918003246391,2.40959514383602,3.4554639118384));
#29363=CARTESIAN_POINT('',(0.14433756729743,3.79999999952898,4.04999999999999));
#29364=CARTESIAN_POINT('Ctrl Pts',(0.1443375672974,3.800000000001,4.05));
#29365=CARTESIAN_POINT('Ctrl Pts',(0.1443378984973,3.958261403905,4.050000359522));
#29366=CARTESIAN_POINT('Ctrl Pts',(0.1338012341637,4.276090778539,4.031750623427));
#29367=CARTESIAN_POINT('Ctrl Pts',(0.09119037446517,4.728509036729,3.957946375843));
#29368=CARTESIAN_POINT('Ctrl Pts',(0.03592510445712,5.070395215176,3.862224014774));
#29369=CARTESIAN_POINT('Ctrl Pts',(1.940766991559E-12,5.24481832766,3.800000000003));
#29370=CARTESIAN_POINT('',(3.386874111916E-13,2.355181672324,3.800000000001));
#29371=CARTESIAN_POINT('Ctrl Pts',(3.386874111916E-13,2.355181672324,3.800000000001));
#29372=CARTESIAN_POINT('Ctrl Pts',(0.03068797257625,2.504173780267,3.853152901811));
#29373=CARTESIAN_POINT('Ctrl Pts',(0.08231078075842,2.809566709961,3.942566526949));
#29374=CARTESIAN_POINT('Ctrl Pts',(0.1295382484853,3.25413134046,4.024366912382));
#29375=CARTESIAN_POINT('Ctrl Pts',(0.1443374905,3.61171344699,4.049999621415));
#29376=CARTESIAN_POINT('Ctrl Pts',(0.1443375672974,3.800000000001,4.05));
#29377=CARTESIAN_POINT('',(0.0734360006991422,1.98494851950308,3.92719616078412));
#29378=CARTESIAN_POINT('Origin',(-0.0267630005725188,2.98738908516278,3.75364512324667));
#29379=CARTESIAN_POINT('Ctrl Pts',(0.0734361377817803,1.98494851831011,
3.92719607885935));
#29380=CARTESIAN_POINT('Ctrl Pts',(0.0844284068963691,1.94072397567073,
3.94623216194698));
#29381=CARTESIAN_POINT('Ctrl Pts',(0.102287144414616,1.84748240172733,3.97716748379283));
#29382=CARTESIAN_POINT('Ctrl Pts',(0.119996932845,1.700515755579,4.007840642711));
#29383=CARTESIAN_POINT('Ctrl Pts',(0.1311959657202,1.536687730076,4.027237692571));
#29384=CARTESIAN_POINT('Ctrl Pts',(0.1339757766234,1.412832779138,4.03205384679));
#29385=CARTESIAN_POINT('Ctrl Pts',(0.133974596216,1.34752837055,4.03205080757));
#29386=CARTESIAN_POINT('Origin',(1.,6.995321512442,3.532050807569));
#29387=CARTESIAN_POINT('',(1.66253962058448E-16,1.34752836921872,3.53205080731726));
#29388=CARTESIAN_POINT('',(-8.905626236455E-12,0.6439853496971,3.532050807569));
#29389=CARTESIAN_POINT('',(0.,1.347528368525,3.532050807566));
#29390=CARTESIAN_POINT('Origin',(1.00129300833713,0.666005680359366,3.53122076182685));
#29391=CARTESIAN_POINT('Origin',(1.,1.347528370609,3.532050807569));
#29392=CARTESIAN_POINT('Origin',(0.,0.,-3.8));
#29393=CARTESIAN_POINT('',(-8.844466825586E-12,6.956014650303,-3.532050807569));
#29394=CARTESIAN_POINT('',(-2.12915400332963E-17,6.25247164440103,-3.5320508052874));
#29395=CARTESIAN_POINT('',(-8.844466825586E-12,6.956014650303,-3.532050807569));
#29396=CARTESIAN_POINT('',(3.29873385069466E-15,6.99871823693242,-2.87370869095006));
#29397=CARTESIAN_POINT('Origin',(0.,3.8,0.));
#29398=CARTESIAN_POINT('Origin',(0.,-42.4,0.));
#29399=CARTESIAN_POINT('Origin',(0.,0.,-3.8));
#29400=CARTESIAN_POINT('',(0.,1.34752836990142,-3.53205080743734));
#29401=CARTESIAN_POINT('',(3.55903513595825E-9,0.643985367713358,-3.53205101022315));
#29402=CARTESIAN_POINT('',(0.,1.347528369529,-3.532050807569));
#29403=CARTESIAN_POINT('',(2.73760181190852E-12,0.601281259440645,-2.87370767806568));
#29404=CARTESIAN_POINT('Origin',(0.,50.,0.));
#29405=CARTESIAN_POINT('Origin',(0.,3.8,0.));
#29406=CARTESIAN_POINT('Origin',(0.,0.,-3.8));
#29407=CARTESIAN_POINT('',(3.27721772858058E-15,0.601281763069545,2.87370869095238));
#29408=CARTESIAN_POINT('Origin',(0.,3.8,0.));
#29409=CARTESIAN_POINT('Origin',(0.,50.,0.));
#29410=CARTESIAN_POINT('Origin',(0.,0.,-3.8));
#29411=CARTESIAN_POINT('',(1.90152351602403E-8,6.95601462898345,3.5320510473839));
#29412=CARTESIAN_POINT('',(3.5763139446717E-16,6.25247164282405,3.53205080558666));
#29413=CARTESIAN_POINT('',(1.485361333931E-8,6.956014650303,3.532050807569));
#29414=CARTESIAN_POINT('',(2.73760181190852E-12,6.99871874056045,2.87370767806342));
#29415=CARTESIAN_POINT('Origin',(0.,-42.4,0.));
#29416=CARTESIAN_POINT('Origin',(0.,3.8,0.));
#29417=CARTESIAN_POINT('Origin',(1.,18.3911851122,-3.532050807569));
#29418=CARTESIAN_POINT('',(0.133975834635972,6.93514097197305,-4.0320529499034));
#29419=CARTESIAN_POINT('Origin',(1.00129390752562,6.93399590143332,-3.53122058726189));
#29420=CARTESIAN_POINT('',(0.133974596215514,6.25247165142154,-4.032050807569));
#29421=CARTESIAN_POINT('',(0.1339745986111,6.935141231182,-4.032050806435));
#29422=CARTESIAN_POINT('Origin',(1.,6.25247167405,-3.532050807569));
#29423=CARTESIAN_POINT('Ctrl Pts',(0.0005956539577002,6.267381300312,-3.496598976845));
#29424=CARTESIAN_POINT('Ctrl Pts',(0.0005454737658584,6.26241504239,-3.498634307646));
#29425=CARTESIAN_POINT('Ctrl Pts',(0.0001990202063126,6.230880706393,-3.511470929608));
#29426=CARTESIAN_POINT('Ctrl Pts',(-0.0007621112943634,6.173196747509,-3.533936979622));
#29427=CARTESIAN_POINT('Ctrl Pts',(-0.002892090579078,6.094032006508,-3.562357810308));
#29428=CARTESIAN_POINT('Ctrl Pts',(-0.00592218410683,6.014627167998,-3.588339308072));
#29429=CARTESIAN_POINT('Ctrl Pts',(-0.01012911618744,5.932736633387,-3.612262577613));
#29430=CARTESIAN_POINT('Ctrl Pts',(-0.01606034386805,5.845994028826,-3.633968305936));
#29431=CARTESIAN_POINT('Ctrl Pts',(-0.02193414995839,5.783303687288,-3.646093985463));
#29432=CARTESIAN_POINT('Ctrl Pts',(-0.02585027170663,5.750191401094,-3.650825051518));
#29433=CARTESIAN_POINT('Ctrl Pts',(-0.02638515003392,5.745804308856,-3.651418389814));
#29434=CARTESIAN_POINT('Ctrl Pts',(-0.006377801946632,6.26876976599,-3.693389523142));
#29435=CARTESIAN_POINT('Ctrl Pts',(-0.006032302342462,6.263345873378,-3.695442025085));
#29436=CARTESIAN_POINT('Ctrl Pts',(-0.003867291976553,6.228875461554,-3.708370566011));
#29437=CARTESIAN_POINT('Ctrl Pts',(-0.0002451597187239,6.165452133895,-3.730795665578));
#29438=CARTESIAN_POINT('Ctrl Pts',(0.003860634442441,6.077325338663,-3.758560483081));
#29439=CARTESIAN_POINT('Ctrl Pts',(0.00697153741604,5.987496073211,-3.783097616472));
#29440=CARTESIAN_POINT('Ctrl Pts',(0.008854436988706,5.892748574972,-3.804363708712));
#29441=CARTESIAN_POINT('Ctrl Pts',(0.008764742844783,5.788862659501,-3.821183298427));
#29442=CARTESIAN_POINT('Ctrl Pts',(0.005993463682357,5.709109095087,-3.826759357469));
#29443=CARTESIAN_POINT('Ctrl Pts',(0.002559975292538,5.66404914375,-3.825622482226));
#29444=CARTESIAN_POINT('Ctrl Pts',(0.002062518958956,5.658019058761,-3.825389338686));
#29445=CARTESIAN_POINT('Ctrl Pts',(0.04343955716361,6.270349119306,-3.88389624378));
#29446=CARTESIAN_POINT('Ctrl Pts',(0.04416842517361,6.26440357571,-3.885852742728));
#29447=CARTESIAN_POINT('Ctrl Pts',(0.0487635922003,6.226593348799,-3.898152002359));
#29448=CARTESIAN_POINT('Ctrl Pts',(0.05678337425826,6.156724067586,-3.919186369339));
#29449=CARTESIAN_POINT('Ctrl Pts',(0.0667793086814,6.058741282577,-3.944363515824));
#29450=CARTESIAN_POINT('Ctrl Pts',(0.0755852569517,5.95766968524,-3.965426912709));
#29451=CARTESIAN_POINT('Ctrl Pts',(0.08297966657217,5.849310626945,-3.981825631411));
#29452=CARTESIAN_POINT('Ctrl Pts',(0.08796210861139,5.727591585706,-3.991250184282));
#29453=CARTESIAN_POINT('Ctrl Pts',(0.08757643356987,5.630384339256,-3.988276144813));
#29454=CARTESIAN_POINT('Ctrl Pts',(0.08417413305102,5.573211510378,-3.980120686141));
#29455=CARTESIAN_POINT('Ctrl Pts',(0.08365291538563,5.56551734014,-3.978906690537));
#29456=CARTESIAN_POINT('Ctrl Pts',(0.1458535053006,6.271986391254,-4.052079985885));
#29457=CARTESIAN_POINT('Ctrl Pts',(0.1469211537512,6.265499099249,-4.053835390391));
#29458=CARTESIAN_POINT('Ctrl Pts',(0.1536605702835,6.224226503898,-4.064837148956));
#29459=CARTESIAN_POINT('Ctrl Pts',(0.1655221409961,6.147747382447,-4.083248089847));
#29460=CARTESIAN_POINT('Ctrl Pts',(0.1805666794667,6.039844468178,-4.104123768826));
#29461=CARTESIAN_POINT('Ctrl Pts',(0.1941422442452,5.927659149072,-4.119976518101));
#29462=CARTESIAN_POINT('Ctrl Pts',(0.2060058169343,5.806079919546,-4.129707461221));
#29463=CARTESIAN_POINT('Ctrl Pts',(0.2148639642194,5.66733934524,-4.129850682383));
#29464=CARTESIAN_POINT('Ctrl Pts',(0.2159461215713,5.553757419004,-4.117045916765));
#29465=CARTESIAN_POINT('Ctrl Pts',(0.2121209376649,5.485326308278,-4.101312141519));
#29466=CARTESIAN_POINT('Ctrl Pts',(0.2115167758576,5.476087063052,-4.099045503577));
#29467=CARTESIAN_POINT('',(-0.0201793190613418,5.74664977779542,-3.67573539656421));
#29468=CARTESIAN_POINT('Ctrl Pts',(-8.5045295969094E-17,6.252471629776,
-3.532050807569));
#29469=CARTESIAN_POINT('Ctrl Pts',(-1.72754179486701E-9,6.22515092260001,
-3.542947549531));
#29470=CARTESIAN_POINT('Ctrl Pts',(-0.000132427690026248,6.19801380159061,
-3.55333740578014));
#29471=CARTESIAN_POINT('Ctrl Pts',(-0.000397224786372729,6.17126247112049,
-3.56316476120976));
#29472=CARTESIAN_POINT('Ctrl Pts',(-0.000637049866794604,6.14703395777986,
-3.57206533579596));
#29473=CARTESIAN_POINT('Ctrl Pts',(-0.000983692273868425,6.12312170573986,
-3.5805035516757));
#29474=CARTESIAN_POINT('Ctrl Pts',(-0.00145122229008661,6.09910625879538,
-3.58861822102923));
#29475=CARTESIAN_POINT('Ctrl Pts',(-0.00149990430028179,6.09660562740823,
-3.58946316873846));
#29476=CARTESIAN_POINT('Ctrl Pts',(-0.00154991211757044,6.09410386888282,
-3.5903045648392));
#29477=CARTESIAN_POINT('Ctrl Pts',(-0.00160127252760695,6.09160050491002,
-3.59114253456933));
#29478=CARTESIAN_POINT('Ctrl Pts',(-0.0021458856451855,6.06505545091433,
-3.60002815886317));
#29479=CARTESIAN_POINT('Ctrl Pts',(-0.00284151775027957,6.03833096917016,
-3.60853468104776));
#29480=CARTESIAN_POINT('Ctrl Pts',(-0.0037223342651763,6.01134660899402,
-3.61661970088636));
#29481=CARTESIAN_POINT('Ctrl Pts',(-0.00436205786534019,5.99174827977556,
-3.62249172747882));
#29482=CARTESIAN_POINT('Ctrl Pts',(-0.00509925812006014,5.9720138726226,
-3.62813767104629));
#29483=CARTESIAN_POINT('Ctrl Pts',(-0.00596753483628204,5.95189359828813,
-3.63358175376179));
#29484=CARTESIAN_POINT('Ctrl Pts',(-0.00629476266444873,5.94431086164487,
-3.63563346761069));
#29485=CARTESIAN_POINT('Ctrl Pts',(-0.00664075452653387,5.93667343669818,
-3.63765606058147));
#29486=CARTESIAN_POINT('Ctrl Pts',(-0.00700790819414537,5.92896854922353,
-3.63964899627758));
#29487=CARTESIAN_POINT('Ctrl Pts',(-0.00782485968872279,5.91182444882841,
-3.64408346592657));
#29488=CARTESIAN_POINT('Ctrl Pts',(-0.00874585896548231,5.89434844461603,
-3.6483701221662));
#29489=CARTESIAN_POINT('Ctrl Pts',(-0.00981144211653737,5.87644460480726,
-3.65245416715839));
#29490=CARTESIAN_POINT('Ctrl Pts',(-0.0104954637008456,5.86495173082641,
-3.65507580670212));
#29491=CARTESIAN_POINT('Ctrl Pts',(-0.011239294790122,5.85328292767612,
-3.65761330920383));
#29492=CARTESIAN_POINT('Ctrl Pts',(-0.0120569570969732,5.8414189888438,
-3.66004292839892));
#29493=CARTESIAN_POINT('Ctrl Pts',(-0.0120570279255355,5.84141796115092,
-3.66004313886041));
#29494=CARTESIAN_POINT('Ctrl Pts',(-0.01205709875466,5.84141693345665,-3.66004334932103));
#29495=CARTESIAN_POINT('Ctrl Pts',(-0.0120571695843467,5.84141590576098,
-3.66004355978076));
#29496=CARTESIAN_POINT('Ctrl Pts',(-0.0130092523383889,5.82760176412085,
-3.6628725300981));
#29497=CARTESIAN_POINT('Ctrl Pts',(-0.0140620820519736,5.81353299437985,
-3.66554488478095));
#29498=CARTESIAN_POINT('Ctrl Pts',(-0.015250518781809,5.79919911074599,
-3.66800316381262));
#29499=CARTESIAN_POINT('Ctrl Pts',(-0.0163231857994438,5.78626154005109,
-3.67022197342293));
#29500=CARTESIAN_POINT('Ctrl Pts',(-0.0175062495206092,5.77310770600626,
-3.6722665937512));
#29501=CARTESIAN_POINT('Ctrl Pts',(-0.0188341058644166,5.75975835931925,
-3.6740632774332));
#29502=CARTESIAN_POINT('Ctrl Pts',(-0.0192667280551368,5.75540907587805,
-3.67464864589882));
#29503=CARTESIAN_POINT('Ctrl Pts',(-0.0197147999565475,5.75103929996326,
-3.67520741276272));
#29504=CARTESIAN_POINT('Ctrl Pts',(-0.020179768057466,5.74665057746385,
-3.67573612888107));
#29505=CARTESIAN_POINT('',(0.0734352791607451,5.61504677957465,-3.92719395374012));
#29506=CARTESIAN_POINT('Ctrl Pts',(0.1339745962155,6.252471629345,-4.032050807569));
#29507=CARTESIAN_POINT('Ctrl Pts',(0.1339746659036,6.217593804566,-4.032050986724));
#29508=CARTESIAN_POINT('Ctrl Pts',(0.1331756273777,6.148571274798,-4.030666927977));
#29509=CARTESIAN_POINT('Ctrl Pts',(0.1296207577408,6.048706349432,-4.024509737841));
#29510=CARTESIAN_POINT('Ctrl Pts',(0.1233657849458,5.948101684635,-4.013675833537));
#29511=CARTESIAN_POINT('Ctrl Pts',(0.1137608443202,5.845755231197,-3.997039458174));
#29512=CARTESIAN_POINT('Ctrl Pts',(0.09929412924214,5.73725831333,-3.971982867046));
#29513=CARTESIAN_POINT('Ctrl Pts',(0.08367513844526,5.656233648091,-3.944928749805));
#29514=CARTESIAN_POINT('Ctrl Pts',(0.07343513682107,5.615047318658,-3.927194345532));
#29515=CARTESIAN_POINT('Origin',(0.9394606772721,5.615046199005,-3.42719362363));
#29516=CARTESIAN_POINT('Origin',(-0.5,3.8,0.));
#29517=CARTESIAN_POINT('',(-0.500000724156137,5.57843318952544,-3.35815048826204));
#29518=CARTESIAN_POINT('Origin',(-0.5,5.81246117975,-3.8));
#29519=CARTESIAN_POINT('',(-0.5000000000008,6.6267742539821,-2.53955651975393));
#29520=CARTESIAN_POINT('Origin',(-0.5,3.8,0.));
#29521=CARTESIAN_POINT('Origin',(-0.5,6.9987182356,-2.873708692481));
#29522=CARTESIAN_POINT('Ctrl Pts',(0.1027377857463,7.348398502532,-1.993772793209));
#29523=CARTESIAN_POINT('Ctrl Pts',(0.1018795142078,7.347090839248,-1.99856950602));
#29524=CARTESIAN_POINT('Ctrl Pts',(0.08748606425769,7.324973749974,-2.07931804569));
#29525=CARTESIAN_POINT('Ctrl Pts',(0.06218815931635,7.280065532666,-2.23117883235));
#29526=CARTESIAN_POINT('Ctrl Pts',(0.03182029544443,7.206284734385,-2.449036815777));
#29527=CARTESIAN_POINT('Ctrl Pts',(0.008692153136156,7.121345659417,-2.66975021154));
#29528=CARTESIAN_POINT('Ctrl Pts',(0.000309930076861,7.05450915858,-2.821709674269));
#29529=CARTESIAN_POINT('Ctrl Pts',(-0.001018477605139,7.016398931017,-2.902151700762));
#29530=CARTESIAN_POINT('Ctrl Pts',(-0.001081418569356,7.014306738012,-2.906550131397));
#29531=CARTESIAN_POINT('Ctrl Pts',(-0.0399338660445,7.115798705959,-1.82477577565));
#29532=CARTESIAN_POINT('Ctrl Pts',(-0.04008326187015,7.11417406958,-1.82941037646));
#29533=CARTESIAN_POINT('Ctrl Pts',(-0.04249896901661,7.086774456842,-1.907411774627));
#29534=CARTESIAN_POINT('Ctrl Pts',(-0.04384834652326,7.033658223989,-2.053551607733));
#29535=CARTESIAN_POINT('Ctrl Pts',(-0.03627411384628,6.953727053625,-2.261605825128));
#29536=CARTESIAN_POINT('Ctrl Pts',(-0.01768977584952,6.869675880613,-2.470533055801));
#29537=CARTESIAN_POINT('Ctrl Pts',(0.004566050698255,6.810275339171,-2.612726145468));
#29538=CARTESIAN_POINT('Ctrl Pts',(0.01963083731976,6.778767570989,-2.687391402537));
#29539=CARTESIAN_POINT('Ctrl Pts',(0.02046458526668,6.777044591192,-2.691471916486));
#29540=CARTESIAN_POINT('Ctrl Pts',(-0.3385562814282,7.087745121797,-1.710515139935));
#29541=CARTESIAN_POINT('Ctrl Pts',(-0.3385854937958,7.085344330529,-1.715026264093));
#29542=CARTESIAN_POINT('Ctrl Pts',(-0.3389179244204,7.044875153857,-1.790931560509));
#29543=CARTESIAN_POINT('Ctrl Pts',(-0.3344184843395,6.967075079031,-1.932588547285));
#29544=CARTESIAN_POINT('Ctrl Pts',(-0.3129178506928,6.851934620108,-2.132671483461));
#29545=CARTESIAN_POINT('Ctrl Pts',(-0.2740805475891,6.733152916448,-2.331716051354));
#29546=CARTESIAN_POINT('Ctrl Pts',(-0.2328066607505,6.65131313147,-2.465517500439));
#29547=CARTESIAN_POINT('Ctrl Pts',(-0.2060460780354,6.608722577737,-2.535169689394));
#29548=CARTESIAN_POINT('Ctrl Pts',(-0.2045679022214,6.606396058465,-2.538974208362));
#29549=CARTESIAN_POINT('Ctrl Pts',(-0.592664250327,7.283070119461,-1.727694044175));
#29550=CARTESIAN_POINT('Ctrl Pts',(-0.5932426506397,7.279955024242,-1.732203216897));
#29551=CARTESIAN_POINT('Ctrl Pts',(-0.6027847744321,7.227402840675,-1.808070564299));
#29552=CARTESIAN_POINT('Ctrl Pts',(-0.6144625375172,7.12501335913,-1.949492146448));
#29553=CARTESIAN_POINT('Ctrl Pts',(-0.6123999906409,6.969240688534,-2.148787406838));
#29554=CARTESIAN_POINT('Ctrl Pts',(-0.5883650519266,6.803424624825,-2.346487045211));
#29555=CARTESIAN_POINT('Ctrl Pts',(-0.5524599168805,6.684333856262,-2.478904894028));
#29556=CARTESIAN_POINT('Ctrl Pts',(-0.5265523235192,6.62041514534,-2.547672988512));
#29557=CARTESIAN_POINT('Ctrl Pts',(-0.5251145852718,6.616917489925,-2.551428709617));
#29558=CARTESIAN_POINT('',(0.0865773249525527,7.32353859101868,-1.99264087060027));
#29559=CARTESIAN_POINT('Ctrl Pts',(0.0865773249525527,7.32353859101868,
-1.99264087060027));
#29560=CARTESIAN_POINT('Ctrl Pts',(0.0865771947823673,7.32353836781842,
-1.99264166097111));
#29561=CARTESIAN_POINT('Ctrl Pts',(0.086577064612313,7.32353814461806,-1.99264245134174));
#29562=CARTESIAN_POINT('Ctrl Pts',(0.0865769344423899,7.32353792141759,
-1.99264324171215));
#29563=CARTESIAN_POINT('Ctrl Pts',(0.0784200001016045,7.3095513450823,-2.04217080846305));
#29564=CARTESIAN_POINT('Ctrl Pts',(0.0707810911838816,7.2951582449645,-2.09085455336554));
#29565=CARTESIAN_POINT('Ctrl Pts',(0.0637332814097185,7.28051481411837,
-2.13835021065206));
#29566=CARTESIAN_POINT('Ctrl Pts',(0.0597136280219686,7.27216306821502,
-2.16543892130584));
#29567=CARTESIAN_POINT('Ctrl Pts',(0.0558856017076574,7.26373046498478,
-2.19214149885421));
#29568=CARTESIAN_POINT('Ctrl Pts',(0.0522572081991286,7.25525026918575,
-2.21839710659367));
#29569=CARTESIAN_POINT('Ctrl Pts',(0.0471928269707495,7.24341391672931,
-2.2550437400591));
#29570=CARTESIAN_POINT('Ctrl Pts',(0.0425107423662426,7.23148153503544,
-2.29081396288452));
#29571=CARTESIAN_POINT('Ctrl Pts',(0.0381540197775249,7.21930644129638,
-2.32622193849712));
#29572=CARTESIAN_POINT('Ctrl Pts',(0.0339164169989268,7.20746423422267,
-2.36066180304784));
#29573=CARTESIAN_POINT('Ctrl Pts',(0.0299862609982032,7.19539220723823,
-2.39475922278885));
#29574=CARTESIAN_POINT('Ctrl Pts',(0.0263406370665062,7.18292131512308,
-2.42897308992333));
#29575=CARTESIAN_POINT('Ctrl Pts',(0.0228702839175758,7.17104998650207,
-2.46154205583199));
#29576=CARTESIAN_POINT('Ctrl Pts',(0.0196579772059949,7.15881950455865,
-2.49421313164689));
#29577=CARTESIAN_POINT('Ctrl Pts',(0.0167223210419962,7.14605148199297,
-2.5273562255484));
#29578=CARTESIAN_POINT('Ctrl Pts',(0.0139677607901511,7.13407109822549,
-2.55845477523683));
#29579=CARTESIAN_POINT('Ctrl Pts',(0.0114564603782286,7.12161730275651,
-2.58996911427475));
#29580=CARTESIAN_POINT('Ctrl Pts',(0.00923922793207137,7.10851913572161,
-2.62218604510167));
#29581=CARTESIAN_POINT('Ctrl Pts',(0.00878499123308488,7.10583575980087,
-2.62878621565919));
#29582=CARTESIAN_POINT('Ctrl Pts',(0.00834323197844714,7.10312525936709,
-2.63541580115636));
#29583=CARTESIAN_POINT('Ctrl Pts',(0.00791460756887311,7.10038603852835,
-2.6420771479805));
#29584=CARTESIAN_POINT('Ctrl Pts',(0.00537502089604281,7.08415623784361,
-2.6815454265942));
#29585=CARTESIAN_POINT('Ctrl Pts',(0.00329666450163376,7.06693306420007,
-2.72213393301624));
#29586=CARTESIAN_POINT('Ctrl Pts',(0.00190428975516473,7.04869070748955,
-2.76359889037046));
#29587=CARTESIAN_POINT('Ctrl Pts',(0.000692060774264857,7.03280855109417,
-2.79969910198664));
#29588=CARTESIAN_POINT('Ctrl Pts',(3.33158514292476E-7,7.01615400055903,
-2.8364631507495));
#29589=CARTESIAN_POINT('Ctrl Pts',(1.31917426878845E-14,6.998718237797,
-2.873708690212));
#29590=CARTESIAN_POINT('',(-0.326860549423355,7.16212374689392,-1.77090033128315));
#29591=CARTESIAN_POINT('Ctrl Pts',(-0.326860549423355,7.16212374689392,
-1.77090033128315));
#29592=CARTESIAN_POINT('Ctrl Pts',(-0.341476935580464,7.14155250819475,
-1.80995513075379));
#29593=CARTESIAN_POINT('Ctrl Pts',(-0.355243357180322,7.1204502792182,-1.84836296151781));
#29594=CARTESIAN_POINT('Ctrl Pts',(-0.36807890051019,7.09898686777342,-1.88591138220589));
#29595=CARTESIAN_POINT('Ctrl Pts',(-0.377748086069401,7.08281819437489,
-1.9141971070683));
#29596=CARTESIAN_POINT('Ctrl Pts',(-0.38688975485068,7.06644508030668,-1.94199540467259));
#29597=CARTESIAN_POINT('Ctrl Pts',(-0.395485916070083,7.04994875753415,
-1.96922143838673));
#29598=CARTESIAN_POINT('Ctrl Pts',(-0.404085211517348,7.03344642007283,
-1.9964573989265));
#29599=CARTESIAN_POINT('Ctrl Pts',(-0.412118118968983,7.01682138823379,
-2.02312644173482));
#29600=CARTESIAN_POINT('Ctrl Pts',(-0.419672264309048,6.99993273664901,
-2.04949488838498));
#29601=CARTESIAN_POINT('Ctrl Pts',(-0.426990524612547,6.98357144852062,
-2.07503995638378));
#29602=CARTESIAN_POINT('Ctrl Pts',(-0.433859736224371,6.966962542256,-2.10030304038216));
#29603=CARTESIAN_POINT('Ctrl Pts',(-0.440323069309193,6.94994622360776,
-2.12552084006602));
#29604=CARTESIAN_POINT('Ctrl Pts',(-0.442710521659904,6.94366066638457,
-2.1348358938231));
#29605=CARTESIAN_POINT('Ctrl Pts',(-0.445042205251157,6.93731921540242,
-2.14414470422125));
#29606=CARTESIAN_POINT('Ctrl Pts',(-0.447318840123917,6.93091273586232,
-2.15345894792871));
#29607=CARTESIAN_POINT('Ctrl Pts',(-0.453065560394441,6.91474139179818,
-2.1769701195086));
#29608=CARTESIAN_POINT('Ctrl Pts',(-0.458453707982576,6.89815868002326,
-2.20051479902279));
#29609=CARTESIAN_POINT('Ctrl Pts',(-0.463470320481012,6.88099827454854,
-2.22428451544489));
#29610=CARTESIAN_POINT('Ctrl Pts',(-0.468181060798269,6.86488417086694,
-2.24660494811022));
#29611=CARTESIAN_POINT('Ctrl Pts',(-0.472564400803481,6.84826055599381,
-2.26912390370278));
#29612=CARTESIAN_POINT('Ctrl Pts',(-0.476570826991915,6.83096858818743,
-2.29199185391141));
#29613=CARTESIAN_POINT('Ctrl Pts',(-0.479287319175806,6.81924405036223,
-2.30749709601038));
#29614=CARTESIAN_POINT('Ctrl Pts',(-0.481829773480396,6.80721183561284,
-2.32316262215034));
#29615=CARTESIAN_POINT('Ctrl Pts',(-0.484170543101125,6.79481658859908,
-2.33903262068985));
#29616=CARTESIAN_POINT('Ctrl Pts',(-0.488905298622254,6.76974429454912,
-2.37113341460814));
#29617=CARTESIAN_POINT('Ctrl Pts',(-0.492850085687612,6.74319348125157,
-2.40405829232308));
#29618=CARTESIAN_POINT('Ctrl Pts',(-0.495623538805572,6.71517798283673,
-2.4375635794965));
#29619=CARTESIAN_POINT('Ctrl Pts',(-0.498396991923532,6.6871624844219,-2.47106886666992));
#29620=CARTESIAN_POINT('Ctrl Pts',(-0.499999415858718,6.65768246277223,
-2.50515434966105));
#29621=CARTESIAN_POINT('Ctrl Pts',(-0.500000000001596,6.62677425398226,
-2.53955651975406));
#29622=CARTESIAN_POINT('Origin',(-0.3268607615544,7.60451284409,-2.00391666631));
#29623=CARTESIAN_POINT('Origin',(0.5,-42.4,0.));
#29624=CARTESIAN_POINT('',(0.517449748472425,7.45443543149202,-3.56771915706352));
#29625=CARTESIAN_POINT('Origin',(0.5,6.956014650303,-3.532050807563));
#29626=CARTESIAN_POINT('',(0.517453499954001,7.54185174628463,-2.0013495955528));
#29627=CARTESIAN_POINT('Origin',(0.5,7.0425494055,-1.981381677743));
#29628=CARTESIAN_POINT('Origin',(0.5174497483513,-42.4,0.));
#29629=CARTESIAN_POINT('Ctrl Pts',(0.001285129943234,6.928768667338,-3.501024341666));
#29630=CARTESIAN_POINT('Ctrl Pts',(0.001003718906394,6.928092877268,-3.51066527064));
#29631=CARTESIAN_POINT('Ctrl Pts',(0.0002283234512161,6.924321936393,-3.563904385738));
#29632=CARTESIAN_POINT('Ctrl Pts',(0.00658911429773,6.917089265922,-3.660499255977));
#29633=CARTESIAN_POINT('Ctrl Pts',(0.03208935343955,6.906663907416,-3.788338152623));
#29634=CARTESIAN_POINT('Ctrl Pts',(0.07394580619339,6.895769141277,-3.911589220024));
#29635=CARTESIAN_POINT('Ctrl Pts',(0.1166553948127,6.887488515458,-3.998174012346));
#29636=CARTESIAN_POINT('Ctrl Pts',(0.1438590730748,6.882919565931,-4.043718798227));
#29637=CARTESIAN_POINT('Ctrl Pts',(0.1489300235062,6.882088247686,-4.051932578979));
#29638=CARTESIAN_POINT('Ctrl Pts',(-0.01806327553642,7.257042281495,-3.523522559884));
#29639=CARTESIAN_POINT('Ctrl Pts',(-0.01835336820514,7.256343395302,-3.5334930686));
#29640=CARTESIAN_POINT('Ctrl Pts',(-0.01915268912732,7.252443569868,-3.588552069544));
#29641=CARTESIAN_POINT('Ctrl Pts',(-0.01259578433519,7.244963592271,-3.688447745911));
#29642=CARTESIAN_POINT('Ctrl Pts',(0.01369008223242,7.234181570178,-3.820653304321));
#29643=CARTESIAN_POINT('Ctrl Pts',(0.05683526715279,7.222914110192,-3.948112582044));
#29644=CARTESIAN_POINT('Ctrl Pts',(0.1008602464213,7.214350258091,-4.037654288618));
#29645=CARTESIAN_POINT('Ctrl Pts',(0.1289014667209,7.209625219336,-4.084753946765));
#29646=CARTESIAN_POINT('Ctrl Pts',(0.1341285295189,7.208765508589,-4.093248118291));
#29647=CARTESIAN_POINT('Ctrl Pts',(0.2189431301382,7.484961949496,-3.546425270851));
#29648=CARTESIAN_POINT('Ctrl Pts',(0.2187175076249,7.484415939128,-3.554209822187));
#29649=CARTESIAN_POINT('Ctrl Pts',(0.2180958581636,7.481370070208,-3.597198589814));
#29650=CARTESIAN_POINT('Ctrl Pts',(0.2231964118796,7.475537193372,-3.675204532862));
#29651=CARTESIAN_POINT('Ctrl Pts',(0.2436481704901,7.467148227663,-3.778456557303));
#29652=CARTESIAN_POINT('Ctrl Pts',(0.2772231730612,7.458397511567,-3.87801747527));
#29653=CARTESIAN_POINT('Ctrl Pts',(0.3114799869555,7.451757587929,-3.947956342863));
#29654=CARTESIAN_POINT('Ctrl Pts',(0.3333015807294,7.448096469322,-3.984749318309));
#29655=CARTESIAN_POINT('Ctrl Pts',(0.3373693460768,7.447430403692,-3.99138493732));
#29656=CARTESIAN_POINT('Ctrl Pts',(0.5469709874831,7.453533131528,-3.553755766535));
#29657=CARTESIAN_POINT('Ctrl Pts',(0.5468380131604,7.453209324245,-3.558363725938));
#29658=CARTESIAN_POINT('Ctrl Pts',(0.5464716902076,7.451404541169,-3.583812218248));
#29659=CARTESIAN_POINT('Ctrl Pts',(0.5494793641476,7.447964171537,-3.630007953227));
#29660=CARTESIAN_POINT('Ctrl Pts',(0.561547096288,7.443048609365,-3.691183951173));
#29661=CARTESIAN_POINT('Ctrl Pts',(0.5813690679602,7.437948418878,-3.750201563262));
#29662=CARTESIAN_POINT('Ctrl Pts',(0.6015883374525,7.434097464698,-3.791652588125));
#29663=CARTESIAN_POINT('Ctrl Pts',(0.6144718870048,7.431978095285,-3.813467167341));
#29664=CARTESIAN_POINT('Ctrl Pts',(0.6168736596913,7.431592627446,-3.817401798674));
#29665=CARTESIAN_POINT('',(0.584439518575878,7.43337435977711,-3.82024990776836));
#29666=CARTESIAN_POINT('Origin',(0.5669897707333,6.935140821459,-3.782055090282));
#29667=CARTESIAN_POINT('Origin',(1.02904178594563,7.43196848844121,-3.56616243168394));
#29668=CARTESIAN_POINT('Ctrl Pts',(0.1075899274291,6.910200321737,-3.984624534481));
#29669=CARTESIAN_POINT('Ctrl Pts',(0.2365969974133,6.888757665974,-4.208071334229));
#29670=CARTESIAN_POINT('Ctrl Pts',(0.5917961608702,6.825498881099,-4.823294332142));
#29671=CARTESIAN_POINT('Ctrl Pts',(1.187797482473,6.69978878732,-5.855598902537));
#29672=CARTESIAN_POINT('Ctrl Pts',(1.927362895286,6.511611808779,-7.13656377305));
#29673=CARTESIAN_POINT('Ctrl Pts',(2.448474526329,6.35378224873,-8.039155594431));
#29674=CARTESIAN_POINT('Ctrl Pts',(2.72900660943,6.261296816161,-8.525051415516));
#29675=CARTESIAN_POINT('Ctrl Pts',(2.737553413063,6.258472120031,-8.53985491365));
#29676=CARTESIAN_POINT('Ctrl Pts',(0.1045493633812,7.227561823644,-4.016835013129));
#29677=CARTESIAN_POINT('Ctrl Pts',(0.2341802329362,7.206015484363,-4.241362265427));
#29678=CARTESIAN_POINT('Ctrl Pts',(0.591097759154,7.142450678831,-4.859561554948));
#29679=CARTESIAN_POINT('Ctrl Pts',(1.189986798084,7.016131565785,-5.896867798471));
#29680=CARTESIAN_POINT('Ctrl Pts',(1.933144313516,6.827040714483,-7.184054373226));
#29681=CARTESIAN_POINT('Ctrl Pts',(2.456795161336,6.668442221886,-8.091044247077));
#29682=CARTESIAN_POINT('Ctrl Pts',(2.738697034763,6.575505198669,-8.579312614601));
#29683=CARTESIAN_POINT('Ctrl Pts',(2.747285573639,6.572666709152,-8.594188400297));
#29684=CARTESIAN_POINT('Ctrl Pts',(0.3084981556159,7.45325258704,-3.920743118734));
#29685=CARTESIAN_POINT('Ctrl Pts',(0.4385726385281,7.431632513509,-4.146038731906));
#29686=CARTESIAN_POINT('Ctrl Pts',(0.7967121737199,7.367850082224,-4.766354603057));
#29687=CARTESIAN_POINT('Ctrl Pts',(1.397654804922,7.241097866794,-5.807217772734));
#29688=CARTESIAN_POINT('Ctrl Pts',(2.1433668343,7.051357117379,-7.098828895431));
#29689=CARTESIAN_POINT('Ctrl Pts',(2.668823439181,6.892211800505,-8.008946432258));
#29690=CARTESIAN_POINT('Ctrl Pts',(2.951699435248,6.798953629834,-8.498902029688));
#29691=CARTESIAN_POINT('Ctrl Pts',(2.960317654028,6.79610533119,-8.513829222485));
#29692=CARTESIAN_POINT('Ctrl Pts',(0.5837385360342,7.437108776495,-3.760283800157));
#29693=CARTESIAN_POINT('Ctrl Pts',(0.7137812869877,7.415493977224,-3.985524451965));
#29694=CARTESIAN_POINT('Ctrl Pts',(1.071833411064,7.351727112854,-4.605688922623));
#29695=CARTESIAN_POINT('Ctrl Pts',(1.672629147444,7.225005877526,-5.646297663004));
#29696=CARTESIAN_POINT('Ctrl Pts',(2.418158450738,7.035311615755,-6.937592294841));
#29697=CARTESIAN_POINT('Ctrl Pts',(2.943485888615,6.876205413586,-7.847486107853));
#29698=CARTESIAN_POINT('Ctrl Pts',(3.226292205042,6.782970214806,-8.337321016606));
#29699=CARTESIAN_POINT('Ctrl Pts',(3.234908300798,6.780122617815,-8.352244532218));
#29700=CARTESIAN_POINT('',(3.16400873498434,6.78858150430351,-8.33346840037192));
#29701=CARTESIAN_POINT('Origin',(-2.22649218408928,-42.9537256923742,1.07765501392591));
#29702=CARTESIAN_POINT('',(2.71354627844193,6.29590662476739,-8.50000002294956));
#29703=CARTESIAN_POINT('Origin',(3.146558987422,6.295906623345,-8.250000035222));
#29704=CARTESIAN_POINT('Ctrl Pts',(0.133975835628604,6.93514102322294,-4.03205295429546));
#29705=CARTESIAN_POINT('Ctrl Pts',(0.248035870487217,6.91600141019252,-4.22961072978345));
#29706=CARTESIAN_POINT('Ctrl Pts',(0.362516631904128,6.89557480007011,-4.42789722465242));
#29707=CARTESIAN_POINT('Ctrl Pts',(0.476791103889355,6.87398689887345,-4.62582641581095));
#29708=CARTESIAN_POINT('Ctrl Pts',(0.482878673537709,6.87283687954006,-4.63637039571904));
#29709=CARTESIAN_POINT('Ctrl Pts',(0.488965658428778,6.87168357686734,-4.64691336279973));
#29710=CARTESIAN_POINT('Ctrl Pts',(0.495051964002143,6.87052701398906,-4.65745515327007));
#29711=CARTESIAN_POINT('Ctrl Pts',(0.575619875510765,6.85521692899437,-4.79700286928915));
#29712=CARTESIAN_POINT('Ctrl Pts',(0.656068680033741,6.83933448907174,-4.93634428707301));
#29713=CARTESIAN_POINT('Ctrl Pts',(0.736179400348117,6.82294025017375,-5.07510012488849));
#29714=CARTESIAN_POINT('Ctrl Pts',(0.8221140916706,6.80535416614358,-5.22394337639183));
#29715=CARTESIAN_POINT('Ctrl Pts',(0.907658335949794,6.78715361300796,-5.37211035257136));
#29716=CARTESIAN_POINT('Ctrl Pts',(0.993626289906327,6.76817004995011,-5.52101121679085));
#29717=CARTESIAN_POINT('Ctrl Pts',(1.05313261411875,6.7550297807447,-5.62407919379812));
#29718=CARTESIAN_POINT('Ctrl Pts',(1.11284190195264,6.74151329238067,-5.7274987143937));
#29719=CARTESIAN_POINT('Ctrl Pts',(1.17302336159817,6.7275501453763,-5.83173606042337));
#29720=CARTESIAN_POINT('Ctrl Pts',(1.22800856343403,6.71479262070306,-5.92697322389587));
#29721=CARTESIAN_POINT('Ctrl Pts',(1.28338791583026,6.70166212210795,-6.02289307603832));
#29722=CARTESIAN_POINT('Ctrl Pts',(1.33936622442084,6.688095964508,-6.11985035063901));
#29723=CARTESIAN_POINT('Ctrl Pts',(1.43348966283431,6.66528546109131,-6.28287692815426));
#29724=CARTESIAN_POINT('Ctrl Pts',(1.52930637368736,6.64125189706976,-6.44883633960552));
#29725=CARTESIAN_POINT('Ctrl Pts',(1.62743110009301,6.6157179419123,-6.61879335115343));
#29726=CARTESIAN_POINT('Ctrl Pts',(1.71482541704086,6.59297624721713,-6.77016474834157));
#29727=CARTESIAN_POINT('Ctrl Pts',(1.80405054587966,6.56904390809249,-6.92470720466088));
#29728=CARTESIAN_POINT('Ctrl Pts',(1.89553771225012,6.54369067439583,-7.08316762517741));
#29729=CARTESIAN_POINT('Ctrl Pts',(1.92588369818274,6.53528109189779,-7.13572841465908));
#29730=CARTESIAN_POINT('Ctrl Pts',(1.95647853330762,6.52671490024969,-7.18872022360712));
#29731=CARTESIAN_POINT('Ctrl Pts',(1.98733784099078,6.51798285441075,-7.24217011240074));
#29732=CARTESIAN_POINT('Ctrl Pts',(2.15286381690566,6.47114510859792,-7.52886951265766));
#29733=CARTESIAN_POINT('Ctrl Pts',(2.32600373553534,6.41959121679276,-7.82875664840512));
#29734=CARTESIAN_POINT('Ctrl Pts',(2.50587483237852,6.36282325692957,-8.14030252705253));
#29735=CARTESIAN_POINT('Ctrl Pts',(2.57414529434987,6.34127685557299,-8.25855043588178));
#29736=CARTESIAN_POINT('Ctrl Pts',(2.64338533227658,6.31897976149477,-8.3784776994861));
#29737=CARTESIAN_POINT('Ctrl Pts',(2.71354626504585,6.295906630069,-8.49999999974909));
#29738=CARTESIAN_POINT('Origin',(3.002221399786,0.,-9.));
#29739=CARTESIAN_POINT('',(3.386180225107E-13,5.244818327676,-3.800000000001));
#29740=CARTESIAN_POINT('Ctrl Pts',(0.0734354173720697,5.61504677956584,
-3.92719387396377));
#29741=CARTESIAN_POINT('Ctrl Pts',(0.0689743793199208,5.59710734302576,
-3.91946712940295));
#29742=CARTESIAN_POINT('Ctrl Pts',(0.0646056578481124,5.5784360241764,-3.91190028184966));
#29743=CARTESIAN_POINT('Ctrl Pts',(0.0602886395540653,5.55918434054357,
-3.90442298682717));
#29744=CARTESIAN_POINT('Ctrl Pts',(0.0559715780169001,5.53993246406866,
-3.8969456169054));
#29745=CARTESIAN_POINT('Ctrl Pts',(0.0517062206933113,5.52010021118334,
-3.88955780130851));
#29746=CARTESIAN_POINT('Ctrl Pts',(0.0474222609735764,5.49942329140985,
-3.88213776541635));
#29747=CARTESIAN_POINT('Ctrl Pts',(0.0431383012538383,5.47874637163634,
-3.87471772952418));
#29748=CARTESIAN_POINT('Ctrl Pts',(0.0388357391379535,5.45722478497467,
-3.86726547333675));
#29749=CARTESIAN_POINT('Ctrl Pts',(0.034760148805027,5.4362886991235,-3.86020634380928));
#29750=CARTESIAN_POINT('Ctrl Pts',(0.0306845584721015,5.41535261327233,
-3.85314721428182));
#29751=CARTESIAN_POINT('Ctrl Pts',(0.0268359399221341,5.39500202823166,
-3.84648121141432));
#29752=CARTESIAN_POINT('Ctrl Pts',(0.0230645959593961,5.37465460666466,
-3.83994905205804));
#29753=CARTESIAN_POINT('Ctrl Pts',(0.0192932519966604,5.35430718509767,
-3.83341689270177));
#29754=CARTESIAN_POINT('Ctrl Pts',(0.0155991826211542,5.33396292700434,
-3.82701857685671));
#29755=CARTESIAN_POINT('Ctrl Pts',(0.011776540402697,5.31245424544518,-3.82039756631518));
#29756=CARTESIAN_POINT('Ctrl Pts',(0.00795389818423762,5.29094556388601,
-3.81377655577365));
#29757=CARTESIAN_POINT('Ctrl Pts',(0.0040026831228265,5.268272458861,-3.80693285053566));
#29758=CARTESIAN_POINT('Ctrl Pts',(3.76143560743003E-13,5.244818327676,
-3.80000000000098));
#29759=CARTESIAN_POINT('',(2.713546265044,1.304093369931,-8.499999999745));
#29760=CARTESIAN_POINT('',(2.713546265046,6.295906630069,-8.499999999749));
#29761=CARTESIAN_POINT('',(0.133974522815126,0.66485875628202,-4.03205067311006));
#29762=CARTESIAN_POINT('Ctrl Pts',(2.71354626504418,1.304093369931,-8.4999999997449));
#29763=CARTESIAN_POINT('Ctrl Pts',(2.61159997231137,1.27056729429867,-8.3234238410882));
#29764=CARTESIAN_POINT('Ctrl Pts',(2.50910501193143,1.2378821522437,-8.14589736143207));
#29765=CARTESIAN_POINT('Ctrl Pts',(2.40674837211237,1.20622891171289,-7.96861045946304));
#29766=CARTESIAN_POINT('Ctrl Pts',(2.30924947494878,1.17607790198004,-7.79973741464557));
#29767=CARTESIAN_POINT('Ctrl Pts',(2.21187614287338,1.14686278150517,-7.63108185950621));
#29768=CARTESIAN_POINT('Ctrl Pts',(2.11522487961953,1.11870492115182,-7.46367696093502));
#29769=CARTESIAN_POINT('Ctrl Pts',(2.09351075323304,1.11237884410014,-7.42606699079168));
#29770=CARTESIAN_POINT('Ctrl Pts',(2.07183288047179,1.10610895833824,-7.38851981327021));
#29771=CARTESIAN_POINT('Ctrl Pts',(2.05017111365136,1.09988905714736,-7.3510005318615));
#29772=CARTESIAN_POINT('Ctrl Pts',(1.97331024742889,1.07781943571198,-7.21787360398792));
#29773=CARTESIAN_POINT('Ctrl Pts',(1.89665242668735,1.05637516593552,-7.08509835967507));
#29774=CARTESIAN_POINT('Ctrl Pts',(1.81929488308289,1.0353118673009,-6.95111116385844));
#29775=CARTESIAN_POINT('Ctrl Pts',(1.74288942113456,1.01450780621848,-6.81877302184251));
#29776=CARTESIAN_POINT('Ctrl Pts',(1.665801326986,0.994075360144622,-6.68525252998749));
#29777=CARTESIAN_POINT('Ctrl Pts',(1.58715752976534,0.973829251194698,-6.54903747990535));
#29778=CARTESIAN_POINT('Ctrl Pts',(1.5631206815207,0.967641189763631,-6.50740443822663));
#29779=CARTESIAN_POINT('Ctrl Pts',(1.53893848254314,0.96147089723312,-6.46551964148831));
#29780=CARTESIAN_POINT('Ctrl Pts',(1.51458594875602,0.95531405854845,-6.42333981567596));
#29781=CARTESIAN_POINT('Ctrl Pts',(1.46961768989598,0.943945125929286,-6.34545250660246));
#29782=CARTESIAN_POINT('Ctrl Pts',(1.42406936453429,0.932612495198426,-6.26656049131749));
#29783=CARTESIAN_POINT('Ctrl Pts',(1.37795947539797,0.921336565457625,-6.18669581966957));
#29784=CARTESIAN_POINT('Ctrl Pts',(1.22462045111637,0.883838317322376,-5.9211048357299));
#29785=CARTESIAN_POINT('Ctrl Pts',(1.06507017471814,0.846970542877258,-5.64475565567324));
#29786=CARTESIAN_POINT('Ctrl Pts',(0.899997396731987,0.811456784908397,
-5.35884121775675));
#29787=CARTESIAN_POINT('Ctrl Pts',(0.885732238628493,0.808387778749686,
-5.33413323918689));
#29788=CARTESIAN_POINT('Ctrl Pts',(0.871425846050205,0.805328855185408,
-5.3093538403878));
#29789=CARTESIAN_POINT('Ctrl Pts',(0.857078667709878,0.802280463959259,
-5.28450379855709));
#29790=CARTESIAN_POINT('Ctrl Pts',(0.782414631538548,0.786416355534968,
-5.15518189441013));
#29791=CARTESIAN_POINT('Ctrl Pts',(0.706645722013296,0.77084087237109,-5.02394629316002));
#29792=CARTESIAN_POINT('Ctrl Pts',(0.629748301253577,0.755591732168624,
-4.89075605342435));
#29793=CARTESIAN_POINT('Ctrl Pts',(0.469464328013554,0.723806624735922,
-4.61313606811522));
#29794=CARTESIAN_POINT('Ctrl Pts',(0.304277117249445,0.693436027781902,
-4.32702342665655));
#29795=CARTESIAN_POINT('Ctrl Pts',(0.133974596315389,0.6648587720723,-4.03205080774139));
#29796=CARTESIAN_POINT('',(0.1339745962156,1.347528370654,-4.032050807569));
#29797=CARTESIAN_POINT('',(0.1339745962156,1.347528370654,-4.032050807569));
#29798=CARTESIAN_POINT('',(0.073424843718969,1.98498956165576,-3.92717625701886));
#29799=CARTESIAN_POINT('Origin',(-0.147569422083157,1.04172484501738,-3.54440667724998));
#29800=CARTESIAN_POINT('',(-1.29347819189345E-8,2.3551814754037,-3.79999997759638));
#29801=CARTESIAN_POINT('Origin',(-0.118328490245077,4.15913738516639,-3.59504904291298));
#29802=CARTESIAN_POINT('',(0.144337567297357,3.80000000094331,-4.05000000000003));
#29803=CARTESIAN_POINT('Ctrl Pts',(0.1443375672974,3.799999999999,-4.05));
#29804=CARTESIAN_POINT('Ctrl Pts',(0.1443378988472,3.641734883366,-4.050000360009));
#29805=CARTESIAN_POINT('Ctrl Pts',(0.1338002849907,3.32390084097,-4.031748979448));
#29806=CARTESIAN_POINT('Ctrl Pts',(0.09119286281607,2.871512797023,-3.957950685846));
#29807=CARTESIAN_POINT('Ctrl Pts',(0.03592693705457,2.529613680379,-3.86222718878));
#29808=CARTESIAN_POINT('Ctrl Pts',(1.940475558015E-12,2.35518167234,-3.800000000003));
#29809=CARTESIAN_POINT('Ctrl Pts',(3.386180225107E-13,5.244818327676,-3.800000000001));
#29810=CARTESIAN_POINT('Ctrl Pts',(0.03068642401925,5.095833738666,-3.85315021964));
#29811=CARTESIAN_POINT('Ctrl Pts',(0.08230825724947,4.790451591005,-3.942562156105));
#29812=CARTESIAN_POINT('Ctrl Pts',(0.1295377956624,4.345878065346,-4.024366128052));
#29813=CARTESIAN_POINT('Ctrl Pts',(0.1443374902468,3.988290562368,-4.049999621017));
#29814=CARTESIAN_POINT('Ctrl Pts',(0.1443375672974,3.799999999999,-4.05));
#29815=CARTESIAN_POINT('Ctrl Pts',(-0.01984074734411,5.778719106975,-3.658132002503));
#29816=CARTESIAN_POINT('Ctrl Pts',(-0.02151789291509,5.772219745287,-3.655227101155));
#29817=CARTESIAN_POINT('Ctrl Pts',(-0.02874571800289,5.743664386755,-3.642708140867));
#29818=CARTESIAN_POINT('Ctrl Pts',(-0.04083585898923,5.692008838292,-3.621767402488));
#29819=CARTESIAN_POINT('Ctrl Pts',(-0.05561412281504,5.623164700404,-3.596170698722));
#29820=CARTESIAN_POINT('Ctrl Pts',(-0.06929848073128,5.554723990994,-3.572468695329));
#29821=CARTESIAN_POINT('Ctrl Pts',(-0.08205687983033,5.487371187967,-3.55037050065));
#29822=CARTESIAN_POINT('Ctrl Pts',(-0.0944087317008,5.419259193829,-3.528976462696));
#29823=CARTESIAN_POINT('Ctrl Pts',(-0.1033895478633,5.367635088747,-3.513421241507));
#29824=CARTESIAN_POINT('Ctrl Pts',(-0.1084344694084,5.33794230972,-3.504684713301));
#29825=CARTESIAN_POINT('Ctrl Pts',(-0.1093975902414,5.332248875779,-3.503016900451));
#29826=CARTESIAN_POINT('Ctrl Pts',(-0.002985157552623,5.726476579393,-3.765100576803));
#29827=CARTESIAN_POINT('Ctrl Pts',(-0.004518714363548,5.720537561251,-3.762444378488));
#29828=CARTESIAN_POINT('Ctrl Pts',(-0.01117002684806,5.694267120759,-3.750923967326));
#29829=CARTESIAN_POINT('Ctrl Pts',(-0.02257083122652,5.645585694094,-3.731177194912));
#29830=CARTESIAN_POINT('Ctrl Pts',(-0.03671407770094,5.579712000861,-3.706680373465));
#29831=CARTESIAN_POINT('Ctrl Pts',(-0.04994669756034,5.513541725306,-3.68376080341));
#29832=CARTESIAN_POINT('Ctrl Pts',(-0.06239188724486,5.447846771628,-3.662205103075));
#29833=CARTESIAN_POINT('Ctrl Pts',(-0.0744755782777,5.381214825156,-3.641275534353));
#29834=CARTESIAN_POINT('Ctrl Pts',(-0.08329239205763,5.330536275783,-3.626004370564));
#29835=CARTESIAN_POINT('Ctrl Pts',(-0.08824062183765,5.301408245067,-3.617434778462));
#29836=CARTESIAN_POINT('Ctrl Pts',(-0.0891849730255,5.295824591682,-3.615799348484));
#29837=CARTESIAN_POINT('Ctrl Pts',(0.03425994679476,5.671886279934,-3.865541747954));
#29838=CARTESIAN_POINT('Ctrl Pts',(0.03287643160393,5.666532787098,-3.863145429351));
#29839=CARTESIAN_POINT('Ctrl Pts',(0.02682754011999,5.642649948543,-3.852668441972));
#29840=CARTESIAN_POINT('Ctrl Pts',(0.01614705102297,5.597076300293,-3.834169292197));
#29841=CARTESIAN_POINT('Ctrl Pts',(0.002667359496765,5.534306543082,-3.810821781622));
#29842=CARTESIAN_POINT('Ctrl Pts',(-0.01009322126234,5.470508734362,-3.78871980735));
#29843=CARTESIAN_POINT('Ctrl Pts',(-0.02221112594464,5.406546133551,-3.76773098098));
#29844=CARTESIAN_POINT('Ctrl Pts',(-0.03401460502959,5.34146074788,-3.747286754671));
#29845=CARTESIAN_POINT('Ctrl Pts',(-0.04266004618244,5.291770247358,-3.732312413783));
#29846=CARTESIAN_POINT('Ctrl Pts',(-0.04750725449303,5.263232420449,-3.723917232833));
#29847=CARTESIAN_POINT('Ctrl Pts',(-0.04843199622471,5.257763499078,-3.72231563461));
#29848=CARTESIAN_POINT('Ctrl Pts',(0.09069940064414,5.616699966831,-3.956232440606));
#29849=CARTESIAN_POINT('Ctrl Pts',(0.08946756522009,5.611938392032,-3.954098839065));
#29850=CARTESIAN_POINT('Ctrl Pts',(0.08402767193487,5.590469223109,-3.944676667507));
#29851=CARTESIAN_POINT('Ctrl Pts',(0.07407536246235,5.548037283815,-3.92743876185));
#29852=CARTESIAN_POINT('Ctrl Pts',(0.06126647054354,5.488405351215,-3.905253110252));
#29853=CARTESIAN_POINT('Ctrl Pts',(0.04898308257803,5.427005911782,-3.883977658227));
#29854=CARTESIAN_POINT('Ctrl Pts',(0.03719603617657,5.364794577562,-3.863561894917));
#29855=CARTESIAN_POINT('Ctrl Pts',(0.02567582837665,5.301272637951,-3.843608309962));
#29856=CARTESIAN_POINT('Ctrl Pts',(0.01720363088747,5.252580973739,-3.828934032668));
#29857=CARTESIAN_POINT('Ctrl Pts',(0.01245853205391,5.224639866974,-3.820715141208));
#29858=CARTESIAN_POINT('Ctrl Pts',(0.01155361033798,5.219286947419,-3.819147737991));
#29859=CARTESIAN_POINT('Ctrl Pts',(-0.0201784110928209,5.74664992548515,
-3.67573593484731));
#29860=CARTESIAN_POINT('Ctrl Pts',(-0.0201784354696587,5.74664939526823,
-3.67573612144244));
#29861=CARTESIAN_POINT('Ctrl Pts',(-0.0201784598462801,5.74664886505137,
-3.67573630803726));
#29862=CARTESIAN_POINT('Ctrl Pts',(-0.020178484222685,5.7466483348346,-3.67573649463177));
#29863=CARTESIAN_POINT('Ctrl Pts',(-0.0209814232443088,5.72918342386011,
-3.68188276676627));
#29864=CARTESIAN_POINT('Ctrl Pts',(-0.0215496981580626,5.71179450558293,
-3.68769910806057));
#29865=CARTESIAN_POINT('Ctrl Pts',(-0.0219239143907458,5.69464667663326,
-3.69319344038992));
#29866=CARTESIAN_POINT('Ctrl Pts',(-0.0222159929576374,5.68126266795729,
-3.69748180784334));
#29867=CARTESIAN_POINT('Ctrl Pts',(-0.0223899043208644,5.66802664780854,
-3.70157408075059));
#29868=CARTESIAN_POINT('Ctrl Pts',(-0.0224622993826163,5.65503849956244,
-3.70548017730559));
#29869=CARTESIAN_POINT('Ctrl Pts',(-0.0224623092421808,5.655036730692,-3.70548070928125));
#29870=CARTESIAN_POINT('Ctrl Pts',(-0.0224623190998546,5.65503496182611,
-3.7054812412535));
#29871=CARTESIAN_POINT('Ctrl Pts',(-0.0224623289556378,5.65503319296475,
-3.70548177322234));
#29872=CARTESIAN_POINT('Ctrl Pts',(-0.0225576168824433,5.63793144391809,
-3.7106249675194));
#29873=CARTESIAN_POINT('Ctrl Pts',(-0.0224803444260501,5.6212524460535,
-3.7154476654276));
#29874=CARTESIAN_POINT('Ctrl Pts',(-0.0222698926513762,5.60469313910181,
-3.72006135912167));
#29875=CARTESIAN_POINT('Ctrl Pts',(-0.0221157521730552,5.59256466217092,
-3.72344055111915));
#29876=CARTESIAN_POINT('Ctrl Pts',(-0.0218890281308965,5.58050088128577,
-3.72670819678444));
#29877=CARTESIAN_POINT('Ctrl Pts',(-0.021590073938272,5.56838931652737,
-3.72991372001025));
#29878=CARTESIAN_POINT('Ctrl Pts',(-0.0210930236774006,5.54825226352312,
-3.73524331964433));
#29879=CARTESIAN_POINT('Ctrl Pts',(-0.0203949237649873,5.52797573110029,
-3.74038852222518));
#29880=CARTESIAN_POINT('Ctrl Pts',(-0.019546685278498,5.50816848599496,
-3.74523501469395));
#29881=CARTESIAN_POINT('Ctrl Pts',(-0.0191881341317336,5.49979594624361,
-3.74728363128013));
#29882=CARTESIAN_POINT('Ctrl Pts',(-0.0188034447277056,5.49150724371414,
-3.7492787304572));
#29883=CARTESIAN_POINT('Ctrl Pts',(-0.0183991125698059,5.48334826563006,
-3.75121139305542));
#29884=CARTESIAN_POINT('Ctrl Pts',(-0.0183990893589477,5.48334779726048,
-3.75121150400073));
#29885=CARTESIAN_POINT('Ctrl Pts',(-0.0183990661480251,5.48334732889133,
-3.75121161494584));
#29886=CARTESIAN_POINT('Ctrl Pts',(-0.0183990429370381,5.4833468605226,
-3.75121172589074));
#29887=CARTESIAN_POINT('Ctrl Pts',(-0.0174959282178277,5.46512313347947,
-3.75552847352253));
#29888=CARTESIAN_POINT('Ctrl Pts',(-0.0164952009111264,5.44755019954919,
-3.75954106424298));
#29889=CARTESIAN_POINT('Ctrl Pts',(-0.0154116253866607,5.43029031610371,
-3.7633559520826));
#29890=CARTESIAN_POINT('Ctrl Pts',(-0.0148623564371937,5.42154120924962,
-3.76528973462815));
#29891=CARTESIAN_POINT('Ctrl Pts',(-0.0142910671327694,5.41287304683532,
-3.7671729788354));
#29892=CARTESIAN_POINT('Ctrl Pts',(-0.0136956716655769,5.40424442836318,
-3.76902069403971));
#29893=CARTESIAN_POINT('Ctrl Pts',(-0.0123428919870068,5.38463961044561,
-3.77321883077051));
#29894=CARTESIAN_POINT('Ctrl Pts',(-0.0108709353686572,5.36523333453026,
-3.77723016957813));
#29895=CARTESIAN_POINT('Ctrl Pts',(-0.00924390264763095,5.34538151671619,
-3.78118265844034));
#29896=CARTESIAN_POINT('Ctrl Pts',(-0.00874213708005937,5.33925935426422,
-3.78240157849747));
#29897=CARTESIAN_POINT('Ctrl Pts',(-0.00822524663056512,5.33309483828452,
-3.78361490643188));
#29898=CARTESIAN_POINT('Ctrl Pts',(-0.00769119476733997,5.32686912636376,
-3.78482636825632));
#29899=CARTESIAN_POINT('Ctrl Pts',(-0.00576649863884664,5.30443197286591,
-3.78919241590802));
#29900=CARTESIAN_POINT('Ctrl Pts',(-0.00361826650166239,5.28120087535866,
-3.79352982465151));
#29901=CARTESIAN_POINT('Ctrl Pts',(-0.00126811120227719,5.25747582420667,
-3.79776089073069));
#29902=CARTESIAN_POINT('Ctrl Pts',(-0.000851633964029754,5.2532714451243,
-3.79851068914442));
#29903=CARTESIAN_POINT('Ctrl Pts',(-0.00042886831096522,5.24905166975247,
-3.79925718508722));
#29904=CARTESIAN_POINT('Ctrl Pts',(4.14410515212417E-13,5.244818327676,
-3.80000000000096));
#29905=CARTESIAN_POINT('Ctrl Pts',(-0.01268225407336,5.772800830803,-3.694029050448));
#29906=CARTESIAN_POINT('Ctrl Pts',(-0.01301759475994,5.739068753102,-3.712030303038));
#29907=CARTESIAN_POINT('Ctrl Pts',(-0.01039416813831,5.648078305665,-3.759169807315));
#29908=CARTESIAN_POINT('Ctrl Pts',(0.007243773431018,5.489308134892,-3.83432961623));
#29909=CARTESIAN_POINT('Ctrl Pts',(0.03200461319616,5.356083219744,-3.889613921073));
#29910=CARTESIAN_POINT('Ctrl Pts',(0.04752295287887,5.284287176484,-3.917085317952));
#29911=CARTESIAN_POINT('Ctrl Pts',(0.04864194797635,5.279159326484,-3.919035833836));
#29912=CARTESIAN_POINT('Ctrl Pts',(-0.06997922621458,5.655780000582,-3.474398901289));
#29913=CARTESIAN_POINT('Ctrl Pts',(-0.07032635079946,5.623484779779,-3.49163753327));
#29914=CARTESIAN_POINT('Ctrl Pts',(-0.06761185683549,5.536547101997,-3.536642069158));
#29915=CARTESIAN_POINT('Ctrl Pts',(-0.04957369418306,5.385410837322,-3.607995938579));
#29916=CARTESIAN_POINT('Ctrl Pts',(-0.02442010904563,5.258978615888,-3.660231095361));
#29917=CARTESIAN_POINT('Ctrl Pts',(-0.008697108721838,5.190924849655,-3.686137282999));
#29918=CARTESIAN_POINT('Ctrl Pts',(-0.007563539672665,5.186064676355,-3.687976401988));
#29919=CARTESIAN_POINT('Ctrl Pts',(-0.2743702068952,5.585058547127,-3.338610219652));
#29920=CARTESIAN_POINT('Ctrl Pts',(-0.2747593672533,5.550259551039,-3.357212409689));
#29921=CARTESIAN_POINT('Ctrl Pts',(-0.2717200159241,5.457732776618,-3.404879810051));
#29922=CARTESIAN_POINT('Ctrl Pts',(-0.2522541760907,5.300544900304,-3.477833556881));
#29923=CARTESIAN_POINT('Ctrl Pts',(-0.2256995812873,5.171582624003,-3.529601984754));
#29924=CARTESIAN_POINT('Ctrl Pts',(-0.209246511161,5.102702800412,-3.554946751412));
#29925=CARTESIAN_POINT('Ctrl Pts',(-0.2080609536006,5.097786222214,-3.556744268162));
#29926=CARTESIAN_POINT('Ctrl Pts',(-0.5292956670922,5.5940470946,-3.350813053167));
#29927=CARTESIAN_POINT('Ctrl Pts',(-0.5297372563238,5.553986538552,-3.372260800208));
#29928=CARTESIAN_POINT('Ctrl Pts',(-0.5262927285377,5.448869233457,-3.426130892594));
#29929=CARTESIAN_POINT('Ctrl Pts',(-0.5050462266558,5.274803163949,-3.505334510713));
#29930=CARTESIAN_POINT('Ctrl Pts',(-0.4767442307066,5.135183346856,-3.559439123509));
#29931=CARTESIAN_POINT('Ctrl Pts',(-0.4593805852712,5.061299382153,-3.585491487082));
#29932=CARTESIAN_POINT('Ctrl Pts',(-0.458130185343,5.056028964579,-3.587336850212));
#29933=CARTESIAN_POINT('',(-0.4330127018922,5.076816196554,-3.579069767442));
#29934=CARTESIAN_POINT('Origin',(-0.4330127019006,5.244818327721,-4.049999999986));
#29935=CARTESIAN_POINT('Ctrl Pts',(-0.5000021724644,5.578412269071,-3.358161259976));
#29936=CARTESIAN_POINT('Ctrl Pts',(-0.5000045975026,5.526517536485,-3.385642436917));
#29937=CARTESIAN_POINT('Ctrl Pts',(-0.4942244627249,5.419967689217,-3.438990063122));
#29938=CARTESIAN_POINT('Ctrl Pts',(-0.4708077496976,5.252312611015,-3.513147270451));
#29939=CARTESIAN_POINT('Ctrl Pts',(-0.4468343747841,5.13611833078,-3.557914058777));
#29940=CARTESIAN_POINT('Ctrl Pts',(-0.4330127018922,5.076816196554,-3.579069767442));
#29941=CARTESIAN_POINT('Origin',(0.,3.8,0.));
#29942=CARTESIAN_POINT('',(-0.3268619336444,0.437875148065591,-1.77090837708039));
#29943=CARTESIAN_POINT('',(-4.03990376683404E-8,0.000376013360896276,-0.053456151853531));
#29944=CARTESIAN_POINT('Ctrl Pts',(-0.326861921820454,0.437875149890247,
-1.77090838054216));
#29945=CARTESIAN_POINT('Ctrl Pts',(-0.319542282990462,0.427568175634498,
-1.75134026812288));
#29946=CARTESIAN_POINT('Ctrl Pts',(-0.31241176881403,0.417107419064298,
-1.73105973218862));
#29947=CARTESIAN_POINT('Ctrl Pts',(-0.305543769648105,0.40674449660338,
-1.71050199902501));
#29948=CARTESIAN_POINT('Ctrl Pts',(-0.299865103021684,0.398176123120899,
-1.69350425187759));
#29949=CARTESIAN_POINT('Ctrl Pts',(-0.294365904146456,0.389669138737853,
-1.67631988987948));
#29950=CARTESIAN_POINT('Ctrl Pts',(-0.288814745499404,0.380887794442087,
-1.65821341382975));
#29951=CARTESIAN_POINT('Ctrl Pts',(-0.287652050165285,0.379048533723895,
-1.65442099560521));
#29952=CARTESIAN_POINT('Ctrl Pts',(-0.286487075372004,0.377197400306006,
-1.65058804734057));
#29953=CARTESIAN_POINT('Ctrl Pts',(-0.28531769463674,0.375331578522012,
-1.64670768593927));
#29954=CARTESIAN_POINT('Ctrl Pts',(-0.278565236555438,0.3645575996085,-1.62430097364065));
#29955=CARTESIAN_POINT('Ctrl Pts',(-0.271665868697669,0.353295923028537,
-1.60031225523217));
#29956=CARTESIAN_POINT('Ctrl Pts',(-0.264753638980834,0.341806749440673,
-1.57508712196688));
#29957=CARTESIAN_POINT('Ctrl Pts',(-0.257841409264,0.330317575852808,-1.54986198870159));
#29958=CARTESIAN_POINT('Ctrl Pts',(-0.2509163176881,0.318596673571711,-1.52340229432317));
#29959=CARTESIAN_POINT('Ctrl Pts',(-0.243933082800515,0.30663613302955,
-1.49546276882618));
#29960=CARTESIAN_POINT('Ctrl Pts',(-0.23694984791293,0.294675592487389,
-1.46752324332919));
#29961=CARTESIAN_POINT('Ctrl Pts',(-0.22990846971366,0.282477015449631,
-1.43810324340019));
#29962=CARTESIAN_POINT('Ctrl Pts',(-0.222822150024723,0.270145781900204,
-1.40717063605061));
#29963=CARTESIAN_POINT('Ctrl Pts',(-0.215735830335797,0.257814548350794,
-1.37623802870107));
#29964=CARTESIAN_POINT('Ctrl Pts',(-0.208604569157203,0.245348810589579,
-1.34379351988624));
#29965=CARTESIAN_POINT('Ctrl Pts',(-0.20139409589261,0.232798729978922,
-1.30960875804952));
#29966=CARTESIAN_POINT('Ctrl Pts',(-0.194183622628007,0.220248649368249,
-1.27542399621276));
#29967=CARTESIAN_POINT('Ctrl Pts',(-0.186893937277403,0.207614742487103,
-1.23949884094976));
#29968=CARTESIAN_POINT('Ctrl Pts',(-0.179513347151867,0.195008186424988,
-1.20167966782215));
#29969=CARTESIAN_POINT('Ctrl Pts',(-0.17213275702633,0.182401630362873,
-1.16386049469453));
#29970=CARTESIAN_POINT('Ctrl Pts',(-0.16466126212586,0.169824308636727,
-1.12414663060252));
#29971=CARTESIAN_POINT('Ctrl Pts',(-0.157115542594206,0.157467963405492,
-1.08257118120827));
#29972=CARTESIAN_POINT('Ctrl Pts',(-0.149569823062563,0.145111618174274,
-1.04099573181408));
#29973=CARTESIAN_POINT('Ctrl Pts',(-0.141949878899737,0.132972291505805,
-0.997559839050705));
#29974=CARTESIAN_POINT('Ctrl Pts',(-0.134207247927528,0.121174400699684,
-0.951967546680385));
#29975=CARTESIAN_POINT('Ctrl Pts',(-0.127569153529385,0.111059555610061,
-0.912879290806096));
#29976=CARTESIAN_POINT('Ctrl Pts',(-0.120840879677674,0.101195125658457,
-0.872206528992164));
#29977=CARTESIAN_POINT('Ctrl Pts',(-0.113972151341684,0.0916740642261438,
-0.829649777958719));
#29978=CARTESIAN_POINT('Ctrl Pts',(-0.112829238751193,0.0900898203234105,
-0.822568605988117));
#29979=CARTESIAN_POINT('Ctrl Pts',(-0.1116824374202,0.0885152001390327,
-0.815435269714428));
#29980=CARTESIAN_POINT('Ctrl Pts',(-0.110531515736002,0.0869507755337904,
-0.808248387991514));
#29981=CARTESIAN_POINT('Ctrl Pts',(-0.104093298235906,0.0781994364901921,
-0.768045211428898));
#29982=CARTESIAN_POINT('Ctrl Pts',(-0.0975261447367866,0.0697631999578778,
-0.726167000035645));
#29983=CARTESIAN_POINT('Ctrl Pts',(-0.0907979124502509,0.0617629058426914,
-0.682336740815209));
#29984=CARTESIAN_POINT('Ctrl Pts',(-0.0890949413787892,0.0597379654332153,
-0.671242940790433));
#29985=CARTESIAN_POINT('Ctrl Pts',(-0.0873816509906677,0.057741210889608,
-0.660024094936211));
#29986=CARTESIAN_POINT('Ctrl Pts',(-0.0856575200882579,0.0557751425005906,
-0.648675740631271));
#29987=CARTESIAN_POINT('Ctrl Pts',(-0.0780501822835085,0.0471003102349018,
-0.59860369296656));
#29988=CARTESIAN_POINT('Ctrl Pts',(-0.0702317996002882,0.0390194097716542,
-0.546009698564737));
#29989=CARTESIAN_POINT('Ctrl Pts',(-0.0621404289527874,0.0318265887957336,
-0.490784212351215));
#29990=CARTESIAN_POINT('Ctrl Pts',(-0.0611527179057972,0.0309485634219814,
-0.484042854775988));
#29991=CARTESIAN_POINT('Ctrl Pts',(-0.0601609390631264,0.03008383072053,
-0.477262309173059));
#29992=CARTESIAN_POINT('Ctrl Pts',(-0.0591649797527023,0.0292329757968122,
-0.470442397304746));
#29993=CARTESIAN_POINT('Ctrl Pts',(-0.0514071364498713,0.0226053966351349,
-0.417319938325012));
#29994=CARTESIAN_POINT('Ctrl Pts',(-0.0433956496731836,0.0168161405436987,
-0.361807975160488));
#29995=CARTESIAN_POINT('Ctrl Pts',(-0.0351244935793345,0.0121644665601162,
-0.303812395418932));
#29996=CARTESIAN_POINT('Ctrl Pts',(-0.0336349978225925,0.0113267785051844,
-0.29336836934148));
#29997=CARTESIAN_POINT('Ctrl Pts',(-0.0321370810062191,0.0105261042260805,
-0.282843860181119));
#29998=CARTESIAN_POINT('Ctrl Pts',(-0.0306307079387777,0.00976435400706599,
-0.272238402589581));
#29999=CARTESIAN_POINT('Ctrl Pts',(-0.0215805482745863,0.00518782429120783,
-0.208521726694507));
#30000=CARTESIAN_POINT('Ctrl Pts',(-0.012225159981005,0.00201431597951373,
-0.141880460699178));
#30001=CARTESIAN_POINT('Ctrl Pts',(-0.00262039848169704,0.000690311987880055,
-0.0724285480818705));
#30002=CARTESIAN_POINT('Ctrl Pts',(-0.00174900083682787,0.000570190945812525,
-0.0661274823978614));
#30003=CARTESIAN_POINT('Ctrl Pts',(-0.000875550568057551,0.00046531029951653,
-0.0598033132919511));
#30004=CARTESIAN_POINT('Ctrl Pts',(-8.93867835446334E-8,0.000376013267725295,
-0.0534561450979849));
#30005=CARTESIAN_POINT('',(-1.33322010970278E-6,0.000376061138413409,0.0534595472478362));
#30006=CARTESIAN_POINT('Ctrl Pts',(-6.386159645368E-8,0.000376010664161264,
-0.0534559600381995));
#30007=CARTESIAN_POINT('Ctrl Pts',(-0.001454973133866,0.000313323311071578,
-0.0490001730603571));
#30008=CARTESIAN_POINT('Ctrl Pts',(-0.002708403504571,0.000259316092946519,
-0.0446031753896197));
#30009=CARTESIAN_POINT('Ctrl Pts',(-0.0037727890176825,0.00021347008401007,
-0.040278121468098));
#30010=CARTESIAN_POINT('Ctrl Pts',(-0.004837174530794,0.000167624075073621,
-0.0359530675465762));
#30011=CARTESIAN_POINT('Ctrl Pts',(-0.005712515186312,0.000129899434652782,
-0.0316999576221515));
#30012=CARTESIAN_POINT('Ctrl Pts',(-0.00641840706118967,9.94838426637834E-5,
-0.027496678112308));
#30013=CARTESIAN_POINT('Ctrl Pts',(-0.00712429893606733,6.90682506747847E-5,
-0.0232933986024644));
#30014=CARTESIAN_POINT('Ctrl Pts',(-0.00766074203030467,4.59440949101007E-5,
-0.0191399497061853));
#30015=CARTESIAN_POINT('Ctrl Pts',(-0.008040469737835,2.95933637711743E-5,
-0.0149969559875762));
#30016=CARTESIAN_POINT('Ctrl Pts',(-0.00842019744536534,1.32426326322479E-5,
-0.010853962268967));
#30017=CARTESIAN_POINT('Ctrl Pts',(-0.00864320976618867,3.62518085065978E-6,
-0.00672142386867571));
#30018=CARTESIAN_POINT('Ctrl Pts',(-0.00870785447653417,8.37616607740621E-7,
-0.00252307065227364));
#30019=CARTESIAN_POINT('Ctrl Pts',(-0.00877249918687967,-1.94994763517854E-6,
0.00167528256412843));
#30020=CARTESIAN_POINT('Ctrl Pts',(-0.00867877628674733,2.10261831921796E-6,
0.00593945050831973));
#30021=CARTESIAN_POINT('Ctrl Pts',(-0.00840122364752867,1.40468953585549E-5,
0.0103322895530075));
#30022=CARTESIAN_POINT('Ctrl Pts',(-0.00812367100831,2.59911723978918E-5,
0.0147251285976952));
#30023=CARTESIAN_POINT('Ctrl Pts',(-0.007662288630005,4.58884199110661E-5,
0.0192466386013889));
#30024=CARTESIAN_POINT('Ctrl Pts',(-0.006982466553949,7.51792644959615E-5,
0.0239030700590784));
#30025=CARTESIAN_POINT('Ctrl Pts',(-0.006302644477893,0.000104470109080857,
0.028559501516768));
#30026=CARTESIAN_POINT('Ctrl Pts',(-0.005404382704086,0.00014315841789564,
0.0333508544250512));
#30027=CARTESIAN_POINT('Ctrl Pts',(-0.00425226433895525,0.000192812210902948,
0.0382797025368775));
#30028=CARTESIAN_POINT('Ctrl Pts',(-0.0031002340599688,0.000242462207589229,
0.0432081738096228));
#30029=CARTESIAN_POINT('Ctrl Pts',(-0.00169438600579797,0.000303103761307874,
0.0482741189859386));
#30030=CARTESIAN_POINT('Ctrl Pts',(-1.29817508026421E-6,0.000376060972450354,
0.0534595358076361));
#30031=CARTESIAN_POINT('',(-0.3268604435632,0.437871921569987,1.77090225146181));
#30032=CARTESIAN_POINT('Ctrl Pts',(-9.098011382209E-7,0.000376077707954448,
0.0534607252664227));
#30033=CARTESIAN_POINT('Ctrl Pts',(-0.00956218302788966,0.00135153777727009,
0.12278977750321));
#30034=CARTESIAN_POINT('Ctrl Pts',(-0.0188675944382579,0.00418251178063798,
0.189245247763867));
#30035=CARTESIAN_POINT('Ctrl Pts',(-0.0278578211264471,0.00841146826043904,
0.252698250846818));
#30036=CARTESIAN_POINT('Ctrl Pts',(-0.0292960008120538,0.00908798060117399,
0.262848920367146));
#30037=CARTESIAN_POINT('Ctrl Pts',(-0.0307261146470735,0.00980032046044534,
0.272922849151112));
#30038=CARTESIAN_POINT('Ctrl Pts',(-0.0321479197748909,0.010546676423365,
0.282919614791902));
#30039=CARTESIAN_POINT('Ctrl Pts',(-0.0401348344435378,0.0147392913405909,
0.339075913973366));
#30040=CARTESIAN_POINT('Ctrl Pts',(-0.0478595619690656,0.020001171173114,
0.39279475688745));
#30041=CARTESIAN_POINT('Ctrl Pts',(-0.0553373273401742,0.0260513509579798,
0.444197697420766));
#30042=CARTESIAN_POINT('Ctrl Pts',(-0.057512014228688,0.0278108668023969,
0.459146722331438));
#30043=CARTESIAN_POINT('Ctrl Pts',(-0.0596658139179924,0.0296373695094689,
0.473900004286979));
#30044=CARTESIAN_POINT('Ctrl Pts',(-0.0617991008907227,0.0315247081520194,
0.488460822104781));
#30045=CARTESIAN_POINT('Ctrl Pts',(-0.0689256003236805,0.0378295878695011,
0.537102969761623));
#30046=CARTESIAN_POINT('Ctrl Pts',(-0.0758231832410947,0.0448090998317559,
0.583595570635645));
#30047=CARTESIAN_POINT('Ctrl Pts',(-0.0825535997623161,0.0522799773424927,
0.628167678070125));
#30048=CARTESIAN_POINT('Ctrl Pts',(-0.0847656203519447,0.0547353580495018,
0.642816759454217));
#30049=CARTESIAN_POINT('Ctrl Pts',(-0.0869595840318742,0.0572442360284669,
0.657258458865084));
#30050=CARTESIAN_POINT('Ctrl Pts',(-0.0891376829985573,0.0598012999793553,
0.671501068028844));
#30051=CARTESIAN_POINT('Ctrl Pts',(-0.0960094214768027,0.067868644490065,
0.716435429101639));
#30052=CARTESIAN_POINT('Ctrl Pts',(-0.10272324972924,0.0764114112181864,
0.759387035815182));
#30053=CARTESIAN_POINT('Ctrl Pts',(-0.109312534271131,0.08530222388455,
0.800637516060127));
#30054=CARTESIAN_POINT('Ctrl Pts',(-0.111166622769007,0.0878039148339511,
0.81224454873079));
#30055=CARTESIAN_POINT('Ctrl Pts',(-0.113010850602073,0.090333482418393,
0.823716907565805));
#30056=CARTESIAN_POINT('Ctrl Pts',(-0.114845961110231,0.0928888168290825,
0.835060881378789));
#30057=CARTESIAN_POINT('Ctrl Pts',(-0.122674528197928,0.10378985345693,
0.883454185019746));
#30058=CARTESIAN_POINT('Ctrl Pts',(-0.13033717192211,0.115155692463132,
0.929509774252189));
#30059=CARTESIAN_POINT('Ctrl Pts',(-0.137873485130416,0.126799435650295,
0.973446256380397));
#30060=CARTESIAN_POINT('Ctrl Pts',(-0.138382141414221,0.127585319009367,
0.976411707404667));
#30061=CARTESIAN_POINT('Ctrl Pts',(-0.138890222206121,0.128372487781146,
0.979367506754383));
#30062=CARTESIAN_POINT('Ctrl Pts',(-0.139397739679552,0.129160892803958,
0.982313722331195));
#30063=CARTESIAN_POINT('Ctrl Pts',(-0.147424697608637,0.141630402289828,
1.02891142531315));
#30064=CARTESIAN_POINT('Ctrl Pts',(-0.155310741595373,0.15440539912281,
1.07311084051338));
#30065=CARTESIAN_POINT('Ctrl Pts',(-0.16306962602991,0.167286308004598,
1.11507454100124));
#30066=CARTESIAN_POINT('Ctrl Pts',(-0.170828510464437,0.180167216886368,
1.15703824148905));
#30067=CARTESIAN_POINT('Ctrl Pts',(-0.178460235346763,0.193153903003862,
1.19676630295696));
#30068=CARTESIAN_POINT('Ctrl Pts',(-0.18598165758879,0.206100818291459,
1.23445885784609));
#30069=CARTESIAN_POINT('Ctrl Pts',(-0.193503079830827,0.219047733579073,
1.27215141273528));
#30070=CARTESIAN_POINT('Ctrl Pts',(-0.200914199432563,0.231953458456882,
1.30780888797803));
#30071=CARTESIAN_POINT('Ctrl Pts',(-0.208273146571748,0.244783459547113,
1.34180302223918));
#30072=CARTESIAN_POINT('Ctrl Pts',(-0.215632093710933,0.257613460637344,
1.37579715650034));
#30073=CARTESIAN_POINT('Ctrl Pts',(-0.222938868387567,0.270373085084809,
1.40812595456548));
#30074=CARTESIAN_POINT('Ctrl Pts',(-0.230130727084885,0.282842535025996,
1.43861161074754));
#30075=CARTESIAN_POINT('Ctrl Pts',(-0.237322585782203,0.295311984967184,
1.4690972669296));
#30076=CARTESIAN_POINT('Ctrl Pts',(-0.244399528500206,0.307485397722405,
1.49774227400769));
#30077=CARTESIAN_POINT('Ctrl Pts',(-0.251454846116976,0.319459465500557,
1.52506969929454));
#30078=CARTESIAN_POINT('Ctrl Pts',(-0.256901118650271,0.328702711516436,
1.54616479576357));
#30079=CARTESIAN_POINT('Ctrl Pts',(-0.262334505016738,0.337825935927688,
1.56647526973609));
#30080=CARTESIAN_POINT('Ctrl Pts',(-0.2679496648376,0.347106534542236,1.58667158422878));
#30081=CARTESIAN_POINT('Ctrl Pts',(-0.269608605929401,0.349848391744766,
1.59263837717569));
#30082=CARTESIAN_POINT('Ctrl Pts',(-0.271283413046643,0.352604303264488,
1.59859506771931));
#30083=CARTESIAN_POINT('Ctrl Pts',(-0.272979105942957,0.355382209947033,
1.6045585936483));
#30084=CARTESIAN_POINT('Ctrl Pts',(-0.278853400615903,0.36500555770221,
1.62521770513763));
#30085=CARTESIAN_POINT('Ctrl Pts',(-0.284978345303742,0.37488926894645,
1.64596018554789));
#30086=CARTESIAN_POINT('Ctrl Pts',(-0.291647922676962,0.385350896245332,
1.66738462816095));
#30087=CARTESIAN_POINT('Ctrl Pts',(-0.293420205285631,0.388130826529165,
1.67307766760241));
#30088=CARTESIAN_POINT('Ctrl Pts',(-0.295230944683588,0.390951814871058,
1.67881873367062));
#30089=CARTESIAN_POINT('Ctrl Pts',(-0.297085656889315,0.393820379335401,
1.68461876748693));
#30090=CARTESIAN_POINT('Ctrl Pts',(-0.3059201512701,0.407484125421129,1.71224589260116));
#30091=CARTESIAN_POINT('Ctrl Pts',(-0.3157523331598,0.422231828276934,1.74120891476497));
#30092=CARTESIAN_POINT('Ctrl Pts',(-0.3268604435632,0.437871921569987,1.77090225146181));
#30093=CARTESIAN_POINT('',(-0.500000000199844,0.97322574578055,2.53955651948966));
#30094=CARTESIAN_POINT('Ctrl Pts',(-0.326860601705563,0.437872144139036,
1.7709026740179));
#30095=CARTESIAN_POINT('Ctrl Pts',(-0.343264928911304,0.460959547950471,
1.81473501139747));
#30096=CARTESIAN_POINT('Ctrl Pts',(-0.358589100390692,0.484717356933362,
1.85775178565521));
#30097=CARTESIAN_POINT('Ctrl Pts',(-0.372741964402922,0.508903336490866,
1.89965332401442));
#30098=CARTESIAN_POINT('Ctrl Pts',(-0.380698914410039,0.522501052829122,
1.92321099019828));
#30099=CARTESIAN_POINT('Ctrl Pts',(-0.388285631095653,0.536233297733624,
1.94641668345229));
#30100=CARTESIAN_POINT('Ctrl Pts',(-0.39548591606965,0.550051242464931,
1.9692214383853));
#30101=CARTESIAN_POINT('Ctrl Pts',(-0.405489578841325,0.569249101964776,
2.00090505629269));
#30102=CARTESIAN_POINT('Ctrl Pts',(-0.414747322949087,0.588607187415817,
2.03181712306189));
#30103=CARTESIAN_POINT('Ctrl Pts',(-0.42335439481679,0.608360124090959,
2.06238573077572));
#30104=CARTESIAN_POINT('Ctrl Pts',(-0.431961466684492,0.628113060766101,
2.09295433848956));
#30105=CARTESIAN_POINT('Ctrl Pts',(-0.439917866312133,0.648261031775009,
2.123179700578));
#30106=CARTESIAN_POINT('Ctrl Pts',(-0.447318840123567,0.669087264136625,
2.15345894792739));
#30107=CARTESIAN_POINT('Ctrl Pts',(-0.45421077773461,0.688481076054676,
2.18165560001105));
#30108=CARTESIAN_POINT('Ctrl Pts',(-0.460621065969921,0.708461418171445,
2.20989678565934));
#30109=CARTESIAN_POINT('Ctrl Pts',(-0.466459965279737,0.729327019690268,
2.23851903007228));
#30110=CARTESIAN_POINT('Ctrl Pts',(-0.472128453601352,0.749583648937855,
2.2663059209886));
#30111=CARTESIAN_POINT('Ctrl Pts',(-0.477258418795676,0.770674668551129,
2.29445219657496));
#30112=CARTESIAN_POINT('Ctrl Pts',(-0.481767751497067,0.792911044852894,
2.32323395632732));
#30113=CARTESIAN_POINT('Ctrl Pts',(-0.482589455892488,0.796963025346541,
2.32847865661062));
#30114=CARTESIAN_POINT('Ctrl Pts',(-0.483390552035199,0.801053140541715,
2.33374436452152));
#30115=CARTESIAN_POINT('Ctrl Pts',(-0.484170543101058,0.805183411400594,
2.33903262068955));
#30116=CARTESIAN_POINT('Ctrl Pts',(-0.490194241371115,0.83708057858172,
2.37987265197359));
#30117=CARTESIAN_POINT('Ctrl Pts',(-0.494959205242138,0.871375098538481,
2.42205463170978));
#30118=CARTESIAN_POINT('Ctrl Pts',(-0.497629691854722,0.908027737205445,
2.46505505642915));
#30119=CARTESIAN_POINT('Ctrl Pts',(-0.499157324262198,0.928994612075099,
2.48965313605516));
#30120=CARTESIAN_POINT('Ctrl Pts',(-0.499999574874154,0.950732289475268,
2.51451910737286));
#30121=CARTESIAN_POINT('Ctrl Pts',(-0.500000000001591,0.973225745780587,
2.53955651948963));
#30122=CARTESIAN_POINT('',(-0.499999999994609,0.973224638042631,-2.53955528646987));
#30123=CARTESIAN_POINT('Origin',(-0.5,3.8,0.));
#30124=CARTESIAN_POINT('Ctrl Pts',(-0.499999999983828,0.973224638043246,
-2.53955528646932));
#30125=CARTESIAN_POINT('Ctrl Pts',(-0.499999467882099,0.941147572377687,
-2.50385035049475));
#30126=CARTESIAN_POINT('Ctrl Pts',(-0.498254574300839,0.910151441566798,
-2.46798114716292));
#30127=CARTESIAN_POINT('Ctrl Pts',(-0.495166769763196,0.880433227438514,
-2.43230957333866));
#30128=CARTESIAN_POINT('Ctrl Pts',(-0.493039810620746,0.859962557593052,
-2.40773807629404));
#30129=CARTESIAN_POINT('Ctrl Pts',(-0.49027566594079,0.84009728363555,-2.38326105062791));
#30130=CARTESIAN_POINT('Ctrl Pts',(-0.487005543648317,0.820889599255338,
-2.35900428574748));
#30131=CARTESIAN_POINT('Ctrl Pts',(-0.483408131607902,0.799759516378343,
-2.33231978583039));
#30132=CARTESIAN_POINT('Ctrl Pts',(-0.479198392185239,0.77942166446121,
-2.30590616238722));
#30133=CARTESIAN_POINT('Ctrl Pts',(-0.474372740319575,0.759556839873406,
-2.27940900016636));
#30134=CARTESIAN_POINT('Ctrl Pts',(-0.469513754567056,0.739554796142232,
-2.25272880497254));
#30135=CARTESIAN_POINT('Ctrl Pts',(-0.464030317974717,0.72003223987174,
-2.22596369837556));
#30136=CARTESIAN_POINT('Ctrl Pts',(-0.457918770674461,0.700704659399275,
-2.19871971650109));
#30137=CARTESIAN_POINT('Ctrl Pts',(-0.456572555292686,0.696447294636109,
-2.19271857380214));
#30138=CARTESIAN_POINT('Ctrl Pts',(-0.455195863561821,0.692199552781376,
-2.18669407899222));
#30139=CARTESIAN_POINT('Ctrl Pts',(-0.453788656365767,0.687958672214371,
-2.18064182619573));
#30140=CARTESIAN_POINT('Ctrl Pts',(-0.445663500202611,0.663472003177413,
-2.14569636880452));
#30141=CARTESIAN_POINT('Ctrl Pts',(-0.436521001197423,0.639212875904072,
-2.10983035256481));
#30142=CARTESIAN_POINT('Ctrl Pts',(-0.426223710361425,0.615068477761928,
-2.0727303728788));
#30143=CARTESIAN_POINT('Ctrl Pts',(-0.418600565927401,0.597194239067346,
-2.04526504164263));
#30144=CARTESIAN_POINT('Ctrl Pts',(-0.410344534688079,0.579383691340677,
-2.01712292969517));
#30145=CARTESIAN_POINT('Ctrl Pts',(-0.401399849929217,0.561607734175777,
-1.98816888936777));
#30146=CARTESIAN_POINT('Ctrl Pts',(-0.385702969888419,0.530412999565221,
-1.93735792062286));
#30147=CARTESIAN_POINT('Ctrl Pts',(-0.367885301289346,0.499330809129928,
-1.88404149274837));
#30148=CARTESIAN_POINT('Ctrl Pts',(-0.347930442098136,0.468787969912562,
-1.82839448987376));
#30149=CARTESIAN_POINT('Ctrl Pts',(-0.34115432792523,0.458416472738944,
-1.80949831820724));
#30150=CARTESIAN_POINT('Ctrl Pts',(-0.334131775937924,0.448106966312162,
-1.79033379514828));
#30151=CARTESIAN_POINT('Ctrl Pts',(-0.3268621439014,0.437875462608086,-1.77090897424662));
#30152=CARTESIAN_POINT('Origin',(0.,3.8,0.));
#30153=CARTESIAN_POINT('',(-1.3332021415609E-6,7.59962393886241,-0.0534595471885383));
#30154=CARTESIAN_POINT('Ctrl Pts',(-9.097914536952E-7,7.5996239222932,-0.0534607251840784));
#30155=CARTESIAN_POINT('Ctrl Pts',(-0.00956218223484543,7.5986484623053,
-0.122789771741156));
#30156=CARTESIAN_POINT('Ctrl Pts',(-0.0188675928807159,7.59581748869241,
-0.189245236636373));
#30157=CARTESIAN_POINT('Ctrl Pts',(-0.0278578188629172,7.5915885328044,
-0.252698234869587));
#30158=CARTESIAN_POINT('Ctrl Pts',(-0.0292959993115927,7.59091202014626,
-0.262848909796949));
#30159=CARTESIAN_POINT('Ctrl Pts',(-0.0307261139013526,7.59019967993104,
-0.272922843907623));
#30160=CARTESIAN_POINT('Ctrl Pts',(-0.0321479197753001,7.58945332357642,
-0.282919614794823));
#30161=CARTESIAN_POINT('Ctrl Pts',(-0.0401348345801153,7.58526070858752,
-0.339075914935605));
#30162=CARTESIAN_POINT('Ctrl Pts',(-0.0478595622363532,7.57999882864497,
-0.39279475874736));
#30163=CARTESIAN_POINT('Ctrl Pts',(-0.0553373277299044,7.57394864872664,
-0.444197700100289));
#30164=CARTESIAN_POINT('Ctrl Pts',(-0.0575120144862837,7.57218913297912,
-0.459146724096235));
#30165=CARTESIAN_POINT('Ctrl Pts',(-0.0596658140459766,7.57036263037731,
-0.473900005160658));
#30166=CARTESIAN_POINT('Ctrl Pts',(-0.0617991008914628,7.56847529184733,
-0.488460822109806));
#30167=CARTESIAN_POINT('Ctrl Pts',(-0.0689256002967675,7.56217041215431,
-0.53710296957742));
#30168=CARTESIAN_POINT('Ctrl Pts',(-0.0758231831874148,7.55519090022252,
-0.583595570273457));
#30169=CARTESIAN_POINT('Ctrl Pts',(-0.0825535996829062,7.54772002274568,
-0.628167677544045));
#30170=CARTESIAN_POINT('Ctrl Pts',(-0.0847656202997536,7.54526464201022,
-0.642816759110531));
#30171=CARTESIAN_POINT('Ctrl Pts',(-0.0869595840064315,7.54275576400144,
-0.657258458698621));
#30172=CARTESIAN_POINT('Ctrl Pts',(-0.089137682999504,7.54019870001955,
-0.671501068034935));
#30173=CARTESIAN_POINT('Ctrl Pts',(-0.0960094214851858,7.53213135550004,
-0.716435429156335));
#30174=CARTESIAN_POINT('Ctrl Pts',(-0.102723249744971,7.52358858876181,
-0.759387035915678));
#30175=CARTESIAN_POINT('Ctrl Pts',(-0.109312534293958,7.51469777608467,
-0.800637516202912));
#30176=CARTESIAN_POINT('Ctrl Pts',(-0.111166622784501,7.51219608514483,
-0.812244548827073));
#30177=CARTESIAN_POINT('Ctrl Pts',(-0.113010850610315,7.50966651757017,
-0.823716907616661));
#30178=CARTESIAN_POINT('Ctrl Pts',(-0.114845961111285,7.50711118316948,
-0.835060881385187));
#30179=CARTESIAN_POINT('Ctrl Pts',(-0.122674528194227,7.49621014654818,
-0.883454184996663));
#30180=CARTESIAN_POINT('Ctrl Pts',(-0.130337171913731,7.48484430754926,
-0.92950977420178));
#30181=CARTESIAN_POINT('Ctrl Pts',(-0.13787348511751,7.47320056436962,-0.973446256305266));
#30182=CARTESIAN_POINT('Ctrl Pts',(-0.138382141405972,7.47241468100338,
-0.976411707356797));
#30183=CARTESIAN_POINT('Ctrl Pts',(-0.138890222202518,7.47162751222442,
-0.979367506733599));
#30184=CARTESIAN_POINT('Ctrl Pts',(-0.139397739680585,7.4708391071944,-0.982313722337323));
#30185=CARTESIAN_POINT('Ctrl Pts',(-0.147424697609637,7.45836959770851,
-1.02891142531904));
#30186=CARTESIAN_POINT('Ctrl Pts',(-0.155310741596374,7.44559460087546,
-1.07311084051926));
#30187=CARTESIAN_POINT('Ctrl Pts',(-0.16306962603091,7.43271369199364,-1.11507454100697));
#30188=CARTESIAN_POINT('Ctrl Pts',(-0.170828510465437,7.41983278311185,
-1.15703824149462));
#30189=CARTESIAN_POINT('Ctrl Pts',(-0.178460235347763,7.40684609699437,
-1.19676630296227));
#30190=CARTESIAN_POINT('Ctrl Pts',(-0.18598165758979,7.39389918170677,-1.23445885785126));
#30191=CARTESIAN_POINT('Ctrl Pts',(-0.193503079831827,7.38095226641914,
-1.27215141274029));
#30192=CARTESIAN_POINT('Ctrl Pts',(-0.200914199433564,7.36804654154129,
-1.30780888798301));
#30193=CARTESIAN_POINT('Ctrl Pts',(-0.208273146572715,7.35521654045108,
-1.34180302224396));
#30194=CARTESIAN_POINT('Ctrl Pts',(-0.215632093711867,7.34238653936088,
-1.37579715650491));
#30195=CARTESIAN_POINT('Ctrl Pts',(-0.222938868388433,7.32962691491351,
-1.40812595456969));
#30196=CARTESIAN_POINT('Ctrl Pts',(-0.230130727085702,7.31715746497242,
-1.43861161075141));
#30197=CARTESIAN_POINT('Ctrl Pts',(-0.23732258578297,7.30468801503134,-1.46909726693312));
#30198=CARTESIAN_POINT('Ctrl Pts',(-0.244399528500939,7.29251460227622,
-1.49774227401089));
#30199=CARTESIAN_POINT('Ctrl Pts',(-0.251454846117659,7.28054053449819,
-1.52506969929741));
#30200=CARTESIAN_POINT('Ctrl Pts',(-0.25690111865087,7.27129728848248,-1.546164795766));
#30201=CARTESIAN_POINT('Ctrl Pts',(-0.262334505017244,7.2621740640714,-1.56647526973809));
#30202=CARTESIAN_POINT('Ctrl Pts',(-0.267949664838005,7.25289346545703,
-1.58667158423037));
#30203=CARTESIAN_POINT('Ctrl Pts',(-0.269608605929838,7.25015160825446,
-1.59263837717737));
#30204=CARTESIAN_POINT('Ctrl Pts',(-0.271283413047111,7.24739569673469,
-1.59859506772109));
#30205=CARTESIAN_POINT('Ctrl Pts',(-0.272979105943457,7.24461779005209,
-1.60455859365018));
#30206=CARTESIAN_POINT('Ctrl Pts',(-0.278853400616557,7.23499444229667,
-1.62521770514));
#30207=CARTESIAN_POINT('Ctrl Pts',(-0.28497834530457,7.22511073105216,-1.64596018555078));
#30208=CARTESIAN_POINT('Ctrl Pts',(-0.291647922678002,7.21464910375299,
-1.6673846281644));
#30209=CARTESIAN_POINT('Ctrl Pts',(-0.29342020528643,7.21186917346954,-1.67307766760504));
#30210=CARTESIAN_POINT('Ctrl Pts',(-0.295230944684135,7.20904818512805,
-1.67881873367243));
#30211=CARTESIAN_POINT('Ctrl Pts',(-0.297085656889598,7.20617962066412,
-1.68461876748789));
#30212=CARTESIAN_POINT('Ctrl Pts',(-0.3059201512703,7.19251587457857,-1.71224589260175));
#30213=CARTESIAN_POINT('Ctrl Pts',(-0.3157523331599,7.177768171723,-1.7412089147651));
#30214=CARTESIAN_POINT('Ctrl Pts',(-0.3268604435631,7.16212807842995,-1.77090225146193));
#30215=CARTESIAN_POINT('',(-0.499999999994609,6.62677536195992,2.53955528646714));
#30216=CARTESIAN_POINT('Origin',(-0.5,3.8,0.));
#30217=CARTESIAN_POINT('',(-0.326861933644355,7.16212485193451,1.77090837708044));
#30218=CARTESIAN_POINT('Ctrl Pts',(-0.499999999983828,6.62677536195925,
2.53955528646654));
#30219=CARTESIAN_POINT('Ctrl Pts',(-0.499999467882044,6.65885242763283,
2.50385035048297));
#30220=CARTESIAN_POINT('Ctrl Pts',(-0.498254574299847,6.68984855845096,
2.46798114714233));
#30221=CARTESIAN_POINT('Ctrl Pts',(-0.495166769760691,6.71956677258583,
2.43230957330944));
#30222=CARTESIAN_POINT('Ctrl Pts',(-0.493039810618576,6.74003744242258,
2.40773807627478));
#30223=CARTESIAN_POINT('Ctrl Pts',(-0.490275665939506,6.75990271637183,
2.38326105061858));
#30224=CARTESIAN_POINT('Ctrl Pts',(-0.487005543648317,6.7791104007444,2.35900428574781));
#30225=CARTESIAN_POINT('Ctrl Pts',(-0.483408131607721,6.80024048362235,
2.33231978582952));
#30226=CARTESIAN_POINT('Ctrl Pts',(-0.479198392184817,6.82057833554045,
2.30590616238507));
#30227=CARTESIAN_POINT('Ctrl Pts',(-0.474372740318849,6.84044316012923,
2.27940900016284));
#30228=CARTESIAN_POINT('Ctrl Pts',(-0.469513754566043,6.86044520386132,
2.25272880496774));
#30229=CARTESIAN_POINT('Ctrl Pts',(-0.46403031797336,6.87996776013273,2.2259636983694));
#30230=CARTESIAN_POINT('Ctrl Pts',(-0.457918770672701,6.89929534060611,
2.1987197164935));
#30231=CARTESIAN_POINT('Ctrl Pts',(-0.456572555291486,6.90355270536742,
2.19271857379713));
#30232=CARTESIAN_POINT('Ctrl Pts',(-0.455195863561208,6.90780044722032,
2.1866940789898));
#30233=CARTESIAN_POINT('Ctrl Pts',(-0.453788656365767,6.91204132778548,
2.18064182619594));
#30234=CARTESIAN_POINT('Ctrl Pts',(-0.44566350020286,6.93652799682176,2.14569636880571));
#30235=CARTESIAN_POINT('Ctrl Pts',(-0.436521001197984,6.96078712409439,
2.10983035256709));
#30236=CARTESIAN_POINT('Ctrl Pts',(-0.426223710362374,6.98493152223582,
2.07273037288226));
#30237=CARTESIAN_POINT('Ctrl Pts',(-0.418600565928086,7.00280576093116,
2.04526504164499));
#30238=CARTESIAN_POINT('Ctrl Pts',(-0.41034453468845,7.02061630865858,2.01712292969638));
#30239=CARTESIAN_POINT('Ctrl Pts',(-0.401399849929217,7.03839226582423,
1.98816888936776));
#30240=CARTESIAN_POINT('Ctrl Pts',(-0.3857029698909,7.06958700042988,1.93735792063084));
#30241=CARTESIAN_POINT('Ctrl Pts',(-0.367885301294979,7.10066919086031,
1.8840414927651));
#30242=CARTESIAN_POINT('Ctrl Pts',(-0.347930442107598,7.13121203007297,
1.82839448990012));
#30243=CARTESIAN_POINT('Ctrl Pts',(-0.341154327931767,7.14158352725146,
1.80949831822508));
#30244=CARTESIAN_POINT('Ctrl Pts',(-0.334131775941308,7.15189303368305,
1.79033379515737));
#30245=CARTESIAN_POINT('Ctrl Pts',(-0.3268621439014,7.16212453739185,1.77090897424674));
#30246=CARTESIAN_POINT('',(-3.64874277834443E-8,7.59962390164863,0.0534561363041487));
#30247=CARTESIAN_POINT('Ctrl Pts',(-0.326861921820406,7.16212485010976,
1.77090838054216));
#30248=CARTESIAN_POINT('Ctrl Pts',(-0.31954228299043,7.17243182436564,1.75134026812263));
#30249=CARTESIAN_POINT('Ctrl Pts',(-0.312411768814016,7.18289258093581,
1.73105973218841));
#30250=CARTESIAN_POINT('Ctrl Pts',(-0.305543769648105,7.19325550339669,
1.71050199902487));
#30251=CARTESIAN_POINT('Ctrl Pts',(-0.299865103021706,7.20182387687912,
1.69350425187754));
#30252=CARTESIAN_POINT('Ctrl Pts',(-0.294365904146499,7.21033086126211,
1.67631988987955));
#30253=CARTESIAN_POINT('Ctrl Pts',(-0.288814745499469,7.21911220555782,
1.65821341382993));
#30254=CARTESIAN_POINT('Ctrl Pts',(-0.287652050165329,7.22095146627604,
1.65442099560534));
#30255=CARTESIAN_POINT('Ctrl Pts',(-0.286487075372026,7.22280259969396,
1.65058804734064));
#30256=CARTESIAN_POINT('Ctrl Pts',(-0.28531769463674,7.22466842147799,1.64670768593927));
#30257=CARTESIAN_POINT('Ctrl Pts',(-0.278565236555438,7.23544240039147,
1.6243009736407));
#30258=CARTESIAN_POINT('Ctrl Pts',(-0.271665868697669,7.24670407697142,
1.60031225523227));
#30259=CARTESIAN_POINT('Ctrl Pts',(-0.264753638980818,7.25819325055929,
1.57508712196697));
#30260=CARTESIAN_POINT('Ctrl Pts',(-0.257841409263967,7.26968242414716,
1.54986198870167));
#30261=CARTESIAN_POINT('Ctrl Pts',(-0.250916317688033,7.28140332642829,
1.52340229432317));
#30262=CARTESIAN_POINT('Ctrl Pts',(-0.243933082800448,7.29336386697047,
1.49546276882614));
#30263=CARTESIAN_POINT('Ctrl Pts',(-0.236949847912863,7.30532440751264,
1.46752324332912));
#30264=CARTESIAN_POINT('Ctrl Pts',(-0.229908469713627,7.3175229845504,1.43810324340012));
#30265=CARTESIAN_POINT('Ctrl Pts',(-0.222822150024707,7.32985421809982,
1.40717063605055));
#30266=CARTESIAN_POINT('Ctrl Pts',(-0.215735830335797,7.34218545164923,
1.37623802870101));
#30267=CARTESIAN_POINT('Ctrl Pts',(-0.208604569157203,7.35465118941044,
1.34379351988619));
#30268=CARTESIAN_POINT('Ctrl Pts',(-0.20139409589261,7.3672012700211,1.30960875804947));
#30269=CARTESIAN_POINT('Ctrl Pts',(-0.194183622628007,7.37975135063177,
1.27542399621269));
#30270=CARTESIAN_POINT('Ctrl Pts',(-0.186893937277403,7.39238525751293,
1.23949884094967));
#30271=CARTESIAN_POINT('Ctrl Pts',(-0.179513347151867,7.40499181357504,
1.20167966782207));
#30272=CARTESIAN_POINT('Ctrl Pts',(-0.17213275702633,7.41759836963715,1.16386049469447));
#30273=CARTESIAN_POINT('Ctrl Pts',(-0.16466126212586,7.43017569136328,1.1241466306025));
#30274=CARTESIAN_POINT('Ctrl Pts',(-0.157115542594223,7.4425320365945,1.08257118120829));
#30275=CARTESIAN_POINT('Ctrl Pts',(-0.149569823062597,7.45488838182571,
1.04099573181413));
#30276=CARTESIAN_POINT('Ctrl Pts',(-0.141949878899804,7.46702770849417,
0.997559839050793));
#30277=CARTESIAN_POINT('Ctrl Pts',(-0.134207247927611,7.47882559930028,
0.951967546680531));
#30278=CARTESIAN_POINT('Ctrl Pts',(-0.127569153529608,7.4889404443897,0.912879290807032));
#30279=CARTESIAN_POINT('Ctrl Pts',(-0.120840879678029,7.49880487434111,
0.872206528993969));
#30280=CARTESIAN_POINT('Ctrl Pts',(-0.113972151342168,7.50832593577324,
0.829649777961458));
#30281=CARTESIAN_POINT('Ctrl Pts',(-0.112829238751547,7.50991017967616,
0.822568605990071));
#30282=CARTESIAN_POINT('Ctrl Pts',(-0.111682437420423,7.51148479986071,
0.815435269715585));
#30283=CARTESIAN_POINT('Ctrl Pts',(-0.110531515736092,7.51304922446613,
0.808248387991861));
#30284=CARTESIAN_POINT('Ctrl Pts',(-0.104093298236056,7.52180056350963,
0.768045211429718));
#30285=CARTESIAN_POINT('Ctrl Pts',(-0.0975261447369932,7.53023680004186,
0.726167000036956));
#30286=CARTESIAN_POINT('Ctrl Pts',(-0.0907979124505207,7.53823709415698,
0.682336740817026));
#30287=CARTESIAN_POINT('Ctrl Pts',(-0.0890949413789858,7.54026203456654,
0.671242940791797));
#30288=CARTESIAN_POINT('Ctrl Pts',(-0.0873816509907904,7.54225878911023,
0.660024094937112));
#30289=CARTESIAN_POINT('Ctrl Pts',(-0.0856575200883063,7.54422485749934,
0.648675740631694));
#30290=CARTESIAN_POINT('Ctrl Pts',(-0.0780501822834028,7.5528996897652,
0.598603692966023));
#30291=CARTESIAN_POINT('Ctrl Pts',(-0.0702317996000271,7.5609805902286,
0.546009698563104));
#30292=CARTESIAN_POINT('Ctrl Pts',(-0.0621404289523591,7.56817341120464,
0.490784212348375));
#30293=CARTESIAN_POINT('Ctrl Pts',(-0.0611527179055199,7.56905143657825,
0.48404285477417));
#30294=CARTESIAN_POINT('Ctrl Pts',(-0.0601609390630012,7.56991616927957,
0.477262309172276));
#30295=CARTESIAN_POINT('Ctrl Pts',(-0.0591649797527306,7.57076702420316,
0.47044239730501));
#30296=CARTESIAN_POINT('Ctrl Pts',(-0.0514071364497827,7.57739460336494,
0.417319938324441));
#30297=CARTESIAN_POINT('Ctrl Pts',(-0.0433956496729695,7.58318385945646,
0.361807975159004));
#30298=CARTESIAN_POINT('Ctrl Pts',(-0.0351244935789875,7.58783553344008,
0.30381239541647));
#30299=CARTESIAN_POINT('Ctrl Pts',(-0.0336349978223634,7.58867322149494,
0.293368369339836));
#30300=CARTESIAN_POINT('Ctrl Pts',(-0.0321370810061093,7.58947389577398,
0.282843860180307));
#30301=CARTESIAN_POINT('Ctrl Pts',(-0.0306307079387886,7.59023564599293,
0.272238402589614));
#30302=CARTESIAN_POINT('Ctrl Pts',(-0.0215805482817282,7.59481217570519,
0.20852172674472));
#30303=CARTESIAN_POINT('Ctrl Pts',(-0.0122251599957601,7.59798568401548,
0.141880460804193));
#30304=CARTESIAN_POINT('Ctrl Pts',(-0.0026203985044172,7.59930968800899,
0.0724285482460437));
#30305=CARTESIAN_POINT('Ctrl Pts',(-0.00174900018331175,7.59942980914455,
0.0661274776723202));
#30306=CARTESIAN_POINT('Ctrl Pts',(-0.000875549235118814,7.59953468986068,
0.0598033036408318));
#30307=CARTESIAN_POINT('Ctrl Pts',(-8.73713329792359E-8,7.59962398693785,
0.0534561304856728));
#30308=CARTESIAN_POINT('Ctrl Pts',(-6.386159488164E-8,7.59962398933584,
0.053455960038065));
#30309=CARTESIAN_POINT('Ctrl Pts',(-0.001454973167811,7.59968667669039,
0.0490001729562442));
#30310=CARTESIAN_POINT('Ctrl Pts',(-0.0027084035629715,7.59974068390958,
0.0446031751838687));
#30311=CARTESIAN_POINT('Ctrl Pts',(-0.00377278909219608,7.59978652991921,
0.0402781211647162));
#30312=CARTESIAN_POINT('Ctrl Pts',(-0.00483717462142067,7.59983237592883,
0.0359530671455637));
#30313=CARTESIAN_POINT('Ctrl Pts',(-0.00571251528470933,7.59987010056958,
0.031699957127514));
#30314=CARTESIAN_POINT('Ctrl Pts',(-0.00641840715996133,7.59990051616159,
0.0274966775244882));
#30315=CARTESIAN_POINT('Ctrl Pts',(-0.00712429903521333,7.5999309317536,
0.0232933979214624));
#30316=CARTESIAN_POINT('Ctrl Pts',(-0.00766074212242867,7.59995405590909,
0.0191399489324386));
#30317=CARTESIAN_POINT('Ctrl Pts',(-0.008040469817144,7.59997040663964,
0.0149969551230673));
#30318=CARTESIAN_POINT('Ctrl Pts',(-0.00842019751185934,7.5999867573702,
0.0108539613136959));
#30319=CARTESIAN_POINT('Ctrl Pts',(-0.00864320981407467,7.59999637482113,
0.00672142282462303));
#30320=CARTESIAN_POINT('Ctrl Pts',(-0.008707854494372,7.59999916238416,
0.00252306949195798));
#30321=CARTESIAN_POINT('Ctrl Pts',(-0.00877249917466933,7.6000019499472,
-0.00167528384070706));
#30322=CARTESIAN_POINT('Ctrl Pts',(-0.00867877623304867,7.59999789737958,
-0.00593945192864444));
#30323=CARTESIAN_POINT('Ctrl Pts',(-0.0084012235511355,7.5999859531005,
-0.0103322910770659));
#30324=CARTESIAN_POINT('Ctrl Pts',(-0.00812367086922233,7.59997400882142,
-0.0147251302254874));
#30325=CARTESIAN_POINT('Ctrl Pts',(-0.00766228844701667,7.59995411157182,
-0.0192466402929024));
#30326=CARTESIAN_POINT('Ctrl Pts',(-0.00698246627103333,7.59992482072332,
-0.0239030719956763));
#30327=CARTESIAN_POINT('Ctrl Pts',(-0.00630264409505,7.59989552987482,-0.0285595036984501));
#30328=CARTESIAN_POINT('Ctrl Pts',(-0.005404382165289,7.59985684155893,
-0.0333508570331727));
#30329=CARTESIAN_POINT('Ctrl Pts',(-0.0042522637803775,7.59980718776503,
-0.038279704925825));
#30330=CARTESIAN_POINT('Ctrl Pts',(-0.0031002334799121,7.59975753776738,
-0.0432081759866854));
#30331=CARTESIAN_POINT('Ctrl Pts',(-0.00169438553966578,7.59969689622004,
-0.0482741203060225));
#30332=CARTESIAN_POINT('Ctrl Pts',(-1.29815779802503E-6,7.59962393902838,
-0.0534595357485616));
#30333=CARTESIAN_POINT('Origin',(0.,3.8,0.));
#30334=CARTESIAN_POINT('',(-0.5,2.02155349221333,-3.35814353757271));
#30335=CARTESIAN_POINT('Origin',(-0.5,3.8,0.));
#30336=CARTESIAN_POINT('',(-0.2886751345948,3.80000000040883,-3.8));
#30337=CARTESIAN_POINT('Ctrl Pts',(-0.4330127018922,5.076816196554,-3.57906976744201));
#30338=CARTESIAN_POINT('Ctrl Pts',(-0.421461672428874,5.02725333529887,
-3.59675108356883));
#30339=CARTESIAN_POINT('Ctrl Pts',(-0.410577745135395,4.97711104164099,
-3.61347395830865));
#30340=CARTESIAN_POINT('Ctrl Pts',(-0.400383395751461,4.92671602852758,
-3.62911986452074));
#30341=CARTESIAN_POINT('Ctrl Pts',(-0.390148390356685,4.87612003542787,
-3.64482816805792));
#30342=CARTESIAN_POINT('Ctrl Pts',(-0.38060847404043,4.82526964336495,-3.65945078408262));
#30343=CARTESIAN_POINT('Ctrl Pts',(-0.37178639252225,4.77451034843562,-3.67291840105275));
#30344=CARTESIAN_POINT('Ctrl Pts',(-0.366141025004971,4.74202879924528,
-3.68153650860726));
#30345=CARTESIAN_POINT('Ctrl Pts',(-0.360789602986865,4.70958483923676,
-3.68968269340426));
#30346=CARTESIAN_POINT('Ctrl Pts',(-0.355738086699606,4.67727116194173,
-3.69734976820227));
#30347=CARTESIAN_POINT('Ctrl Pts',(-0.349682038096245,4.63853166490287,
-3.70654149895834));
#30348=CARTESIAN_POINT('Ctrl Pts',(-0.344057031854475,4.59998676204821,
-3.71504840903257));
#30349=CARTESIAN_POINT('Ctrl Pts',(-0.338840070970698,4.56124717707513,
-3.7229696124727));
#30350=CARTESIAN_POINT('Ctrl Pts',(-0.333642550907729,4.52265195379967,
-3.73086129782748));
#30351=CARTESIAN_POINT('Ctrl Pts',(-0.328850040735808,4.48386323128829,
-3.73817168621647));
#30352=CARTESIAN_POINT('Ctrl Pts',(-0.324439799587048,4.44448617446809,
-3.7449482734638));
#30353=CARTESIAN_POINT('Ctrl Pts',(-0.320114530549047,4.40586779535293,
-3.75159429621302));
#30354=CARTESIAN_POINT('Ctrl Pts',(-0.316156942085466,4.36668328229687,
-3.7577269598045));
#30355=CARTESIAN_POINT('Ctrl Pts',(-0.312545582610481,4.3265544635123,-3.76334165296685));
#30356=CARTESIAN_POINT('Ctrl Pts',(-0.310835779677329,4.30755542103619,
-3.76599993689129));
#30357=CARTESIAN_POINT('Ctrl Pts',(-0.309203586104177,4.28834464558913,
-3.76854138443604));
#30358=CARTESIAN_POINT('Ctrl Pts',(-0.307646725297922,4.26888179333454,
-3.77096139782409));
#30359=CARTESIAN_POINT('Ctrl Pts',(-0.303204116915783,4.21334321838992,
-3.77786707090637));
#30360=CARTESIAN_POINT('Ctrl Pts',(-0.299374932036076,4.15576288358911,
-3.78377686396753));
#30361=CARTESIAN_POINT('Ctrl Pts',(-0.296343544491563,4.09649174472707,
-3.78841558508418));
#30362=CARTESIAN_POINT('Ctrl Pts',(-0.29341632601102,4.03925736921679,-3.79289490354127));
#30363=CARTESIAN_POINT('Ctrl Pts',(-0.291233016738444,3.98044673527077,
-3.79618867850224));
#30364=CARTESIAN_POINT('Ctrl Pts',(-0.289959628991768,3.92039772486898,
-3.79809220370522));
#30365=CARTESIAN_POINT('Ctrl Pts',(-0.289119295393155,3.88077020282327,
-3.7993483773947));
#30366=CARTESIAN_POINT('Ctrl Pts',(-0.288675227111371,3.84060382170757,
-3.79999999999563));
#30367=CARTESIAN_POINT('Ctrl Pts',(-0.288675134594801,3.80000000040882,
-3.8));
#30368=CARTESIAN_POINT('',(-0.433012748163602,2.52318359238809,-3.57906969214748));
#30369=CARTESIAN_POINT('Ctrl Pts',(-0.2886751345948,3.799999999988,-3.8));
#30370=CARTESIAN_POINT('Ctrl Pts',(-0.288675077415421,3.74533021445964,
-3.79999999999983));
#30371=CARTESIAN_POINT('Ctrl Pts',(-0.289487908451124,3.69041088673595,
-3.79881587771527));
#30372=CARTESIAN_POINT('Ctrl Pts',(-0.291063540487692,3.63558198909325,
-3.79644132282977));
#30373=CARTESIAN_POINT('Ctrl Pts',(-0.292642987709118,3.58062033051703,
-3.79406101827327));
#30374=CARTESIAN_POINT('Ctrl Pts',(-0.294988934447464,3.52574990970548,
-3.79048451816112));
#30375=CARTESIAN_POINT('Ctrl Pts',(-0.298050928768093,3.47131045792295,
-3.78575794061495));
#30376=CARTESIAN_POINT('Ctrl Pts',(-0.299717636057897,3.4416779303485,-3.78318516600236));
#30377=CARTESIAN_POINT('Ctrl Pts',(-0.301596497624397,3.41217301177703,
-3.78027255366643));
#30378=CARTESIAN_POINT('Ctrl Pts',(-0.303679376872831,3.38284956903489,
-3.77703395774325));
#30379=CARTESIAN_POINT('Ctrl Pts',(-0.306623102617713,3.34140685295161,
-3.77245686178173));
#30380=CARTESIAN_POINT('Ctrl Pts',(-0.309974334650717,3.30033191238049,
-3.76723435458545));
#30381=CARTESIAN_POINT('Ctrl Pts',(-0.313797594204672,3.25924674056197,
-3.76132767947797));
#30382=CARTESIAN_POINT('Ctrl Pts',(-0.317605535936777,3.21832617575843,
-3.75544466935995));
#30383=CARTESIAN_POINT('Ctrl Pts',(-0.321881730426927,3.17739517904764,
-3.74888292969922));
#30384=CARTESIAN_POINT('Ctrl Pts',(-0.326689926501334,3.13608827366232,
-3.74155331642238));
#30385=CARTESIAN_POINT('Ctrl Pts',(-0.33141297166874,3.09551289428063,-3.73435350717368));
#30386=CARTESIAN_POINT('Ctrl Pts',(-0.336649342271546,3.05457452467595,
-3.72641276750167));
#30387=CARTESIAN_POINT('Ctrl Pts',(-0.342459459876233,3.0129385834656,-3.71759792427891));
#30388=CARTESIAN_POINT('Ctrl Pts',(-0.344418554584142,2.99889949551009,
-3.71462567588676));
#30389=CARTESIAN_POINT('Ctrl Pts',(-0.346442881404941,2.98478121679129,
-3.71155363126647));
#30390=CARTESIAN_POINT('Ctrl Pts',(-0.348534756685023,2.9705713231386,-3.70837539496744));
#30391=CARTESIAN_POINT('Ctrl Pts',(-0.356659453339846,2.91538109429238,
-3.69603134842088));
#30392=CARTESIAN_POINT('Ctrl Pts',(-0.365803112449362,2.85881925761048,
-3.68208281858365));
#30393=CARTESIAN_POINT('Ctrl Pts',(-0.37604091649859,2.80129090113052,-3.66641243395166));
#30394=CARTESIAN_POINT('Ctrl Pts',(-0.385983162284082,2.74542334818568,
-3.65119444239651));
#30395=CARTESIAN_POINT('Ctrl Pts',(-0.396957290506915,2.68864469579488,
-3.6343524254303));
#30396=CARTESIAN_POINT('Ctrl Pts',(-0.409032158424929,2.63132978639543,
-3.61582769664616));
#30397=CARTESIAN_POINT('Ctrl Pts',(-0.416588932442298,2.59546058922504,
-3.60423442787457));
#30398=CARTESIAN_POINT('Ctrl Pts',(-0.424576821049575,2.55938141989069,
-3.59198309575253));
#30399=CARTESIAN_POINT('Ctrl Pts',(-0.4330127018923,2.52318380344511,-3.57906976744169));
#30400=CARTESIAN_POINT('Ctrl Pts',(-0.433012750939953,2.52318359296197,
-3.57906969235237));
#30401=CARTESIAN_POINT('Ctrl Pts',(-0.448008301212658,2.45883169965399,
-3.55611221221238));
#30402=CARTESIAN_POINT('Ctrl Pts',(-0.47294675063507,2.33599978785211,-3.50837670153741));
#30403=CARTESIAN_POINT('Ctrl Pts',(-0.4951282325919,2.169475318356,-3.433897201164));
#30404=CARTESIAN_POINT('Ctrl Pts',(-0.5000030708506,2.069070757037,-3.383302730847));
#30405=CARTESIAN_POINT('Ctrl Pts',(-0.5000027938226,2.021563351426,-3.358143198296));
#30406=CARTESIAN_POINT('Origin',(0.,3.8,0.));
#30407=CARTESIAN_POINT('',(-0.2886751345948,3.79999999959147,3.8));
#30408=CARTESIAN_POINT('',(-0.433012748163509,5.07681640761144,3.57906969214753));
#30409=CARTESIAN_POINT('Ctrl Pts',(-0.2886751345948,3.800000000012,3.8));
#30410=CARTESIAN_POINT('Ctrl Pts',(-0.288675077512002,3.854680470407,3.79999999999983));
#30411=CARTESIAN_POINT('Ctrl Pts',(-0.289488192254766,3.90961078877838,
3.79881541653737));
#30412=CARTESIAN_POINT('Ctrl Pts',(-0.29106443631587,3.96445101878628,3.79643989316572));
#30413=CARTESIAN_POINT('Ctrl Pts',(-0.292644478808979,4.01942340274798,
3.79405864525926));
#30414=CARTESIAN_POINT('Ctrl Pts',(-0.294991333029181,4.07430489435071,
3.79048071962058));
#30415=CARTESIAN_POINT('Ctrl Pts',(-0.298054593819528,4.12875580671285,
3.78575218675927));
#30416=CARTESIAN_POINT('Ctrl Pts',(-0.299720336973532,4.15836518074405,
3.78318090021813));
#30417=CARTESIAN_POINT('Ctrl Pts',(-0.301597919992156,4.18784731408018,
3.78027029368594));
#30418=CARTESIAN_POINT('Ctrl Pts',(-0.303679237984622,4.21714850636058,
3.77703417030362));
#30419=CARTESIAN_POINT('Ctrl Pts',(-0.306623704527528,4.25860126881648,
3.77245598616143));
#30420=CARTESIAN_POINT('Ctrl Pts',(-0.309975928571019,4.29968660146913,
3.76723201769777));
#30421=CARTESIAN_POINT('Ctrl Pts',(-0.313800430565152,4.34078239401191,
3.76132349078443));
#30422=CARTESIAN_POINT('Ctrl Pts',(-0.31760959484575,4.38171337673252,3.75543865932041));
#30423=CARTESIAN_POINT('Ctrl Pts',(-0.321887256642832,4.4226550181757,3.74887471626853));
#30424=CARTESIAN_POINT('Ctrl Pts',(-0.326697163260439,4.46397267254489,
3.74154250144424));
#30425=CARTESIAN_POINT('Ctrl Pts',(-0.331421911964052,4.50455881057979,
3.73434010122323));
#30426=CARTESIAN_POINT('Ctrl Pts',(-0.336660225862619,4.54550804309632,
3.72639637912335));
#30427=CARTESIAN_POINT('Ctrl Pts',(-0.342472525973247,4.58715483660548,
3.71757814486913));
#30428=CARTESIAN_POINT('Ctrl Pts',(-0.344428109536364,4.60116715243447,
3.7146111965638));
#30429=CARTESIAN_POINT('Ctrl Pts',(-0.346448669875045,4.61525831485455,
3.71154483758887));
#30430=CARTESIAN_POINT('Ctrl Pts',(-0.348536508288431,4.62944066318899,
3.70837271404165));
#30431=CARTESIAN_POINT('Ctrl Pts',(-0.356662858901035,4.68464164729618,
3.69602607458624));
#30432=CARTESIAN_POINT('Ctrl Pts',(-0.365808436465691,4.74121366106227,
3.68207456931469));
#30433=CARTESIAN_POINT('Ctrl Pts',(-0.376048419508924,4.79875168152469,
3.66640083442217));
#30434=CARTESIAN_POINT('Ctrl Pts',(-0.385992977863913,4.85462972348075,
3.65117928858355));
#30435=CARTESIAN_POINT('Ctrl Pts',(-0.396969705155249,4.91141841694761,
3.63433329970587));
#30436=CARTESIAN_POINT('Ctrl Pts',(-0.409047459096639,4.96874295603494,
3.61580418478638));
#30437=CARTESIAN_POINT('Ctrl Pts',(-0.416599751629854,5.00458833677544,
3.60421781724382));
#30438=CARTESIAN_POINT('Ctrl Pts',(-0.424582554004133,5.04064317972623,
3.59197431995565));
#30439=CARTESIAN_POINT('Ctrl Pts',(-0.4330127018923,5.07681619655489,3.57906976744169));
#30440=CARTESIAN_POINT('',(-0.500001202747678,5.57843980229415,3.35814469502115));
#30441=CARTESIAN_POINT('Ctrl Pts',(-0.433012750939854,5.07681640703761,
3.57906969235253));
#30442=CARTESIAN_POINT('Ctrl Pts',(-0.448008301217003,5.14116830036308,
3.55611221220637));
#30443=CARTESIAN_POINT('Ctrl Pts',(-0.472946750665154,5.26399868565327,
3.50837750997614));
#30444=CARTESIAN_POINT('Ctrl Pts',(-0.495128010756759,5.4305283596975,3.43389511617736));
#30445=CARTESIAN_POINT('Ctrl Pts',(-0.500002924832392,5.53091478323016,
3.38331031137448));
#30446=CARTESIAN_POINT('Ctrl Pts',(-0.500002793997349,5.57842093152281,
3.35815152191705));
#30447=CARTESIAN_POINT('',(-0.5,3.76245328712248,3.7998145013082));
#30448=CARTESIAN_POINT('Origin',(-0.5,3.8,0.));
#30449=CARTESIAN_POINT('',(-0.500000724156204,2.02156681047555,3.35815048826256));
#30450=CARTESIAN_POINT('Origin',(-0.5,3.8,0.));
#30451=CARTESIAN_POINT('',(-0.4330127018922,2.523183803446,3.579069767442));
#30452=CARTESIAN_POINT('Ctrl Pts',(-0.5000021724646,2.021587730931,3.358161259977));
#30453=CARTESIAN_POINT('Ctrl Pts',(-0.5000045975033,2.07348246476,3.385642437576));
#30454=CARTESIAN_POINT('Ctrl Pts',(-0.4942244624564,2.180032313752,3.438990064545));
#30455=CARTESIAN_POINT('Ctrl Pts',(-0.4708077491425,2.347687391963,3.513147271656));
#30456=CARTESIAN_POINT('Ctrl Pts',(-0.4468343744848,2.463881670505,3.557914059235));
#30457=CARTESIAN_POINT('Ctrl Pts',(-0.4330127018922,2.523183803446,3.579069767442));
#30458=CARTESIAN_POINT('Ctrl Pts',(-0.4330127018922,2.523183803446,3.57906976744201));
#30459=CARTESIAN_POINT('Ctrl Pts',(-0.421461955081707,2.57274545228049,
3.59675065104351));
#30460=CARTESIAN_POINT('Ctrl Pts',(-0.410578361600438,2.62288617598632,
3.61347302244933));
#30461=CARTESIAN_POINT('Ctrl Pts',(-0.400384366707824,2.67327924047737,
3.62911839570725));
#30462=CARTESIAN_POINT('Ctrl Pts',(-0.390149610775323,2.72387380337345,
3.64482632752932));
#30463=CARTESIAN_POINT('Ctrl Pts',(-0.380609979224414,2.77472238881455,
3.65944851944638));
#30464=CARTESIAN_POINT('Ctrl Pts',(-0.371788187636978,2.82547947224395,
3.6729157002281));
#30465=CARTESIAN_POINT('Ctrl Pts',(-0.366141409425059,2.85796879031149,
3.68153596542712));
#30466=CARTESIAN_POINT('Ctrl Pts',(-0.360788745083571,2.89042033217581,
3.68968403564874));
#30467=CARTESIAN_POINT('Ctrl Pts',(-0.355736151997639,2.92274131878139,
3.69735272948451));
#30468=CARTESIAN_POINT('Ctrl Pts',(-0.349680482227613,2.96147889732692,
3.70654386691575));
#30469=CARTESIAN_POINT('Ctrl Pts',(-0.344055854981136,3.00002159271372,
3.71505018110053));
#30470=CARTESIAN_POINT('Ctrl Pts',(-0.338839256994681,3.03875870384398,
3.72297081495769));
#30471=CARTESIAN_POINT('Ctrl Pts',(-0.333642070583658,3.07735166962192,
3.7308619752035));
#30472=CARTESIAN_POINT('Ctrl Pts',(-0.328849882432668,3.11613787231206,
3.73817185829506));
#30473=CARTESIAN_POINT('Ctrl Pts',(-0.324439935228584,3.15551217709503,
3.74494798977599));
#30474=CARTESIAN_POINT('Ctrl Pts',(-0.320114937030083,3.19412801292544,
3.75159359234028));
#30475=CARTESIAN_POINT('Ctrl Pts',(-0.316157595366561,3.23330976389502,
3.75772587921199));
#30476=CARTESIAN_POINT('Ctrl Pts',(-0.312546442879592,3.27343563631605,
3.76334026775392));
#30477=CARTESIAN_POINT('Ctrl Pts',(-0.310836075108498,3.29244064904359,
3.76599943799144));
#30478=CARTESIAN_POINT('Ctrl Pts',(-0.309203367954887,3.31165751762995,
3.76854169759761));
#30479=CARTESIAN_POINT('Ctrl Pts',(-0.307646040500939,3.33112663667463,
3.77096244600287));
#30480=CARTESIAN_POINT('Ctrl Pts',(-0.303203848073521,3.38666124692601,
3.7778675000474));
#30481=CARTESIAN_POINT('Ctrl Pts',(-0.299374978655613,3.44423741493144,
3.78377682303441));
#30482=CARTESIAN_POINT('Ctrl Pts',(-0.296343776557985,3.50350417053243,
3.78841526539902));
#30483=CARTESIAN_POINT('Ctrl Pts',(-0.293416735114649,3.56073435323517,
3.79289431780017));
#30484=CARTESIAN_POINT('Ctrl Pts',(-0.29123348268165,3.61954059473043,3.79618800351884));
#30485=CARTESIAN_POINT('Ctrl Pts',(-0.289960005341534,3.67958500427146,
3.79809165618784));
#30486=CARTESIAN_POINT('Ctrl Pts',(-0.289119428723424,3.71921816076234,
3.79934818888941));
#30487=CARTESIAN_POINT('Ctrl Pts',(-0.288675227064339,3.75939032158238,
3.79999999999563));
#30488=CARTESIAN_POINT('Ctrl Pts',(-0.288675134594801,3.79999999959147,
3.8));
#30489=CARTESIAN_POINT('Ctrl Pts',(0.09332729536784,0.2663525855947,-2.027339375446));
#30490=CARTESIAN_POINT('Ctrl Pts',(0.0956460765109,0.2627254329722,-2.020940474449));
#30491=CARTESIAN_POINT('Ctrl Pts',(0.1067234777855,0.2452163007571,-1.98987166704));
#30492=CARTESIAN_POINT('Ctrl Pts',(0.1252614819808,0.2144240760922,-1.933661042191));
#30493=CARTESIAN_POINT('Ctrl Pts',(0.1483230597314,0.1738236541099,-1.855915420958));
#30494=CARTESIAN_POINT('Ctrl Pts',(0.1706856731413,0.1325495117081,-1.772637372698));
#30495=CARTESIAN_POINT('Ctrl Pts',(0.1930020158897,0.08995564733656,-1.681442257421));
#30496=CARTESIAN_POINT('Ctrl Pts',(0.2153249421398,0.04637396170794,-1.581617848906));
#30497=CARTESIAN_POINT('Ctrl Pts',(0.237760929357,0.002207589586509,-1.472368077024));
#30498=CARTESIAN_POINT('Ctrl Pts',(0.2604508155607,-0.04209002824358,-1.352628361368));
#30499=CARTESIAN_POINT('Ctrl Pts',(0.2834723960102,-0.08579256744141,-1.221593810851));
#30500=CARTESIAN_POINT('Ctrl Pts',(0.3069634986954,-0.1280921905644,-1.078167578903));
#30501=CARTESIAN_POINT('Ctrl Pts',(0.3311487111769,-0.1680644146237,-0.9208497005944));
#30502=CARTESIAN_POINT('Ctrl Pts',(0.3564829869058,-0.2046987259317,-0.7467239997496));
#30503=CARTESIAN_POINT('Ctrl Pts',(0.383183258108,-0.2361911499073,-0.5536747851934));
#30504=CARTESIAN_POINT('Ctrl Pts',(0.4118738384147,-0.2601195235891,-0.3402017808901));
#30505=CARTESIAN_POINT('Ctrl Pts',(0.4323948723823,-0.2689470860258,-0.1832271812612));
#30506=CARTESIAN_POINT('Ctrl Pts',(0.4433244432103,-0.2710639706472,-0.09819688475105));
#30507=CARTESIAN_POINT('Ctrl Pts',(0.4441525558925,-0.2712093650815,-0.09174594482558));
#30508=CARTESIAN_POINT('Ctrl Pts',(0.004133716395932,0.4140946903737,-1.91818759396));
#30509=CARTESIAN_POINT('Ctrl Pts',(0.006375610685108,0.4107521532303,-1.912236954105));
#30510=CARTESIAN_POINT('Ctrl Pts',(0.01709859516906,0.3946002443624,-1.883314369697));
#30511=CARTESIAN_POINT('Ctrl Pts',(0.03514371433922,0.3660649704597,-1.830747145249));
#30512=CARTESIAN_POINT('Ctrl Pts',(0.05770123147569,0.3282842837314,-1.757747888332));
#30513=CARTESIAN_POINT('Ctrl Pts',(0.0796798615306,0.2897221082235,-1.679243883391));
#30514=CARTESIAN_POINT('Ctrl Pts',(0.1016848560021,0.2498171933258,-1.593045679998));
#30515=CARTESIAN_POINT('Ctrl Pts',(0.123750946579,0.2089035319323,-1.498504779354));
#30516=CARTESIAN_POINT('Ctrl Pts',(0.1459810956979,0.1673646699477,-1.394842391727));
#30517=CARTESIAN_POINT('Ctrl Pts',(0.1685009069597,0.1256530218562,-1.281076556188));
#30518=CARTESIAN_POINT('Ctrl Pts',(0.1913848392552,0.08446552394875,-1.156432362992));
#30519=CARTESIAN_POINT('Ctrl Pts',(0.2147620673246,0.04458670410526,-1.019885111451));
#30520=CARTESIAN_POINT('Ctrl Pts',(0.2388605698404,0.006899880930569,-0.8699663883086));
#30521=CARTESIAN_POINT('Ctrl Pts',(0.2641204729043,-0.02760311364001,-0.7039575843831));
#30522=CARTESIAN_POINT('Ctrl Pts',(0.2907706259586,-0.05720484323787,-0.5197608497958));
#30523=CARTESIAN_POINT('Ctrl Pts',(0.3194378379588,-0.07956950255824,-0.3159115398517));
#30524=CARTESIAN_POINT('Ctrl Pts',(0.3399248718625,-0.08765027203072,-0.166143302502));
#30525=CARTESIAN_POINT('Ctrl Pts',(0.3508467599435,-0.08948791449151,-0.08495485013422));
#30526=CARTESIAN_POINT('Ctrl Pts',(0.3516743579076,-0.08961280997143,-0.07879497185162));
#30527=CARTESIAN_POINT('Ctrl Pts',(-0.1656119288838,0.4794541755272,-1.825386409491));
#30528=CARTESIAN_POINT('Ctrl Pts',(-0.1635163591258,0.4764802331255,-1.81996392764));
#30529=CARTESIAN_POINT('Ctrl Pts',(-0.1534678705812,0.4620697875466,-1.79353716736));
#30530=CARTESIAN_POINT('Ctrl Pts',(-0.1363607683355,0.4363025257814,-1.744942128327));
#30531=CARTESIAN_POINT('Ctrl Pts',(-0.1147625365557,0.401817534727,-1.676772747774));
#30532=CARTESIAN_POINT('Ctrl Pts',(-0.09351467101445,0.3662552687182,-1.602739197825));
#30533=CARTESIAN_POINT('Ctrl Pts',(-0.07210220814432,0.3291973603179,-1.520912659697));
#30534=CARTESIAN_POINT('Ctrl Pts',(-0.05052490541033,0.2910078739752,-1.430734790665));
#30535=CARTESIAN_POINT('Ctrl Pts',(-0.02868648988052,0.2520567001868,-1.331405236481));
#30536=CARTESIAN_POINT('Ctrl Pts',(-0.006490350805663,0.2128285287965,-1.222048142703));
#30537=CARTESIAN_POINT('Ctrl Pts',(0.01613162121186,0.1740090831683,-1.101895162335));
#30538=CARTESIAN_POINT('Ctrl Pts',(0.03929213278289,0.1363916820305,-0.9700014892297));
#30539=CARTESIAN_POINT('Ctrl Pts',(0.0632256162551,0.1008368490525,-0.8248557918097));
#30540=CARTESIAN_POINT('Ctrl Pts',(0.08834397957883,0.06837116739273,-0.6639649220209));
#30541=CARTESIAN_POINT('Ctrl Pts',(0.1148987520299,0.04065350496847,-0.4851100355562));
#30542=CARTESIAN_POINT('Ctrl Pts',(0.1435214914534,0.02000868274697,-0.2867927966161));
#30543=CARTESIAN_POINT('Ctrl Pts',(0.163943819323,0.01294768061339,-0.1413866086486));
#30544=CARTESIAN_POINT('Ctrl Pts',(0.1748512775237,0.01158181464608,-0.06242107600965));
#30545=CARTESIAN_POINT('Ctrl Pts',(0.1756779116267,0.01149231638014,-0.05642892400297));
#30546=CARTESIAN_POINT('Ctrl Pts',(-0.3607780994109,0.4412029905006,-1.779076638338));
#30547=CARTESIAN_POINT('Ctrl Pts',(-0.3588507672437,0.4385619065362,-1.774090671374));
#30548=CARTESIAN_POINT('Ctrl Pts',(-0.3495777848353,0.4257115558353,-1.749698719792));
#30549=CARTESIAN_POINT('Ctrl Pts',(-0.3335491737094,0.402324347319,-1.70411452853));
#30550=CARTESIAN_POINT('Ctrl Pts',(-0.3130538865687,0.370540606216,-1.639289845029));
#30551=CARTESIAN_POINT('Ctrl Pts',(-0.2926462223267,0.3372918543045,-1.567971206541));
#30552=CARTESIAN_POINT('Ctrl Pts',(-0.2719150265569,0.3023143326515,-1.488471217684));
#30553=CARTESIAN_POINT('Ctrl Pts',(-0.2508997108556,0.2660203897208,-1.400318838748));
#30554=CARTESIAN_POINT('Ctrl Pts',(-0.2295116935927,0.2287766291807,-1.302660309974));
#30555=CARTESIAN_POINT('Ctrl Pts',(-0.2076876987407,0.191122835208,-1.194714908186));
#30556=CARTESIAN_POINT('Ctrl Pts',(-0.1853669172732,0.1537553352,-1.07569529903));
#30557=CARTESIAN_POINT('Ctrl Pts',(-0.1624555769196,0.1175054839721,-0.9447183706796));
#30558=CARTESIAN_POINT('Ctrl Pts',(-0.1387118251765,0.08323678325404,-0.80016934265));
#30559=CARTESIAN_POINT('Ctrl Pts',(-0.1137561980987,0.05205271358332,-0.6397351948212));
#30560=CARTESIAN_POINT('Ctrl Pts',(-0.08731109012258,0.02560056658367,-0.4609765504096));
#30561=CARTESIAN_POINT('Ctrl Pts',(-0.05873948333614,0.006273119797196,
-0.2623030025696));
#30562=CARTESIAN_POINT('Ctrl Pts',(-0.03839155165444,0.0001736500266636,
-0.1169978048482));
#30563=CARTESIAN_POINT('Ctrl Pts',(-0.02750058379875,-0.0006811329928475,
-0.03791428735169));
#30564=CARTESIAN_POINT('Ctrl Pts',(-0.02667504964837,-0.0007318324155962,
-0.03191205058213));
#30565=CARTESIAN_POINT('',(0.0865744907536029,0.276461867453166,-1.99263825429456));
#30566=CARTESIAN_POINT('Ctrl Pts',(0.086572192368048,0.27646163366543,-1.99263802090364));
#30567=CARTESIAN_POINT('Ctrl Pts',(0.0865723894795379,0.276461279743604,
-1.99263643431398));
#30568=CARTESIAN_POINT('Ctrl Pts',(0.0865725865894618,0.276460925821444,
-1.99263484772351));
#30569=CARTESIAN_POINT('Ctrl Pts',(0.0865727836978197,0.27646057189895,
-1.99263326113225));
#30570=CARTESIAN_POINT('Ctrl Pts',(0.0891567115206156,0.271820940228061,
-1.97183435972548));
#30571=CARTESIAN_POINT('Ctrl Pts',(0.0914671231050367,0.267125712631713,
-1.95089962877548));
#30572=CARTESIAN_POINT('Ctrl Pts',(0.0935122293987559,0.262455035110272,
-1.93012905924239));
#30573=CARTESIAN_POINT('Ctrl Pts',(0.0941596821290163,0.260976362376874,
-1.92355338051383));
#30574=CARTESIAN_POINT('Ctrl Pts',(0.0947809196141619,0.259499997507271,
-1.91699407057979));
#30575=CARTESIAN_POINT('Ctrl Pts',(0.0953771352104668,0.258028107912017,
-1.91046048468356));
#30576=CARTESIAN_POINT('Ctrl Pts',(0.0955557312246131,0.257587204291573,
-1.90850335305805));
#30577=CARTESIAN_POINT('Ctrl Pts',(0.0957319805226283,0.257146849192486,
-1.9065485833918));
#30578=CARTESIAN_POINT('Ctrl Pts',(0.0959060097778447,0.256706880517564,
-1.90459553014602));
#30579=CARTESIAN_POINT('Ctrl Pts',(0.097493810682784,0.252692712558751,
-1.88677634389946));
#30580=CARTESIAN_POINT('Ctrl Pts',(0.0989008011237806,0.24870884944417,
-1.8690992935969));
#30581=CARTESIAN_POINT('Ctrl Pts',(0.10017829812544,0.244656350480217,-1.85110290858136));
#30582=CARTESIAN_POINT('Ctrl Pts',(0.100704848599869,0.242986017595427,
-1.84368527468036));
#30583=CARTESIAN_POINT('Ctrl Pts',(0.101208840073355,0.241304288351045,
-1.83621349856648));
#30584=CARTESIAN_POINT('Ctrl Pts',(0.101691640129157,0.239605341791607,
-1.82865576303145));
#30585=CARTESIAN_POINT('Ctrl Pts',(0.101946581634144,0.238708216806738,
-1.82466491744549));
#30586=CARTESIAN_POINT('Ctrl Pts',(0.102195936452327,0.237805832916687,
-1.8206499048855));
#30587=CARTESIAN_POINT('Ctrl Pts',(0.102439497850678,0.23689865123378,-1.81661186663138));
#30588=CARTESIAN_POINT('Ctrl Pts',(0.103898903583166,0.231462871354842,
-1.79241617627995));
#30589=CARTESIAN_POINT('Ctrl Pts',(0.105146699251486,0.225856178570456,
-1.76739479128144));
#30590=CARTESIAN_POINT('Ctrl Pts',(0.106164852738633,0.220154712920121,
-1.74175866230358));
#30591=CARTESIAN_POINT('Ctrl Pts',(0.106419458818648,0.218728967354355,
-1.73534792523084));
#30592=CARTESIAN_POINT('Ctrl Pts',(0.106659590009949,0.217297634713757,
-1.72889885721906));
#30593=CARTESIAN_POINT('Ctrl Pts',(0.106885499617317,0.21586057372366,-1.72240913586726));
#30594=CARTESIAN_POINT('Ctrl Pts',(0.107713756972225,0.21059184545503,-1.69861572794831));
#30595=CARTESIAN_POINT('Ctrl Pts',(0.108351090819835,0.20524572023201,-1.67427586744531));
#30596=CARTESIAN_POINT('Ctrl Pts',(0.108791121039501,0.199822429937497,
-1.64928232445734));
#30597=CARTESIAN_POINT('Ctrl Pts',(0.108951156646876,0.197850020958601,
-1.64019236505506));
#30598=CARTESIAN_POINT('Ctrl Pts',(0.109085136510625,0.195867422628958,
-1.63101618866698));
#30599=CARTESIAN_POINT('Ctrl Pts',(0.109193134880891,0.193875368857428,
-1.62175335534115));
#30600=CARTESIAN_POINT('Ctrl Pts',(0.109463080273659,0.188896166519022,
-1.59860060614561));
#30601=CARTESIAN_POINT('Ctrl Pts',(0.109570286280441,0.183857804617195,
-1.57490650509088));
#30602=CARTESIAN_POINT('Ctrl Pts',(0.10951482512735,0.178775962091305,-1.55067263118934));
#30603=CARTESIAN_POINT('Ctrl Pts',(0.109487072033164,0.176232977562583,
-1.53854585510594));
#30604=CARTESIAN_POINT('Ctrl Pts',(0.109418566296671,0.173679123371706,
-1.52628331173168));
#30605=CARTESIAN_POINT('Ctrl Pts',(0.109308883011478,0.171115928526719,
-1.51387842705374));
#30606=CARTESIAN_POINT('Ctrl Pts',(0.109111685863714,0.166507617317722,
-1.49157595979515));
#30607=CARTESIAN_POINT('Ctrl Pts',(0.10878136088443,0.161869001571485,-1.46881339834872));
#30608=CARTESIAN_POINT('Ctrl Pts',(0.108313218868863,0.157208146484988,
-1.44554692938918));
#30609=CARTESIAN_POINT('Ctrl Pts',(0.108001033258028,0.154100004417399,
-1.43003143071021));
#30610=CARTESIAN_POINT('Ctrl Pts',(0.107627386646029,0.150982306259349,
-1.41429254314733));
#30611=CARTESIAN_POINT('Ctrl Pts',(0.10719200013546,0.14785739335023,-1.39831770099805));
#30612=CARTESIAN_POINT('Ctrl Pts',(0.106611352561574,0.14368989377172,-1.37701305992163));
#30613=CARTESIAN_POINT('Ctrl Pts',(0.10592087243008,0.139509507623095,-1.35528876480802));
#30614=CARTESIAN_POINT('Ctrl Pts',(0.105117695700426,0.135324079865163,
-1.33311775486119));
#30615=CARTESIAN_POINT('Ctrl Pts',(0.104415231498044,0.131663474343298,
-1.31372682850179));
#30616=CARTESIAN_POINT('Ctrl Pts',(0.103626886060035,0.127998649213348,
-1.29399350119365));
#30617=CARTESIAN_POINT('Ctrl Pts',(0.102751909024411,0.124339054087829,
-1.27391565922516));
#30618=CARTESIAN_POINT('Ctrl Pts',(0.101876317049589,0.120676886976531,
-1.25382370642686));
#30619=CARTESIAN_POINT('Ctrl Pts',(0.100913986009255,0.117019958340212,
-1.2333867545795));
#30620=CARTESIAN_POINT('Ctrl Pts',(0.099864286261075,0.113377625644681,
-1.21260144449221));
#30621=CARTESIAN_POINT('Ctrl Pts',(0.0986644170002263,0.109214222684237,
-1.18884259850392));
#30622=CARTESIAN_POINT('Ctrl Pts',(0.0973503045944713,0.105070115399845,
-1.16462961242153));
#30623=CARTESIAN_POINT('Ctrl Pts',(0.0959208955659195,0.100960008497594,
-1.13995065515804));
#30624=CARTESIAN_POINT('Ctrl Pts',(0.0948501598641185,0.0978812269098513,
-1.12146424567172));
#30625=CARTESIAN_POINT('Ctrl Pts',(0.0937147709341765,0.0948215515490566,
-1.10271639655319));
#30626=CARTESIAN_POINT('Ctrl Pts',(0.0925141428635644,0.0917876969243179,
-1.08370349261096));
#30627=CARTESIAN_POINT('Ctrl Pts',(0.090711884050162,0.087233587812719,
-1.05516328558349));
#30628=CARTESIAN_POINT('Ctrl Pts',(0.0887624161433915,0.0827369922636152,
-1.02602400443288));
#30629=CARTESIAN_POINT('Ctrl Pts',(0.0866635512471383,0.078311623003293,
-0.996203974437649));
#30630=CARTESIAN_POINT('Ctrl Pts',(0.085497600329366,0.0758532640304192,
-0.979638500688956));
#30631=CARTESIAN_POINT('Ctrl Pts',(0.0842855705515153,0.0734169891445541,
-0.962862931509203));
#30632=CARTESIAN_POINT('Ctrl Pts',(0.0830271621620788,0.0710055491604767,
-0.945861979442115));
#30633=CARTESIAN_POINT('Ctrl Pts',(0.0805113794233251,0.0661846506839502,
-0.91187404507058));
#30634=CARTESIAN_POINT('Ctrl Pts',(0.0778094210554922,0.0614631819880825,
-0.876988620646972));
#30635=CARTESIAN_POINT('Ctrl Pts',(0.0749072538413882,0.0568696075407514,
-0.841041215753322));
#30636=CARTESIAN_POINT('Ctrl Pts',(0.0737445261640158,0.0550292324851632,
-0.826639205284582));
#30637=CARTESIAN_POINT('Ctrl Pts',(0.0725496940810796,0.0532095281332425,
-0.812066792693763));
#30638=CARTESIAN_POINT('Ctrl Pts',(0.071321326187919,0.0514129525452542,
-0.797314202957885));
#30639=CARTESIAN_POINT('Ctrl Pts',(0.0679485646593548,0.0464800484372401,
-0.756807635353096));
#30640=CARTESIAN_POINT('Ctrl Pts',(0.0643257157371699,0.0417180858650663,
-0.714939461591492));
#30641=CARTESIAN_POINT('Ctrl Pts',(0.0604397797041336,0.0371900436535931,
-0.671518074178239));
#30642=CARTESIAN_POINT('Ctrl Pts',(0.0593779426029125,0.0359527501996705,
-0.659653123301561));
#30643=CARTESIAN_POINT('Ctrl Pts',(0.058296514394975,0.0347330482780736,
-0.647672164086912));
#30644=CARTESIAN_POINT('Ctrl Pts',(0.0571958008445849,0.0335324230205638,
-0.635571162783657));
#30645=CARTESIAN_POINT('Ctrl Pts',(0.0528001609141237,0.0287377911006063,
-0.587246469671356));
#30646=CARTESIAN_POINT('Ctrl Pts',(0.0480918396870737,0.0242470394462572,
-0.537007861922811));
#30647=CARTESIAN_POINT('Ctrl Pts',(0.0430831220032363,0.0201948414791885,
-0.484762336726024));
#30648=CARTESIAN_POINT('Ctrl Pts',(0.0422475647486355,0.0195188514110342,
-0.476046707226787));
#30649=CARTESIAN_POINT('Ctrl Pts',(0.0414037495294555,0.0188551002544172,
-0.467275222038145));
#30650=CARTESIAN_POINT('Ctrl Pts',(0.0405515875419014,0.0182042309408489,
-0.45844730531979));
#30651=CARTESIAN_POINT('Ctrl Pts',(0.0358409313489692,0.0146062981445854,
-0.409647568688297));
#30652=CARTESIAN_POINT('Ctrl Pts',(0.0308772748861987,0.0114003528827624,
-0.359129169797274));
#30653=CARTESIAN_POINT('Ctrl Pts',(0.0256599441662973,0.00870164296594191,
-0.306772181437106));
#30654=CARTESIAN_POINT('Ctrl Pts',(0.0247474568793358,0.0082296509411883,
-0.297615183572278));
#30655=CARTESIAN_POINT('Ctrl Pts',(0.023827246648876,0.007773234547942,
-0.288402053146454));
#30656=CARTESIAN_POINT('Ctrl Pts',(0.0228993572944685,0.0073330928560306,
-0.279132302431854));
#30657=CARTESIAN_POINT('Ctrl Pts',(0.0224196995669689,0.00710556856909132,
-0.274340451397965));
#30658=CARTESIAN_POINT('Ctrl Pts',(0.0219379899997736,0.00688239373712214,
-0.269533471847087));
#30659=CARTESIAN_POINT('Ctrl Pts',(0.0214542272153199,0.00666366350834061,
-0.264711292193313));
#30660=CARTESIAN_POINT('Ctrl Pts',(0.0168726023431542,0.00459211131647106,
-0.219041350333829));
#30661=CARTESIAN_POINT('Ctrl Pts',(0.012107704008177,0.00291832101405385,
-0.171999057778165));
#30662=CARTESIAN_POINT('Ctrl Pts',(0.0071767230354041,0.00173218952277883,
-0.123647703296785));
#30663=CARTESIAN_POINT('Ctrl Pts',(0.00482106357237431,0.00116554327383814,
-0.100548987977606));
#30664=CARTESIAN_POINT('Ctrl Pts',(0.00242773055893293,0.000710192814652613,
-0.0771508945150003));
#30665=CARTESIAN_POINT('Ctrl Pts',(-4.41691394796437E-8,0.000376013360727031,
-0.0534561522398133));
#30666=CARTESIAN_POINT('Origin',(-0.3268616990873,-0.004510051500619,-2.00392196632));
#30667=CARTESIAN_POINT('Ctrl Pts',(0.001363716877125,0.5959039627023,-1.995067420053));
#30668=CARTESIAN_POINT('Ctrl Pts',(-0.0002547629821562,0.5664635602052,
-1.947200740707));
#30669=CARTESIAN_POINT('Ctrl Pts',(-0.004372367677236,0.4912734831306,-1.819803089527));
#30670=CARTESIAN_POINT('Ctrl Pts',(-0.010697518644,0.3716703089505,-1.590379225775));
#30671=CARTESIAN_POINT('Ctrl Pts',(-0.01714467798321,0.2420950677737,-1.288569665529));
#30672=CARTESIAN_POINT('Ctrl Pts',(-0.02256867464757,0.1250955634456,-0.9310228511924));
#30673=CARTESIAN_POINT('Ctrl Pts',(-0.02637651263401,0.03561097409294,-0.5171914444459));
#30674=CARTESIAN_POINT('Ctrl Pts',(-0.02742725699744,0.00614471551626,-0.2127089892193));
#30675=CARTESIAN_POINT('Ctrl Pts',(-0.0274982583504,0.0009348878949177,
-0.05030904096571));
#30676=CARTESIAN_POINT('Ctrl Pts',(-0.02750035356637,0.0007368753892566,
-0.0435739000559));
#30677=CARTESIAN_POINT('Ctrl Pts',(-0.02360189154764,0.2674772673847,-2.008012314209));
#30678=CARTESIAN_POINT('Ctrl Pts',(-0.007100235964077,0.2366788583949,-1.961090142431));
#30679=CARTESIAN_POINT('Ctrl Pts',(0.0350348100739,0.1618430617063,-1.831220908937));
#30680=CARTESIAN_POINT('Ctrl Pts',(0.1002819388271,0.05748454313784,-1.58377920092));
#30681=CARTESIAN_POINT('Ctrl Pts',(0.1674804264519,-0.03345159548168,-1.25031815927));
#30682=CARTESIAN_POINT('Ctrl Pts',(0.2248447651455,-0.08751112646634,-0.8568392396615));
#30683=CARTESIAN_POINT('Ctrl Pts',(0.2662490974893,-0.08993933952185,-0.4123496126141));
#30684=CARTESIAN_POINT('Ctrl Pts',(0.2789069387192,-0.04935013640268,-0.09830602538954));
#30685=CARTESIAN_POINT('Ctrl Pts',(0.280659326246,-0.01693316005029,0.06530116546309));
#30686=CARTESIAN_POINT('Ctrl Pts',(0.2807233254675,-0.01557036011737,0.07207992811515));
#30687=CARTESIAN_POINT('Ctrl Pts',(0.2095583867952,0.03476773911214,-2.019596510591));
#30688=CARTESIAN_POINT('Ctrl Pts',(0.2389857802896,0.01651651743335,-1.964918501646));
#30689=CARTESIAN_POINT('Ctrl Pts',(0.3101581568231,-0.02378135277356,-1.8140793846));
#30690=CARTESIAN_POINT('Ctrl Pts',(0.4068616564537,-0.06360695540912,-1.532524925838));
#30691=CARTESIAN_POINT('Ctrl Pts',(0.4886889080963,-0.07025856326138,-1.166376398116));
#30692=CARTESIAN_POINT('Ctrl Pts',(0.5374668975788,-0.0301895956346,-0.7523865517121));
#30693=CARTESIAN_POINT('Ctrl Pts',(0.5443422263587,0.06410224085544,-0.306016547345));
#30694=CARTESIAN_POINT('Ctrl Pts',(0.5164520353949,0.1626419470658,-0.005351407090899));
#30695=CARTESIAN_POINT('Ctrl Pts',(0.4928891039187,0.2211875903434,0.1483861234045));
#30696=CARTESIAN_POINT('Ctrl Pts',(0.4918968454427,0.2236257229715,0.1547511527327));
#30697=CARTESIAN_POINT('Ctrl Pts',(0.5381945238366,0.06011096769621,-2.021739002091));
#30698=CARTESIAN_POINT('Ctrl Pts',(0.5663364060878,0.05955934821613,-1.956015197361));
#30699=CARTESIAN_POINT('Ctrl Pts',(0.6290746726958,0.06388977555888,-1.780336254063));
#30700=CARTESIAN_POINT('Ctrl Pts',(0.6951750183963,0.09286790168404,-1.472370815216));
#30701=CARTESIAN_POINT('Ctrl Pts',(0.722409287336,0.1573502975438,-1.095301225048));
#30702=CARTESIAN_POINT('Ctrl Pts',(0.6972159851597,0.2570732908323,-0.6905298257101));
#30703=CARTESIAN_POINT('Ctrl Pts',(0.6139081869808,0.390278014667,-0.2723690173986));
#30704=CARTESIAN_POINT('Ctrl Pts',(0.5194992042508,0.4942376361727,0.001310753365298));
#30705=CARTESIAN_POINT('Ctrl Pts',(0.4611419320742,0.5491867406386,0.140986686312));
#30706=CARTESIAN_POINT('Ctrl Pts',(0.4587078974379,0.5514645860387,0.1467692430352));
#30707=CARTESIAN_POINT('',(0.517453073023301,0.0581490680041601,-2.00135351550452));
#30708=CARTESIAN_POINT('Origin',(0.5,0.5574505945004,-1.981381677743));
#30709=CARTESIAN_POINT('',(0.0174497466342749,0.000631384652492612,-0.0468912686246816));
#30710=CARTESIAN_POINT('Ctrl Pts',(0.5174542977566,0.05814216397504,-2.00131664892));
#30711=CARTESIAN_POINT('Ctrl Pts',(0.5174639416778,0.05475396251608,-1.917084695768));
#30712=CARTESIAN_POINT('Ctrl Pts',(0.5075557516816,0.04777984816496,-1.740184484562));
#30713=CARTESIAN_POINT('Ctrl Pts',(0.4629797196812,0.03689526489914,-1.449958596358));
#30714=CARTESIAN_POINT('Ctrl Pts',(0.3893196154359,0.02615576871374,-1.136163711401));
#30715=CARTESIAN_POINT('Ctrl Pts',(0.2880099327639,0.01602335717792,-0.7982355138282));
#30716=CARTESIAN_POINT('Ctrl Pts',(0.1627480055582,0.007130463259151,-0.4370888248374));
#30717=CARTESIAN_POINT('Ctrl Pts',(0.06701238076293,0.002487361406222,-0.1800461149003));
#30718=CARTESIAN_POINT('Ctrl Pts',(0.01744974438142,0.0006314603528128,
-0.04689126959127));
#30719=CARTESIAN_POINT('Origin',(-1.165507207395E-9,0.5003265405398,-0.04642263385298));
#30720=CARTESIAN_POINT('Ctrl Pts',(0.006092677297575,0.0006211886451104,
-0.06868317847516));
#30721=CARTESIAN_POINT('Ctrl Pts',(0.003734755652693,0.0005321863950901,
-0.06378738842989));
#30722=CARTESIAN_POINT('Ctrl Pts',(-0.0004662461385957,0.0003735846093764,
-0.0539892436276));
#30723=CARTESIAN_POINT('Ctrl Pts',(-0.005281917808373,0.000191741613253,
-0.03903695947574));
#30724=CARTESIAN_POINT('Ctrl Pts',(-0.008492810860386,7.047881929461E-5,
-0.02433820698463));
#30725=CARTESIAN_POINT('Ctrl Pts',(-0.01020745238675,5.717916985109E-6,
-0.009761485291432));
#30726=CARTESIAN_POINT('Ctrl Pts',(-0.01046402050289,-3.972854523874E-6,
0.005086971193826));
#30727=CARTESIAN_POINT('Ctrl Pts',(-0.009120895507617,4.675707571391E-5,
0.0206052220199));
#30728=CARTESIAN_POINT('Ctrl Pts',(-0.005888618210501,0.0001688308862598,
0.03701638652806));
#30729=CARTESIAN_POINT('Ctrl Pts',(-0.0007646346092876,0.000362319517914,
0.05329605733798));
#30730=CARTESIAN_POINT('Ctrl Pts',(0.003740802969237,0.000532414618925,
0.06380088841363));
#30731=CARTESIAN_POINT('Ctrl Pts',(0.006102566108989,0.0006215605327993,
0.06870005168943));
#30732=CARTESIAN_POINT('Ctrl Pts',(0.01191131197223,0.0005749797399242,
-0.0658677090212));
#30733=CARTESIAN_POINT('Ctrl Pts',(0.00963371057603,0.0004892299014565,
-0.06113683657842));
#30734=CARTESIAN_POINT('Ctrl Pts',(0.005585856909428,0.0003368091360034,
-0.05169022499205));
#30735=CARTESIAN_POINT('Ctrl Pts',(0.0009633490093534,0.0001627225989566,
-0.03732842304272));
#30736=CARTESIAN_POINT('Ctrl Pts',(-0.002109362176125,4.698878340268E-5,
-0.02325255344655));
#30737=CARTESIAN_POINT('Ctrl Pts',(-0.003746892799021,-1.469338550221E-5,
-0.009321455256237));
#30738=CARTESIAN_POINT('Ctrl Pts',(-0.003991703710451,-2.39151618659E-5,
0.004857311811217));
#30739=CARTESIAN_POINT('Ctrl Pts',(-0.002709569206432,2.438079570959E-5,
0.01968209560004));
#30740=CARTESIAN_POINT('Ctrl Pts',(0.0003816499484515,0.0001408144285733,
0.03538922245701));
#30741=CARTESIAN_POINT('Ctrl Pts',(0.005298322943173,0.000325982175415,
0.05102182560571));
#30742=CARTESIAN_POINT('Ctrl Pts',(0.009639551536444,0.0004894497837499,
0.06114990277001));
#30743=CARTESIAN_POINT('Ctrl Pts',(0.01192093360861,0.0005753410642185,
0.06588431050857));
#30744=CARTESIAN_POINT('Ctrl Pts',(0.01772876858441,0.0006541169916031,
-0.06305053973395));
#30745=CARTESIAN_POINT('Ctrl Pts',(0.01553153160975,0.0005716213667831,
-0.05848468665063));
#30746=CARTESIAN_POINT('Ctrl Pts',(0.01163691029307,0.0004253850445901,
-0.04938982358326));
#30747=CARTESIAN_POINT('Ctrl Pts',(0.007207672394919,0.0002590592591866,
-0.03561886171171));
#30748=CARTESIAN_POINT('Ctrl Pts',(0.004273219070382,0.0001488574804655,
-0.0221662498297));
#30749=CARTESIAN_POINT('Ctrl Pts',(0.002712841758818,9.02557475416E-5,-0.008881161993923));
#30750=CARTESIAN_POINT('Ctrl Pts',(0.002479794518074,8.150322565388E-5,
0.004627515065121));
#30751=CARTESIAN_POINT('Ctrl Pts',(0.003700904988553,0.0001273638646299,
0.01875841664537));
#30752=CARTESIAN_POINT('Ctrl Pts',(0.006650988424963,0.0002381542001466,
0.03376108270538));
#30753=CARTESIAN_POINT('Ctrl Pts',(0.01136023680079,0.0004149964575127,
0.04874622628719));
#30754=CARTESIAN_POINT('Ctrl Pts',(0.01553716610055,0.0005718329029132,
0.05849731878084));
#30755=CARTESIAN_POINT('Ctrl Pts',(0.01773812289881,0.000654467746636,0.06306686930469));
#30756=CARTESIAN_POINT('Ctrl Pts',(0.02354285942016,0.0008585706397761,
-0.06023273003868));
#30757=CARTESIAN_POINT('Ctrl Pts',(0.02142600081806,0.0007793298069184,
-0.05583193601455));
#30758=CARTESIAN_POINT('Ctrl Pts',(0.01768463845196,0.0006392790252621,
-0.04708890449065));
#30759=CARTESIAN_POINT('Ctrl Pts',(0.01344870410678,0.0004807153655589,
-0.0339089183807));
#30760=CARTESIAN_POINT('Ctrl Pts',(0.01065253264431,0.0003760466017198,
-0.02107970464963));
#30761=CARTESIAN_POINT('Ctrl Pts',(0.009169322037649,0.0003205258489241,
-0.008440771081267));
#30762=CARTESIAN_POINT('Ctrl Pts',(0.008948040509729,0.0003122426643748,
0.00439766737295));
#30763=CARTESIAN_POINT('Ctrl Pts',(0.01010811635309,0.0003556675546408,
0.01783453251478));
#30764=CARTESIAN_POINT('Ctrl Pts',(0.01291703957031,0.0004608135953648,
0.03213257955172));
#30765=CARTESIAN_POINT('Ctrl Pts',(0.01741882731899,0.0006293288894782,
0.04647011514478));
#30766=CARTESIAN_POINT('Ctrl Pts',(0.0214314288034,0.0007795329954019,0.05584413397741));
#30767=CARTESIAN_POINT('Ctrl Pts',(0.02355194636618,0.0008589108236551,
0.06024878760529));
#30768=CARTESIAN_POINT('',(0.01744974833007,0.0006313468236252,0.04689126965548));
#30769=CARTESIAN_POINT('Ctrl Pts',(0.0174497479592083,0.000631346809740766,
-0.0468912686588925));
#30770=CARTESIAN_POINT('Ctrl Pts',(0.0157883609881824,0.000569144385170808,
-0.042428263604913));
#30771=CARTESIAN_POINT('Ctrl Pts',(0.0143880925285003,0.000516716746237668,
-0.0380261499390857));
#30772=CARTESIAN_POINT('Ctrl Pts',(0.0132318096816563,0.000473426719980336,
-0.0337070287085344));
#30773=CARTESIAN_POINT('Ctrl Pts',(0.012075526745096,0.000430136690364122,
-0.0293879071428618));
#30774=CARTESIAN_POINT('Ctrl Pts',(0.0111632296390876,0.00039597912474571,
-0.0251517780112341));
#30775=CARTESIAN_POINT('Ctrl Pts',(0.0104662607830076,0.000369883996918147,
-0.0209620713811407));
#30776=CARTESIAN_POINT('Ctrl Pts',(0.00976929192692803,0.000343788869090604,
-0.0167723647510503));
#30777=CARTESIAN_POINT('Ctrl Pts',(0.00928765138909347,0.000325754222720897,
-0.0126290806302953));
#30778=CARTESIAN_POINT('Ctrl Pts',(0.00900722076971805,0.000315257154874697,
-0.00847390166297909));
#30779=CARTESIAN_POINT('Ctrl Pts',(0.00872679015034244,0.00030476008702849,
-0.00431872269566002));
#30780=CARTESIAN_POINT('Ctrl Pts',(0.00864756965543408,0.000301794698414069,
-0.000151648881534076));
#30781=CARTESIAN_POINT('Ctrl Pts',(0.00879065645835876,0.00030714892521388,
0.00415254495726168));
#30782=CARTESIAN_POINT('Ctrl Pts',(0.00893374326128334,0.000312503152013687,
0.00845673879605441));
#30783=CARTESIAN_POINT('Ctrl Pts',(0.00929913705597671,0.000326185758752549,
0.0128980526579098));
#30784=CARTESIAN_POINT('Ctrl Pts',(0.00993647955010509,0.000350048854730892,
0.017490916144555));
#30785=CARTESIAN_POINT('Ctrl Pts',(0.0105738220442339,0.000373911950709252,
0.0220837796312034));
#30786=CARTESIAN_POINT('Ctrl Pts',(0.0114831132114847,0.000407956289444159,
0.0268281927430151));
#30787=CARTESIAN_POINT('Ctrl Pts',(0.0127186536112733,0.000454214065906362,
0.0317313795019498));
#30788=CARTESIAN_POINT('Ctrl Pts',(0.013954194011061,0.000500471842368533,
0.0366345662608811));
#30789=CARTESIAN_POINT('Ctrl Pts',(0.0155159835211523,0.000558946556874616,
0.0416965266644137));
#30790=CARTESIAN_POINT('Ctrl Pts',(0.01744974833007,0.000631346823626039,
0.04689126965548));
#30791=CARTESIAN_POINT('Origin',(-3.054478024959E-10,0.500326540572,0.0464226361404));
#30792=CARTESIAN_POINT('Ctrl Pts',(-0.02750316139292,0.000737046107151,
0.04358922770264));
#30793=CARTESIAN_POINT('Ctrl Pts',(-0.02750089427334,0.0009349916310092,
0.0503203531369));
#30794=CARTESIAN_POINT('Ctrl Pts',(-0.02742485534677,0.006227555794608,
0.215269551417));
#30795=CARTESIAN_POINT('Ctrl Pts',(-0.02635280173773,0.03636739278822,0.5234275620995));
#30796=CARTESIAN_POINT('Ctrl Pts',(-0.02245453925619,0.1277268866354,0.9410069594231));
#30797=CARTESIAN_POINT('Ctrl Pts',(-0.01694441566883,0.2463169338229,1.299793310531));
#30798=CARTESIAN_POINT('Ctrl Pts',(-0.0104233500914,0.3770396234592,1.601669677065));
#30799=CARTESIAN_POINT('Ctrl Pts',(-0.004150342494761,0.4953591802118,1.82694866898));
#30800=CARTESIAN_POINT('Ctrl Pts',(-0.0001379825129479,0.5685899304984,
1.950653360374));
#30801=CARTESIAN_POINT('Ctrl Pts',(0.00136439425857,0.5959155261576,1.995080420042));
#30802=CARTESIAN_POINT('Ctrl Pts',(0.2807219033002,-0.01557494114624,-0.07206410546613));
#30803=CARTESIAN_POINT('Ctrl Pts',(0.2806561737658,-0.01693705404338,-0.06529447791634));
#30804=CARTESIAN_POINT('Ctrl Pts',(0.2788362287107,-0.04986605013889,0.1007651614235));
#30805=CARTESIAN_POINT('Ctrl Pts',(0.2659383333367,-0.09061371251157,0.418903610299));
#30806=CARTESIAN_POINT('Ctrl Pts',(0.2235950281925,-0.08686708797216,0.867690420062));
#30807=CARTESIAN_POINT('Ctrl Pts',(0.1653583372217,-0.03098330080804,1.262746140425));
#30808=CARTESIAN_POINT('Ctrl Pts',(0.09742648092702,0.06171309111801,1.596177405319));
#30809=CARTESIAN_POINT('Ctrl Pts',(0.0327510301912,0.1657560048726,1.838700874606));
#30810=CARTESIAN_POINT('Ctrl Pts',(-0.008292099066429,0.2388992121263,1.964475131896));
#30811=CARTESIAN_POINT('Ctrl Pts',(-0.02360837126204,0.26748382362,2.008025395665));
#30812=CARTESIAN_POINT('Ctrl Pts',(0.4918992607781,0.2236194238177,-0.154735914236));
#30813=CARTESIAN_POINT('Ctrl Pts',(0.4928878083092,0.2211824821229,-0.1483835574529));
#30814=CARTESIAN_POINT('Ctrl Pts',(0.5167500083103,0.1617115780388,0.007565532273837));
#30815=CARTESIAN_POINT('Ctrl Pts',(0.5448287089644,0.06217287105558,0.3123858450131));
#30816=CARTESIAN_POINT('Ctrl Pts',(0.5368240119861,-0.03202577563772,0.7634855185153));
#30817=CARTESIAN_POINT('Ctrl Pts',(0.4864905623783,-0.07085440170093,1.179726783911));
#30818=CARTESIAN_POINT('Ctrl Pts',(0.4030125096111,-0.06257200120437,1.546392400176));
#30819=CARTESIAN_POINT('Ctrl Pts',(0.3064646604076,-0.02184495218348,1.822739961703));
#30820=CARTESIAN_POINT('Ctrl Pts',(0.2368627668342,0.01782842154317,1.968863315844));
#30821=CARTESIAN_POINT('Ctrl Pts',(0.20954953649,0.0347661639898,2.019612509741));
#30822=CARTESIAN_POINT('Ctrl Pts',(0.4587131901114,0.5514599684041,-0.1467549726057));
#30823=CARTESIAN_POINT('Ctrl Pts',(0.4611428327526,0.5491832199421,-0.1409845745533));
#30824=CARTESIAN_POINT('Ctrl Pts',(0.5203496374827,0.4933654935977,0.0006860175196782));
#30825=CARTESIAN_POINT('Ctrl Pts',(0.6157665169565,0.3881443830302,0.2781802504261));
#30826=CARTESIAN_POINT('Ctrl Pts',(0.6987262516413,0.2539939406104,0.7010848027865));
#30827=CARTESIAN_POINT('Ctrl Pts',(0.7224328581585,0.1545174083523,1.108648913658));
#30828=CARTESIAN_POINT('Ctrl Pts',(0.6931602429224,0.09088468309498,1.487044303164));
#30829=CARTESIAN_POINT('Ctrl Pts',(0.6260499982531,0.06342531207403,1.790200141908));
#30830=CARTESIAN_POINT('Ctrl Pts',(0.5643084424037,0.05959486348343,1.96075674842));
#30831=CARTESIAN_POINT('Ctrl Pts',(0.5381889316308,0.06010461940414,2.021758679482));
#30832=CARTESIAN_POINT('',(0.0865743867590526,0.276459412161963,1.99264095059477));
#30833=CARTESIAN_POINT('Ctrl Pts',(-9.09801138851544E-7,0.000376077721329259,
0.0534607252662348));
#30834=CARTESIAN_POINT('Ctrl Pts',(0.00652835314144758,0.00127246330365846,
0.117157269627312));
#30835=CARTESIAN_POINT('Ctrl Pts',(0.0127944512297398,0.0030456007331035,
0.178629296439096));
#30836=CARTESIAN_POINT('Ctrl Pts',(0.0187482386330756,0.00549398588579434,
0.237760295451468));
#30837=CARTESIAN_POINT('Ctrl Pts',(0.0205286495875721,0.0062261470214498,
0.255442733748302));
#30838=CARTESIAN_POINT('Ctrl Pts',(0.0222814724261678,0.0070187559964705,
0.272915929701867));
#30839=CARTESIAN_POINT('Ctrl Pts',(0.0240062157849765,0.00786654683602309,
0.290177057805191));
#30840=CARTESIAN_POINT('Ctrl Pts',(0.0299524099712426,0.0107893752879032,
0.349686212632305));
#30841=CARTESIAN_POINT('Ctrl Pts',(0.0355590334273618,0.0143650914300685,
0.406673541011523));
#30842=CARTESIAN_POINT('Ctrl Pts',(0.040830769447185,0.0184196009791735,
0.461351968844045));
#30843=CARTESIAN_POINT('Ctrl Pts',(0.0422015721807883,0.0194738898799141,
0.475569930073535));
#30844=CARTESIAN_POINT('Ctrl Pts',(0.0435499058409064,0.0205607528992102,
0.489631863372403));
#30845=CARTESIAN_POINT('Ctrl Pts',(0.0448761834508286,0.0216775220448886,
0.50354169221264));
#30846=CARTESIAN_POINT('Ctrl Pts',(0.0450702352677852,0.0218409200244811,
0.505576882688457));
#30847=CARTESIAN_POINT('Ctrl Pts',(0.0452638122696533,0.0220049588166182,
0.507608814414488));
#30848=CARTESIAN_POINT('Ctrl Pts',(0.0454569139116692,0.0221696311704481,
0.509637503452834));
#30849=CARTESIAN_POINT('Ctrl Pts',(0.0504911582929488,0.0264627115573665,
0.562526315200067));
#30850=CARTESIAN_POINT('Ctrl Pts',(0.0552009765120379,0.0311819748374701,
0.613211073235368));
#30851=CARTESIAN_POINT('Ctrl Pts',(0.059585318651173,0.0362023190716366,
0.661979072375273));
#30852=CARTESIAN_POINT('Ctrl Pts',(0.0606025057087322,0.0373670614702519,
0.673293467094923));
#30853=CARTESIAN_POINT('Ctrl Pts',(0.0616022346451153,0.0385482249859112,
0.684504695746438));
#30854=CARTESIAN_POINT('Ctrl Pts',(0.0625845886509375,0.039744617250358,
0.695616355729162));
#30855=CARTESIAN_POINT('Ctrl Pts',(0.067314054123752,0.0455045529488005,
0.749112561702244));
#30856=CARTESIAN_POINT('Ctrl Pts',(0.0716395927107308,0.0516133879646876,
0.800300379856481));
#30857=CARTESIAN_POINT('Ctrl Pts',(0.0755946966027367,0.0579677961016361,
0.849588598140686));
#30858=CARTESIAN_POINT('Ctrl Pts',(0.076137857342939,0.0588404571293751,
0.856357427950849));
#30859=CARTESIAN_POINT('Ctrl Pts',(0.0766740369127634,0.0597178291689939,
0.863090434392253));
#30860=CARTESIAN_POINT('Ctrl Pts',(0.0772033241577391,0.0605997177594687,
0.869788678677261));
#30861=CARTESIAN_POINT('Ctrl Pts',(0.0785440273149263,0.062833572492906,
0.886755566403666));
#30862=CARTESIAN_POINT('Ctrl Pts',(0.079840730238549,0.0650962458724791,
0.903499201468074));
#30863=CARTESIAN_POINT('Ctrl Pts',(0.0810937204906553,0.0673839988051382,
0.920028260063856));
#30864=CARTESIAN_POINT('Ctrl Pts',(0.083937326066278,0.0725759522014398,
0.95754022243048));
#30865=CARTESIAN_POINT('Ctrl Pts',(0.0865557106728475,0.077896178421874,
0.993947062286089));
#30866=CARTESIAN_POINT('Ctrl Pts',(0.0889539161279948,0.0833020208043715,
1.02934740992229));
#30867=CARTESIAN_POINT('Ctrl Pts',(0.0924088532493085,0.091089862950746,
1.08034636620153));
#30868=CARTESIAN_POINT('Ctrl Pts',(0.0954064872304019,0.0990548371110723,
1.12925696354537));
#30869=CARTESIAN_POINT('Ctrl Pts',(0.097957198115787,0.107078805606651,
1.17620683708701));
#30870=CARTESIAN_POINT('Ctrl Pts',(0.0999421648726084,0.113323069044253,
1.21274329394345));
#30871=CARTESIAN_POINT('Ctrl Pts',(0.101656839723861,0.11960376445875,1.24809198876482));
#30872=CARTESIAN_POINT('Ctrl Pts',(0.103114408059529,0.125879416749678,
1.28234280769469));
#30873=CARTESIAN_POINT('Ctrl Pts',(0.103529836038383,0.127668068083146,
1.2921047846353));
#30874=CARTESIAN_POINT('Ctrl Pts',(0.103924381198634,0.12945636796932,1.30177759316701));
#30875=CARTESIAN_POINT('Ctrl Pts',(0.104298386010344,0.131243356550118,
1.31136316830229));
#30876=CARTESIAN_POINT('Ctrl Pts',(0.105984622059922,0.139300163496924,
1.35458063995765));
#30877=CARTESIAN_POINT('Ctrl Pts',(0.107252382666339,0.147329259312068,
1.39602675468255));
#30878=CARTESIAN_POINT('Ctrl Pts',(0.108116417619743,0.155318344975294,
1.43608914702022));
#30879=CARTESIAN_POINT('Ctrl Pts',(0.108980452573148,0.163307430638519,
1.47615153935789));
#30880=CARTESIAN_POINT('Ctrl Pts',(0.109440821161486,0.171256644751982,
1.51483017857233));
#30881=CARTESIAN_POINT('Ctrl Pts',(0.109518134026559,0.179029875568212,
1.55188588983053));
#30882=CARTESIAN_POINT('Ctrl Pts',(0.10954937952823,0.182171377260427,1.56686171936345));
#30883=CARTESIAN_POINT('Ctrl Pts',(0.109517733598986,0.1852845885706,1.58157153761736));
#30884=CARTESIAN_POINT('Ctrl Pts',(0.109424701710558,0.188373020356353,
1.59605530105348));
#30885=CARTESIAN_POINT('Ctrl Pts',(0.109287538484396,0.192926504915998,
1.61740969634115));
#30886=CARTESIAN_POINT('Ctrl Pts',(0.10901734790502,0.197425875042288,1.63827290332916));
#30887=CARTESIAN_POINT('Ctrl Pts',(0.108614123231663,0.201885013497263,
1.65876475480962));
#30888=CARTESIAN_POINT('Ctrl Pts',(0.108197298559382,0.206494550184769,
1.67994775734428));
#30889=CARTESIAN_POINT('Ctrl Pts',(0.107636013113304,0.211064909866213,
1.7007318090833));
#30890=CARTESIAN_POINT('Ctrl Pts',(0.106916313695468,0.21567514026169,1.72156283502369));
#30891=CARTESIAN_POINT('Ctrl Pts',(0.106467581648172,0.218549615455923,
1.73455096407572));
#30892=CARTESIAN_POINT('Ctrl Pts',(0.105956508353049,0.221439865662645,
1.74755699928328));
#30893=CARTESIAN_POINT('Ctrl Pts',(0.105370932926517,0.224367934091294,
1.76068425372678));
#30894=CARTESIAN_POINT('Ctrl Pts',(0.104614139175432,0.228152150076371,
1.7776498292643));
#30895=CARTESIAN_POINT('Ctrl Pts',(0.103730622287019,0.232003387630288,
1.7948137637274));
#30896=CARTESIAN_POINT('Ctrl Pts',(0.102682811222916,0.235980870867143,
1.81251182586718));
#30897=CARTESIAN_POINT('Ctrl Pts',(0.101740077804292,0.239559480120153,
1.82843507309721));
#30898=CARTESIAN_POINT('Ctrl Pts',(0.100664403176851,0.243240281303386,
1.84479084066647));
#30899=CARTESIAN_POINT('Ctrl Pts',(0.0993976726189429,0.247073344449856,
1.86180605447616));
#30900=CARTESIAN_POINT('Ctrl Pts',(0.0992357132674213,0.247563425325909,
1.86398155500184));
#30901=CARTESIAN_POINT('Ctrl Pts',(0.0990705841490034,0.248056005652083,
1.86616780777675));
#30902=CARTESIAN_POINT('Ctrl Pts',(0.0989021290735271,0.24855119856692,
1.86836524213669));
#30903=CARTESIAN_POINT('Ctrl Pts',(0.0971030164000728,0.253839895546632,
1.8918340037331));
#30904=CARTESIAN_POINT('Ctrl Pts',(0.0949363222751762,0.259415398134344,
1.91658901567945));
#30905=CARTESIAN_POINT('Ctrl Pts',(0.0922869113983242,0.265180778941099,
1.94227889863466));
#30906=CARTESIAN_POINT('Ctrl Pts',(0.0905915320651791,0.268870092498646,
1.95871806139862));
#30907=CARTESIAN_POINT('Ctrl Pts',(0.0886979474295743,0.272637052898358,
1.97553922388023));
#30908=CARTESIAN_POINT('Ctrl Pts',(0.0865694808505399,0.276456078074887,
1.99264108439717));
#30909=CARTESIAN_POINT('',(0.517453499953991,0.0581482537155648,2.00134959555289));
#30910=CARTESIAN_POINT('Ctrl Pts',(0.01744974833007,0.0006313468236252,
0.04689126965548));
#30911=CARTESIAN_POINT('Ctrl Pts',(0.06753743330703,0.002506810781753,0.1814388238611));
#30912=CARTESIAN_POINT('Ctrl Pts',(0.1639979857046,0.007200545681001,0.4404924524998));
#30913=CARTESIAN_POINT('Ctrl Pts',(0.2891401437734,0.0161206324859,0.8017214821276));
#30914=CARTESIAN_POINT('Ctrl Pts',(0.3899548010611,0.02623514120806,1.138584886082));
#30915=CARTESIAN_POINT('Ctrl Pts',(0.4632860851713,0.03695536152136,1.451600247463));
#30916=CARTESIAN_POINT('Ctrl Pts',(0.5076215437038,0.04781101990821,1.74099111528));
#30917=CARTESIAN_POINT('Ctrl Pts',(0.5174627880836,0.05476666475408,1.917359950681));
#30918=CARTESIAN_POINT('Ctrl Pts',(0.5174549507661,0.05813997872694,2.001305923414));
#30919=CARTESIAN_POINT('Origin',(0.5,0.5574505945004,1.981381677743));
#30920=CARTESIAN_POINT('Ctrl Pts',(0.4441505898026,-0.2712136506453,0.09177744215382));
#30921=CARTESIAN_POINT('Ctrl Pts',(0.4433243095181,-0.2710682902751,0.0982149450773));
#30922=CARTESIAN_POINT('Ctrl Pts',(0.4319126563181,-0.2688550636628,0.1870059243145));
#30923=CARTESIAN_POINT('Ctrl Pts',(0.4105084687887,-0.2594278398504,0.3505980872243));
#30924=CARTESIAN_POINT('Ctrl Pts',(0.3806737777615,-0.2337260742433,0.5722228281209));
#30925=CARTESIAN_POINT('Ctrl Pts',(0.353019478122,-0.2001401451587,0.7712432567423));
#30926=CARTESIAN_POINT('Ctrl Pts',(0.3268098245248,-0.1612906812422,0.949891806445));
#30927=CARTESIAN_POINT('Ctrl Pts',(0.301767398999,-0.1190354334272,1.110873752657));
#30928=CARTESIAN_POINT('Ctrl Pts',(0.2775004469511,-0.07465283465729,1.256626058425));
#30929=CARTESIAN_POINT('Ctrl Pts',(0.2538473285855,-0.02929051310002,1.388548718725));
#30930=CARTESIAN_POINT('Ctrl Pts',(0.2306285320361,0.01624208910001,1.508164313338));
#30931=CARTESIAN_POINT('Ctrl Pts',(0.207745940936,0.06125122341503,1.61657011171));
#30932=CARTESIAN_POINT('Ctrl Pts',(0.1848495979175,0.1056635488392,1.715813080168));
#30933=CARTESIAN_POINT('Ctrl Pts',(0.1609461047857,0.1507778699002,1.810174952061));
#30934=CARTESIAN_POINT('Ctrl Pts',(0.1337042946383,0.2000534730528,1.907032302569));
#30935=CARTESIAN_POINT('Ctrl Pts',(0.1104061460155,0.2393905012997,1.979544729913));
#30936=CARTESIAN_POINT('Ctrl Pts',(0.09567837415139,0.2626728328007,2.020855911046));
#30937=CARTESIAN_POINT('Ctrl Pts',(0.09337813193119,0.2662727193221,2.027206328594));
#30938=CARTESIAN_POINT('Ctrl Pts',(0.3516735936865,-0.08961443345137,0.07882304454895));
#30939=CARTESIAN_POINT('Ctrl Pts',(0.350847645443,-0.08948955446609,0.08497125195283));
#30940=CARTESIAN_POINT('Ctrl Pts',(0.3394417549389,-0.08756810521069,0.1697648837853));
#30941=CARTESIAN_POINT('Ctrl Pts',(0.3180756196171,-0.0789298656086,0.3258309287581));
#30942=CARTESIAN_POINT('Ctrl Pts',(0.2882640593895,-0.05489063086291,0.5374733705197));
#30943=CARTESIAN_POINT('Ctrl Pts',(0.2606668037211,-0.02331128782057,0.727339125934));
#30944=CARTESIAN_POINT('Ctrl Pts',(0.2345362971097,0.01328668833229,0.8976506379832));
#30945=CARTESIAN_POINT('Ctrl Pts',(0.2095892877488,0.05312819491485,1.051034607763));
#30946=CARTESIAN_POINT('Ctrl Pts',(0.1854463195438,0.09496901379647,1.18976893841));
#30947=CARTESIAN_POINT('Ctrl Pts',(0.1619437477539,0.1377124771179,1.315220328414));
#30948=CARTESIAN_POINT('Ctrl Pts',(0.138910375473,0.180572989123,1.428824558866));
#30949=CARTESIAN_POINT('Ctrl Pts',(0.116252767292,0.222883140253,1.531631702806));
#30950=CARTESIAN_POINT('Ctrl Pts',(0.09364048231002,0.2645458762256,1.625553474633));
#30951=CARTESIAN_POINT('Ctrl Pts',(0.07009425725316,0.3067759181797,1.714671038853));
#30952=CARTESIAN_POINT('Ctrl Pts',(0.04337896997847,0.3527292312924,1.805808681844));
#30953=CARTESIAN_POINT('Ctrl Pts',(0.02066764874299,0.3892243623864,1.87369224103));
#30954=CARTESIAN_POINT('Ctrl Pts',(0.006407516092703,0.4107061153768,1.912158009393));
#30955=CARTESIAN_POINT('Ctrl Pts',(0.004182600943537,0.4140246350262,1.918065761637));
#30956=CARTESIAN_POINT('Ctrl Pts',(0.1756764843761,0.01149244822416,0.05645169963164));
#30957=CARTESIAN_POINT('Ctrl Pts',(0.17485115759,0.01158197569545,0.06243513417433));
#30958=CARTESIAN_POINT('Ctrl Pts',(0.1634561005124,0.01301067790449,0.1449398854909));
#30959=CARTESIAN_POINT('Ctrl Pts',(0.142162384109,0.0205792288548,0.2964239473772));
#30960=CARTESIAN_POINT('Ctrl Pts',(0.1123948451772,0.04280987956687,0.5023434273092));
#30961=CARTESIAN_POINT('Ctrl Pts',(0.08490615253173,0.07240212532535,0.6866379321782));
#30962=CARTESIAN_POINT('Ctrl Pts',(0.05892627421398,0.1068593421783,0.851677617466));
#30963=CARTESIAN_POINT('Ctrl Pts',(0.03416085577481,0.1444520696214,1.000117458598));
#30964=CARTESIAN_POINT('Ctrl Pts',(0.01025384696266,0.1839161130489,1.134060645629));
#30965=CARTESIAN_POINT('Ctrl Pts',(-0.01296221266782,0.2241827829663,1.254905212894));
#30966=CARTESIAN_POINT('Ctrl Pts',(-0.03564269543703,0.2644587861952,1.364006309255));
#30967=CARTESIAN_POINT('Ctrl Pts',(-0.05787212820653,0.3040834971127,1.462390721409));
#30968=CARTESIAN_POINT('Ctrl Pts',(-0.07994380918533,0.3429004915365,1.551819675945));
#30969=CARTESIAN_POINT('Ctrl Pts',(-0.1028101008249,0.3820329385455,1.636246280064));
#30970=CARTESIAN_POINT('Ctrl Pts',(-0.128523338039,0.4242129766637,1.721805374643));
#30971=CARTESIAN_POINT('Ctrl Pts',(-0.1501178408998,0.4572657293956,1.78472613206));
#30972=CARTESIAN_POINT('Ctrl Pts',(-0.1634879877075,0.4764412198706,1.819892205208));
#30973=CARTESIAN_POINT('Ctrl Pts',(-0.1655695444196,0.47939642768,1.825280786222));
#30974=CARTESIAN_POINT('Ctrl Pts',(-0.02667784573403,-0.0007319642824258,
0.03192949709643));
#30975=CARTESIAN_POINT('Ctrl Pts',(-0.02750246349207,-0.0006811764769736,
0.03792619875474));
#30976=CARTESIAN_POINT('Ctrl Pts',(-0.03888513505006,0.0002138505247069,
0.1205939522374));
#30977=CARTESIAN_POINT('Ctrl Pts',(-0.06009558709032,0.006779437368235,
0.2719283687744));
#30978=CARTESIAN_POINT('Ctrl Pts',(-0.08981251210483,0.02764286901391,0.4782430106847));
#30979=CARTESIAN_POINT('Ctrl Pts',(-0.1171763833478,0.05591290450752,0.6623591991827));
#30980=CARTESIAN_POINT('Ctrl Pts',(-0.1429830753047,0.08903539736197,0.8269045289161));
#30981=CARTESIAN_POINT('Ctrl Pts',(-0.1675397077971,0.1252746988455,0.9746599149559));
#30982=CARTESIAN_POINT('Ctrl Pts',(-0.1911754199786,0.1632989348384,1.107594926954));
#30983=CARTESIAN_POINT('Ctrl Pts',(-0.2140620594383,0.2020353250487,1.227193389706));
#30984=CARTESIAN_POINT('Ctrl Pts',(-0.2363368040236,0.240653835145,1.334762175212));
#30985=CARTESIAN_POINT('Ctrl Pts',(-0.2580739379061,0.2784788650227,1.431336257167));
#30986=CARTESIAN_POINT('Ctrl Pts',(-0.2795240541198,0.3152782469921,1.518560016079));
#30987=CARTESIAN_POINT('Ctrl Pts',(-0.3016085856314,0.3521058650065,1.600372605688));
#30988=CARTESIAN_POINT('Ctrl Pts',(-0.3261697059412,0.3912871821253,1.682306192781));
#30989=CARTESIAN_POINT('Ctrl Pts',(-0.346480135901,0.4214151408305,1.741542105517));
#30990=CARTESIAN_POINT('Ctrl Pts',(-0.3588270127402,0.4385277461565,1.774025923849));
#30991=CARTESIAN_POINT('Ctrl Pts',(-0.3607437416807,0.4411556988437,1.778987451663));
#30992=CARTESIAN_POINT('Origin',(-0.3268607615544,-0.004512844089665,2.00391666631));
#30993=CARTESIAN_POINT('Ctrl Pts',(0.1027377857463,0.2516014974679,1.993772793209));
#30994=CARTESIAN_POINT('Ctrl Pts',(0.1018795142078,0.2529091607515,1.99856950602));
#30995=CARTESIAN_POINT('Ctrl Pts',(0.08748606425778,0.2750262500263,2.079318045689));
#30996=CARTESIAN_POINT('Ctrl Pts',(0.06218815931651,0.3199344673338,2.231178832349));
#30997=CARTESIAN_POINT('Ctrl Pts',(0.03182029544458,0.3937152656143,2.449036815776));
#30998=CARTESIAN_POINT('Ctrl Pts',(0.008692153136202,0.4786543405831,2.669750211539));
#30999=CARTESIAN_POINT('Ctrl Pts',(0.0003099300768639,0.5454908414197,2.821709674268));
#31000=CARTESIAN_POINT('Ctrl Pts',(-0.001018477605139,0.5836010689834,2.902151700762));
#31001=CARTESIAN_POINT('Ctrl Pts',(-0.001081418569355,0.5856932619884,2.906550131397));
#31002=CARTESIAN_POINT('Ctrl Pts',(-0.03993386604451,0.4842012940407,1.82477577565));
#31003=CARTESIAN_POINT('Ctrl Pts',(-0.04008326187016,0.4858259304199,1.82941037646));
#31004=CARTESIAN_POINT('Ctrl Pts',(-0.04249896901661,0.5132255431577,1.907411774626));
#31005=CARTESIAN_POINT('Ctrl Pts',(-0.04384834652328,0.5663417760107,2.053551607732));
#31006=CARTESIAN_POINT('Ctrl Pts',(-0.03627411384636,0.6462729463744,2.261605825127));
#31007=CARTESIAN_POINT('Ctrl Pts',(-0.01768977584964,0.730324119387,2.4705330558));
#31008=CARTESIAN_POINT('Ctrl Pts',(0.004566050698213,0.7897246608292,2.612726145468));
#31009=CARTESIAN_POINT('Ctrl Pts',(0.01963083731976,0.8212324290105,2.687391402537));
#31010=CARTESIAN_POINT('Ctrl Pts',(0.02046458526668,0.8229554088081,2.691471916486));
#31011=CARTESIAN_POINT('Ctrl Pts',(-0.3385562814283,0.5122548782035,1.710515139935));
#31012=CARTESIAN_POINT('Ctrl Pts',(-0.3385854937958,0.5146556694714,1.715026264093));
#31013=CARTESIAN_POINT('Ctrl Pts',(-0.3389179244204,0.5551248461428,1.790931560508));
#31014=CARTESIAN_POINT('Ctrl Pts',(-0.3344184843396,0.6329249209683,1.932588547284));
#31015=CARTESIAN_POINT('Ctrl Pts',(-0.312917850693,0.748065379891,2.13267148346));
#31016=CARTESIAN_POINT('Ctrl Pts',(-0.2740805475893,0.8668470835516,2.331716051354));
#31017=CARTESIAN_POINT('Ctrl Pts',(-0.2328066607506,0.9486868685298,2.465517500439));
#31018=CARTESIAN_POINT('Ctrl Pts',(-0.2060460780354,0.9912774222627,2.535169689394));
#31019=CARTESIAN_POINT('Ctrl Pts',(-0.2045679022214,0.993603941535,2.538974208362));
#31020=CARTESIAN_POINT('Ctrl Pts',(-0.592664250327,0.3169298805394,1.727694044175));
#31021=CARTESIAN_POINT('Ctrl Pts',(-0.5932426506397,0.3200449757575,1.732203216897));
#31022=CARTESIAN_POINT('Ctrl Pts',(-0.602784774432,0.3725971593248,1.808070564298));
#31023=CARTESIAN_POINT('Ctrl Pts',(-0.6144625375171,0.4749866408694,1.949492146447));
#31024=CARTESIAN_POINT('Ctrl Pts',(-0.612399990641,0.6307593114652,2.148787406837));
#31025=CARTESIAN_POINT('Ctrl Pts',(-0.5883650519268,0.7965753751741,2.34648704521));
#31026=CARTESIAN_POINT('Ctrl Pts',(-0.5524599168806,0.9156661437381,2.478904894027));
#31027=CARTESIAN_POINT('Ctrl Pts',(-0.5265523235192,0.9795848546602,2.547672988512));
#31028=CARTESIAN_POINT('Ctrl Pts',(-0.5251145852718,0.983082510075,2.551428709617));
#31029=CARTESIAN_POINT('Ctrl Pts',(0.0865773249525696,0.276461408980929,
1.99264087060027));
#31030=CARTESIAN_POINT('Ctrl Pts',(0.0865771947823855,0.27646163218119,
1.9926416609711));
#31031=CARTESIAN_POINT('Ctrl Pts',(0.0865770646123325,0.276461855381553,
1.99264245134172));
#31032=CARTESIAN_POINT('Ctrl Pts',(0.0865769344424107,0.276462078582019,
1.99264324171212));
#31033=CARTESIAN_POINT('Ctrl Pts',(0.078420000105942,0.290448654910433,
2.04217080843749));
#31034=CARTESIAN_POINT('Ctrl Pts',(0.0707810911918314,0.304841755020766,
2.0908545533155));
#31035=CARTESIAN_POINT('Ctrl Pts',(0.0637332814206178,0.319485185859224,
2.13835021057908));
#31036=CARTESIAN_POINT('Ctrl Pts',(0.0597136280289845,0.327836931769758,
2.16543892125728));
#31037=CARTESIAN_POINT('Ctrl Pts',(0.0558856017111063,0.336269535007341,
2.1921414988295));
#31038=CARTESIAN_POINT('Ctrl Pts',(0.0522572081993674,0.344749730813805,
2.21839710659208));
#31039=CARTESIAN_POINT('Ctrl Pts',(0.0471928269709879,0.356586083270145,
2.25504374005737));
#31040=CARTESIAN_POINT('Ctrl Pts',(0.0425107423664863,0.368518464963908,
2.29081396288276));
#31041=CARTESIAN_POINT('Ctrl Pts',(0.0381540197777746,0.380693558702874,
2.32622193849537));
#31042=CARTESIAN_POINT('Ctrl Pts',(0.0339164169991585,0.392535765776565,
2.36066180304628));
#31043=CARTESIAN_POINT('Ctrl Pts',(0.029986260998421,0.404607792760995,
2.3947592227875));
#31044=CARTESIAN_POINT('Ctrl Pts',(0.0263406370667108,0.417078684876168,
2.42897308992216));
#31045=CARTESIAN_POINT('Ctrl Pts',(0.0228702839178175,0.428950013497028,
2.46154205583053));
#31046=CARTESIAN_POINT('Ctrl Pts',(0.0196579772062671,0.441180495440324,
2.49421313164509));
#31047=CARTESIAN_POINT('Ctrl Pts',(0.0167223210422853,0.453948518005868,
2.52735622554626));
#31048=CARTESIAN_POINT('Ctrl Pts',(0.0139677607904214,0.465928901773376,
2.55845477523476));
#31049=CARTESIAN_POINT('Ctrl Pts',(0.0114564603784741,0.478382697242401,
2.58996911427275));
#31050=CARTESIAN_POINT('Ctrl Pts',(0.00923922793228618,0.491480864277342,
2.62218604509979));
#31051=CARTESIAN_POINT('Ctrl Pts',(0.00878499123326938,0.494164240198235,
2.62878621565768));
#31052=CARTESIAN_POINT('Ctrl Pts',(0.00834323197860242,0.496874740632172,
2.63541580115522));
#31053=CARTESIAN_POINT('Ctrl Pts',(0.00791460756900038,0.499613961471066,
2.64207714797975));
#31054=CARTESIAN_POINT('Ctrl Pts',(0.00537502089503349,0.515843762162931,
2.6815454266108));
#31055=CARTESIAN_POINT('Ctrl Pts',(0.00329666449988076,0.533066935814479,
2.72213393305126));
#31056=CARTESIAN_POINT('Ctrl Pts',(0.00190428975338371,0.551309292533906,
2.7635988904245));
#31057=CARTESIAN_POINT('Ctrl Pts',(0.000692060773595733,0.567191448922158,
2.79969910202339));
#31058=CARTESIAN_POINT('Ctrl Pts',(3.33158528145791E-7,0.583845999449411,
2.83646315076817));
#31059=CARTESIAN_POINT('Ctrl Pts',(1.31062334541924E-14,0.6012817622028,
2.873708690212));
#31060=CARTESIAN_POINT('Origin',(-0.5,0.6012817644084,2.87370869249));
#31061=CARTESIAN_POINT('Origin',(0.5,50.,0.));
#31062=CARTESIAN_POINT('',(0.517449748466302,0.145564568504214,3.5677191570162));
#31063=CARTESIAN_POINT('Origin',(0.5,0.6439853496966,3.532050807563));
#31064=CARTESIAN_POINT('Origin',(0.5174497483513,50.,0.));
#31065=CARTESIAN_POINT('Ctrl Pts',(0.001285090917852,0.6712313346096,3.501024393646));
#31066=CARTESIAN_POINT('Ctrl Pts',(0.00100370682231,0.6719071272873,3.510665341527));
#31067=CARTESIAN_POINT('Ctrl Pts',(0.0002345815242706,0.6756478789743,3.563478189283));
#31068=CARTESIAN_POINT('Ctrl Pts',(0.006495759564992,0.6828348068514,3.659504026904));
#31069=CARTESIAN_POINT('Ctrl Pts',(0.03172096583422,0.6932191711605,3.786961238567));
#31070=CARTESIAN_POINT('Ctrl Pts',(0.0735297005907,0.7041454719876,3.91068142931));
#31071=CARTESIAN_POINT('Ctrl Pts',(0.1164371395684,0.7124748329371,3.997808690824));
#31072=CARTESIAN_POINT('Ctrl Pts',(0.1438590078278,0.7170804204961,4.043718664671));
#31073=CARTESIAN_POINT('Ctrl Pts',(0.1489299286299,0.7179117303395,4.051932350288));
#31074=CARTESIAN_POINT('Ctrl Pts',(-0.01806331604683,0.3429577205548,3.52352261367));
#31075=CARTESIAN_POINT('Ctrl Pts',(-0.01835338084308,0.3436566094381,3.533493141926));
#31076=CARTESIAN_POINT('Ctrl Pts',(-0.01914623767077,0.3475252138821,3.588111304264));
#31077=CARTESIAN_POINT('Ctrl Pts',(-0.01269201706095,0.3549578839107,3.687418512264));
#31078=CARTESIAN_POINT('Ctrl Pts',(0.01331034779256,0.3656975079899,3.819229367317));
#31079=CARTESIAN_POINT('Ctrl Pts',(0.05640635123584,0.3769975825921,3.947173799546));
#31080=CARTESIAN_POINT('Ctrl Pts',(0.1006352724421,0.3856118388514,4.037276496891));
#31081=CARTESIAN_POINT('Ctrl Pts',(0.128901400684,0.3903747672857,4.08475381042));
#31082=CARTESIAN_POINT('Ctrl Pts',(0.1341284332036,0.3912344693522,4.093247883936));
#31083=CARTESIAN_POINT('Ctrl Pts',(0.2189431004029,0.1150380520537,3.546425312536));
#31084=CARTESIAN_POINT('Ctrl Pts',(0.2187174988582,0.1155840645799,3.554209879268));
#31085=CARTESIAN_POINT('Ctrl Pts',(0.2181008733428,0.1186055490003,3.596854451109));
#31086=CARTESIAN_POINT('Ctrl Pts',(0.2231215509742,0.1244016054761,3.674400795666));
#31087=CARTESIAN_POINT('Ctrl Pts',(0.2433526981449,0.1327577803046,3.777344386712));
#31088=CARTESIAN_POINT('Ctrl Pts',(0.2768893862856,0.1415339936859,3.877284136683));
#31089=CARTESIAN_POINT('Ctrl Pts',(0.3113049080117,0.1482130428467,3.947661212052));
#31090=CARTESIAN_POINT('Ctrl Pts',(0.333301521837,0.1519035194771,3.984749200474));
#31091=CARTESIAN_POINT('Ctrl Pts',(0.337369261638,0.1525695781223,3.991384739697));
#31092=CARTESIAN_POINT('Ctrl Pts',(0.5469709732897,0.1464668692464,3.553755790656));
#31093=CARTESIAN_POINT('Ctrl Pts',(0.5468380100126,0.14679067791,3.558363759427));
#31094=CARTESIAN_POINT('Ctrl Pts',(0.546474641405,0.1485810122013,3.583608495761));
#31095=CARTESIAN_POINT('Ctrl Pts',(0.5494352161253,0.1519997850887,3.629531909379));
#31096=CARTESIAN_POINT('Ctrl Pts',(0.561372714573,0.1568964726213,3.69052485114));
#31097=CARTESIAN_POINT('Ctrl Pts',(0.5811719886411,0.1620118107838,3.749766788604));
#31098=CARTESIAN_POINT('Ctrl Pts',(0.6014849610443,0.165885532055,3.791477585897));
#31099=CARTESIAN_POINT('Ctrl Pts',(0.6144718382275,0.1680218961319,3.813467076393));
#31100=CARTESIAN_POINT('Ctrl Pts',(0.6168735921791,0.1684073594755,3.817401654546));
#31101=CARTESIAN_POINT('',(0.584439525498375,0.166625640969186,3.82024992016299));
#31102=CARTESIAN_POINT('Origin',(0.5669897777871,0.6648591790704,3.782055102499));
#31103=CARTESIAN_POINT('Origin',(1.02904420412633,0.168033706666644,3.56616160740965));
#31104=CARTESIAN_POINT('Ctrl Pts',(0.1075904147796,0.6897997585045,3.984625378597));
#31105=CARTESIAN_POINT('Ctrl Pts',(0.2296596146426,0.7100892540097,4.196055434799));
#31106=CARTESIAN_POINT('Ctrl Pts',(0.5800094549946,0.7722604608586,4.802879158712));
#31107=CARTESIAN_POINT('Ctrl Pts',(1.173423480477,0.8967762996715,5.830702400772));
#31108=CARTESIAN_POINT('Ctrl Pts',(1.919928591278,1.086197265899,7.123687180788));
#31109=CARTESIAN_POINT('Ctrl Pts',(2.445873995284,1.245360410803,8.034651342534));
#31110=CARTESIAN_POINT('Ctrl Pts',(2.729006765993,1.338703235373,8.52505168669));
#31111=CARTESIAN_POINT('Ctrl Pts',(2.737553647736,1.341527957415,8.539855320115));
#31112=CARTESIAN_POINT('Ctrl Pts',(0.1045498530895,0.3724382569512,4.016835861329));
#31113=CARTESIAN_POINT('Ctrl Pts',(0.2272093052091,0.3928258600432,4.229288264428));
#31114=CARTESIAN_POINT('Ctrl Pts',(0.5792540041567,0.4552978195373,4.839047569541));
#31115=CARTESIAN_POINT('Ctrl Pts',(1.175543046931,0.5804168562544,5.871850487623));
#31116=CARTESIAN_POINT('Ctrl Pts',(1.925673807413,0.7707576941208,7.171115077098));
#31117=CARTESIAN_POINT('Ctrl Pts',(2.454181932341,0.9306962513913,8.086518001686));
#31118=CARTESIAN_POINT('Ctrl Pts',(2.73869719209,1.024494853114,8.5793128871));
#31119=CARTESIAN_POINT('Ctrl Pts',(2.747285809458,1.027333368668,8.594188808748));
#31120=CARTESIAN_POINT('Ctrl Pts',(0.308498647005,0.1467474938082,3.920743969836));
#31121=CARTESIAN_POINT('Ctrl Pts',(0.4315778554011,0.167204865842,4.133923412134));
#31122=CARTESIAN_POINT('Ctrl Pts',(0.7848278483999,0.2298907047566,4.745770347781));
#31123=CARTESIAN_POINT('Ctrl Pts',(1.383161451851,0.3554387040121,5.782114548835));
#31124=CARTESIAN_POINT('Ctrl Pts',(2.135870583181,0.5464337060764,7.085845007618));
#31125=CARTESIAN_POINT('Ctrl Pts',(2.666201180077,0.7069236957289,8.00440454625));
#31126=CARTESIAN_POINT('Ctrl Pts',(2.951699593123,0.8010464221266,8.498902303127));
#31127=CARTESIAN_POINT('Ctrl Pts',(2.960317890666,0.8038947468991,8.513829632345));
#31128=CARTESIAN_POINT('Ctrl Pts',(0.5837390273062,0.1628913043404,3.76028465105));
#31129=CARTESIAN_POINT('Ctrl Pts',(0.7067882102565,0.1833436857553,3.973412087749));
#31130=CARTESIAN_POINT('Ctrl Pts',(1.059951987769,0.2460142257326,4.585109693795));
#31131=CARTESIAN_POINT('Ctrl Pts',(1.658139342435,0.3715315410122,5.62120058452));
#31132=CARTESIAN_POINT('Ctrl Pts',(2.410664041181,0.562479750276,6.924611596699));
#31133=CARTESIAN_POINT('Ctrl Pts',(2.940864275444,0.7229302956031,7.842945340627));
#31134=CARTESIAN_POINT('Ctrl Pts',(3.22629236288,0.817029837147,8.337321289974));
#31135=CARTESIAN_POINT('Ctrl Pts',(3.23490853738,0.8198774602596,8.352244941975));
#31136=CARTESIAN_POINT('',(3.16400873341414,0.811418495172985,8.33346839762618));
#31137=CARTESIAN_POINT('Origin',(-2.23140270727043,50.6145742054134,-1.08622182306733));
#31138=CARTESIAN_POINT('Origin',(3.146558985788,1.304093376118,8.250000032393));
#31139=CARTESIAN_POINT('Ctrl Pts',(2.697976171111,1.328291304826,8.470478725465));
#31140=CARTESIAN_POINT('Ctrl Pts',(2.702496427436,1.32989020433,8.478861959952));
#31141=CARTESIAN_POINT('Ctrl Pts',(2.741672170872,1.343336298271,8.549038004148));
#31142=CARTESIAN_POINT('Ctrl Pts',(2.830553529668,1.36759303881,8.670613831123));
#31143=CARTESIAN_POINT('Ctrl Pts',(2.985965248763,1.397432557112,8.808744119105));
#31144=CARTESIAN_POINT('Ctrl Pts',(3.163320103837,1.421879840356,8.910729967018));
#31145=CARTESIAN_POINT('Ctrl Pts',(3.361331922286,1.440697594273,8.976477330544));
#31146=CARTESIAN_POINT('Ctrl Pts',(3.512953212907,1.449081077376,8.993152567829));
#31147=CARTESIAN_POINT('Ctrl Pts',(3.596210880627,1.45181260013,8.991916516691));
#31148=CARTESIAN_POINT('Ctrl Pts',(3.606094403736,1.452110276979,8.991622099435));
#31149=CARTESIAN_POINT('Ctrl Pts',(2.707229713817,1.02483114282,8.522615032357));
#31150=CARTESIAN_POINT('Ctrl Pts',(2.711757531714,1.026437245798,8.531038853544));
#31151=CARTESIAN_POINT('Ctrl Pts',(2.750998819302,1.039943784245,8.601554659816));
#31152=CARTESIAN_POINT('Ctrl Pts',(2.840029078046,1.064307470111,8.72371926588));
#31153=CARTESIAN_POINT('Ctrl Pts',(2.995702241282,1.094273334906,8.86251873823));
#31154=CARTESIAN_POINT('Ctrl Pts',(3.173356931632,1.118818630411,8.964999159331));
#31155=CARTESIAN_POINT('Ctrl Pts',(3.37170509839,1.13770523227,9.031066488327));
#31156=CARTESIAN_POINT('Ctrl Pts',(3.523584957284,1.146112696876,9.04782465196));
#31157=CARTESIAN_POINT('Ctrl Pts',(3.606984784191,1.148848479805,9.046584219238));
#31158=CARTESIAN_POINT('Ctrl Pts',(3.61688518525,1.149146535858,9.046288572707));
#31159=CARTESIAN_POINT('Ctrl Pts',(2.911986615036,0.8053087593334,8.453506053933));
#31160=CARTESIAN_POINT('Ctrl Pts',(2.915517483284,0.8065606383852,8.46009945291));
#31161=CARTESIAN_POINT('Ctrl Pts',(2.946117152648,0.8170869048461,8.515290469754));
#31162=CARTESIAN_POINT('Ctrl Pts',(3.015515812346,0.8360518603861,8.610867703186));
#31163=CARTESIAN_POINT('Ctrl Pts',(3.136719074313,0.8593273898185,8.719331257004));
#31164=CARTESIAN_POINT('Ctrl Pts',(3.274842213709,0.8783567362483,8.799303634155));
#31165=CARTESIAN_POINT('Ctrl Pts',(3.428844796628,0.8929793997328,8.850790670297));
#31166=CARTESIAN_POINT('Ctrl Pts',(3.546633920865,0.8994873453306,8.863833347941));
#31167=CARTESIAN_POINT('Ctrl Pts',(3.611290879112,0.9016089397426,8.862870550793));
#31168=CARTESIAN_POINT('Ctrl Pts',(3.61896601985,0.9018401752654,8.862640837198));
#31169=CARTESIAN_POINT('Ctrl Pts',(3.182848628904,0.8084535997814,8.306825925367));
#31170=CARTESIAN_POINT('Ctrl Pts',(3.185008068947,0.809213682988,8.310874647509));
#31171=CARTESIAN_POINT('Ctrl Pts',(3.20372011791,0.81560237474,8.344760982929));
#31172=CARTESIAN_POINT('Ctrl Pts',(3.246113072049,0.8270747078833,8.403376857699));
#31173=CARTESIAN_POINT('Ctrl Pts',(3.319898698697,0.8410712468725,8.469670488211));
#31174=CARTESIAN_POINT('Ctrl Pts',(3.403641274247,0.8524565440747,8.518356395924));
#31175=CARTESIAN_POINT('Ctrl Pts',(3.496640992492,0.8611771229168,8.54957704807));
#31176=CARTESIAN_POINT('Ctrl Pts',(3.567534072232,0.8650624697199,8.557453867267));
#31177=CARTESIAN_POINT('Ctrl Pts',(3.606407884075,0.8663395697229,8.556875268173));
#31178=CARTESIAN_POINT('Ctrl Pts',(3.611021902544,0.8664790129072,8.556736982723));
#31179=CARTESIAN_POINT('',(3.579571669199,1.362459037518,9.));
#31180=CARTESIAN_POINT('Ctrl Pts',(2.71354627750015,1.3040933719743,8.50000002131796));
#31181=CARTESIAN_POINT('Ctrl Pts',(2.73240780783335,1.30718564412007,8.53266776695291));
#31182=CARTESIAN_POINT('Ctrl Pts',(2.75295855457772,1.31021121384129,8.56397556110528));
#31183=CARTESIAN_POINT('Ctrl Pts',(2.77500953840381,1.31315034809672,8.59385060141172));
#31184=CARTESIAN_POINT('Ctrl Pts',(2.79564689372688,1.31590106246167,8.62181043426805));
#31185=CARTESIAN_POINT('Ctrl Pts',(2.8175992397998,1.31857622541632,8.64851590702357));
#31186=CARTESIAN_POINT('Ctrl Pts',(2.84075275697417,1.32116110135567,8.67390401044094));
#31187=CARTESIAN_POINT('Ctrl Pts',(2.86139502942833,1.32346562006004,8.69653850453914));
#31188=CARTESIAN_POINT('Ctrl Pts',(2.88300033530865,1.32570076855028,8.71812559348188));
#31189=CARTESIAN_POINT('Ctrl Pts',(2.9053417331799,1.3278487177207,8.73852142578194));
#31190=CARTESIAN_POINT('Ctrl Pts',(2.9276224102888,1.32999082906881,8.75886182509195));
#31191=CARTESIAN_POINT('Ctrl Pts',(2.9506345494046,1.33204612157451,8.77801710890381));
#31192=CARTESIAN_POINT('Ctrl Pts',(2.97412950703109,1.33400408893246,8.79589009824868));
#31193=CARTESIAN_POINT('Ctrl Pts',(2.98173577942302,1.33463796251912,8.80167631108535));
#31194=CARTESIAN_POINT('Ctrl Pts',(2.98939251035384,1.3352616975211,8.80732850506171));
#31195=CARTESIAN_POINT('Ctrl Pts',(2.99709090026803,1.33587512176817,8.81284448333751));
#31196=CARTESIAN_POINT('Ctrl Pts',(3.01817510751269,1.33755515669732,8.82795154214076));
#31197=CARTESIAN_POINT('Ctrl Pts',(3.03956856536244,1.33915243335482,8.84204027731431));
#31198=CARTESIAN_POINT('Ctrl Pts',(3.06130422044454,1.34067812790984,8.85521079188191));
#31199=CARTESIAN_POINT('Ctrl Pts',(3.08331169847731,1.34222290257973,8.8685460149949));
#31200=CARTESIAN_POINT('Ctrl Pts',(3.10567056825425,1.34369438926915,8.88094026547201));
#31201=CARTESIAN_POINT('Ctrl Pts',(3.12844969744608,1.34509853175425,8.89245753558751));
#31202=CARTESIAN_POINT('Ctrl Pts',(3.14220400284712,1.34594636945708,8.89941179837871));
#31203=CARTESIAN_POINT('Ctrl Pts',(3.15611215472,1.34676953926675,8.90604553466176));
#31204=CARTESIAN_POINT('Ctrl Pts',(3.17019402171472,1.34756813901533,8.91236502669045));
#31205=CARTESIAN_POINT('Ctrl Pts',(3.19363757911981,1.34889765157618,8.92288574629397));
#31206=CARTESIAN_POINT('Ctrl Pts',(3.21754745231044,1.3501582134814,8.93253160234711));
#31207=CARTESIAN_POINT('Ctrl Pts',(3.24201675624197,1.35135481993116,8.94130645721643));
#31208=CARTESIAN_POINT('Ctrl Pts',(3.26586440232776,1.35252102585176,8.94985838145439));
#31209=CARTESIAN_POINT('Ctrl Pts',(3.29024397859368,1.35362654202181,8.95758316176405));
#31210=CARTESIAN_POINT('Ctrl Pts',(3.31525278905935,1.35466793937946,8.96443755649156));
#31211=CARTESIAN_POINT('Ctrl Pts',(3.33073613975584,1.35531268497921,8.96868122084033));
#31212=CARTESIAN_POINT('Ctrl Pts',(3.34646086769962,1.35593269322772,8.97259033901732));
#31213=CARTESIAN_POINT('Ctrl Pts',(3.36245086038982,1.35652537029808,8.9761447405435));
#31214=CARTESIAN_POINT('Ctrl Pts',(3.39660962826479,1.35779148210085,8.98373786325591));
#31215=CARTESIAN_POINT('Ctrl Pts',(3.43197070713738,1.35894127328653,8.98970505443759));
#31216=CARTESIAN_POINT('Ctrl Pts',(3.46825922074053,1.35994135206922,8.9937705445444));
#31217=CARTESIAN_POINT('Ctrl Pts',(3.50454773434368,1.36094143085192,8.99783603465122));
#31218=CARTESIAN_POINT('Ctrl Pts',(3.5417633787783,1.36179176414304,8.99999968426863));
#31219=CARTESIAN_POINT('Ctrl Pts',(3.579571669199,1.362459037518,8.99999999999982));
#31220=CARTESIAN_POINT('',(3.597021417327,0.8702239620615,8.586024047651));
#31221=CARTESIAN_POINT('Ctrl Pts',(3.16400873340959,0.811418495170706,8.33346839762921));
#31222=CARTESIAN_POINT('Ctrl Pts',(3.18251475913057,0.81755879068723,8.36584286454173));
#31223=CARTESIAN_POINT('Ctrl Pts',(3.20370582008103,0.823267569144944,8.3949175534773));
#31224=CARTESIAN_POINT('Ctrl Pts',(3.22761204491947,0.828633602007933,8.42130397461794));
#31225=CARTESIAN_POINT('Ctrl Pts',(3.25151827749776,0.833999636608221,8.44769040430141));
#31226=CARTESIAN_POINT('Ctrl Pts',(3.2781396477692,0.839023714446743,8.47138842976006));
#31227=CARTESIAN_POINT('Ctrl Pts',(3.30578098628547,0.843474250546619,8.4914816817855));
#31228=CARTESIAN_POINT('Ctrl Pts',(3.33342232480175,0.847924786646494,8.51157493381093));
#31229=CARTESIAN_POINT('Ctrl Pts',(3.36208365741291,0.851801051595527,8.52806353860089));
#31230=CARTESIAN_POINT('Ctrl Pts',(3.39233262875664,0.855252149752825,8.54175073446735));
#31231=CARTESIAN_POINT('Ctrl Pts',(3.42258160010037,0.858703247910124,8.55543793033381));
#31232=CARTESIAN_POINT('Ctrl Pts',(3.45441819613419,0.861729575415374,8.56632364815803));
#31233=CARTESIAN_POINT('Ctrl Pts',(3.48846097084022,0.864270436217875,8.57396910073167));
#31234=CARTESIAN_POINT('Ctrl Pts',(3.52250374554625,0.866811297020377,8.58161455330531));
#31235=CARTESIAN_POINT('Ctrl Pts',(3.55875270266928,0.868866585502102,8.58601975919096));
#31236=CARTESIAN_POINT('Ctrl Pts',(3.59702141732714,0.870223962057679,8.58602404765169));
#31237=CARTESIAN_POINT('Origin',(3.579571668976,1.362459037517,8.5));
#31238=CARTESIAN_POINT('Origin',(3.579571668976,17.50736,8.));
#31239=CARTESIAN_POINT('',(3.57957168230051,6.23754096186244,9.00000000000025));
#31240=CARTESIAN_POINT('Ctrl Pts',(3.579571669193,6.237540962482,9.));
#31241=CARTESIAN_POINT('Ctrl Pts',(3.53011728241888,6.23841424781783,9.00000000001073));
#31242=CARTESIAN_POINT('Ctrl Pts',(3.48117061949772,6.23960201462633,8.99633236936105));
#31243=CARTESIAN_POINT('Ctrl Pts',(3.43310495241581,6.24107719429828,8.98921559881559));
#31244=CARTESIAN_POINT('Ctrl Pts',(3.41090223035401,6.24175861632436,8.98592818624043));
#31245=CARTESIAN_POINT('Ctrl Pts',(3.3888867000059,6.24250136492367,8.9819046412304));
#31246=CARTESIAN_POINT('Ctrl Pts',(3.36709170786865,6.24330277213392,8.97716542413648));
#31247=CARTESIAN_POINT('Ctrl Pts',(3.33744658181104,6.24439283069516,8.97071923286102));
#31248=CARTESIAN_POINT('Ctrl Pts',(3.30820446262744,6.24559141304431,8.96294344610757));
#31249=CARTESIAN_POINT('Ctrl Pts',(3.27958235305604,6.24688296887885,8.95394256133893));
#31250=CARTESIAN_POINT('Ctrl Pts',(3.25079015911753,6.24818219967028,8.94488818960472));
#31251=CARTESIAN_POINT('Ctrl Pts',(3.22262595615722,6.24957551220371,8.93459447260509));
#31252=CARTESIAN_POINT('Ctrl Pts',(3.19528464198247,6.25104707730712,8.92321367022184));
#31253=CARTESIAN_POINT('Ctrl Pts',(3.18656406822489,6.25151643631237,8.9195837376601));
#31254=CARTESIAN_POINT('Ctrl Pts',(3.1779269748766,6.2519937559938,8.91584353960427));
#31255=CARTESIAN_POINT('Ctrl Pts',(3.16937899398663,6.25247852273933,8.91199888672359));
#31256=CARTESIAN_POINT('Ctrl Pts',(3.14459614848154,6.25388398907288,8.90085222652524));
#31257=CARTESIAN_POINT('Ctrl Pts',(3.12056218077246,6.25535205339036,8.88883262541388));
#31258=CARTESIAN_POINT('Ctrl Pts',(3.09717010751247,6.25688421677726,8.8759501889363));
#31259=CARTESIAN_POINT('Ctrl Pts',(3.07357809068857,6.25842947631876,8.86295763993332));
#31260=CARTESIAN_POINT('Ctrl Pts',(3.05063831677839,6.26003993538532,8.8490870940687));
#31261=CARTESIAN_POINT('Ctrl Pts',(3.02826126562333,6.26171713388391,8.83430020925031));
#31262=CARTESIAN_POINT('Ctrl Pts',(3.01732772911007,6.26253662126396,8.82707526508949));
#31263=CARTESIAN_POINT('Ctrl Pts',(3.00652890218638,6.26337204166456,8.81963085750914));
#31264=CARTESIAN_POINT('Ctrl Pts',(2.99585681279478,6.26422357471117,8.81195872227185));
#31265=CARTESIAN_POINT('Ctrl Pts',(2.97302911160615,6.26604501203492,8.79554795168614));
#31266=CARTESIAN_POINT('Ctrl Pts',(2.95079225545371,6.26794017054501,8.77810692567441));
#31267=CARTESIAN_POINT('Ctrl Pts',(2.92912259389889,6.26991940834275,8.7595498671788));
#31268=CARTESIAN_POINT('Ctrl Pts',(2.90794523902614,6.27185368041776,8.74141440104973));
#31269=CARTESIAN_POINT('Ctrl Pts',(2.88730911650271,6.27386825483174,8.7222124749539));
#31270=CARTESIAN_POINT('Ctrl Pts',(2.8672324480952,6.27597279963524,8.70183533282027));
#31271=CARTESIAN_POINT('Ctrl Pts',(2.85910235513914,6.27682503988423,8.6935835623391));
#31272=CARTESIAN_POINT('Ctrl Pts',(2.85106451293426,6.27769203405006,8.68513878574988));
#31273=CARTESIAN_POINT('Ctrl Pts',(2.84312235741875,6.27857442415559,8.67649272834736));
#31274=CARTESIAN_POINT('Ctrl Pts',(2.82117822934304,6.28101246272719,8.65260372357777));
#31275=CARTESIAN_POINT('Ctrl Pts',(2.79996899724937,6.28356803599439,8.62717678449721));
#31276=CARTESIAN_POINT('Ctrl Pts',(2.77978100812815,6.28622141984332,8.60027901747484));
#31277=CARTESIAN_POINT('Ctrl Pts',(2.75981064432942,6.28884620037211,8.57367120678183));
#31278=CARTESIAN_POINT('Ctrl Pts',(2.74084026265292,6.29156669406441,8.54562420429965));
#31279=CARTESIAN_POINT('Ctrl Pts',(2.72313539509604,6.29436380782913,8.51625275668281));
#31280=CARTESIAN_POINT('Ctrl Pts',(2.71989618577763,6.29487555619111,8.51087907814442));
#31281=CARTESIAN_POINT('Ctrl Pts',(2.716699290052,6.2953898692451,8.50546119925901));
#31282=CARTESIAN_POINT('Ctrl Pts',(2.71354626506509,6.295906630064,8.49999999978095));
#31283=CARTESIAN_POINT('',(3.579571669193,6.237540962482,9.));
#31284=CARTESIAN_POINT('Ctrl Pts',(3.606118543797,6.147888877213,8.991622020187));
#31285=CARTESIAN_POINT('Ctrl Pts',(3.596226611735,6.14818683719,8.991916533163));
#31286=CARTESIAN_POINT('Ctrl Pts',(3.514543691835,6.150866828852,8.9931285392));
#31287=CARTESIAN_POINT('Ctrl Pts',(3.362649869023,6.159198407814,8.976794092479));
#31288=CARTESIAN_POINT('Ctrl Pts',(3.163916181684,6.178009793471,8.911233217637));
#31289=CARTESIAN_POINT('Ctrl Pts',(2.986337602701,6.202539765663,8.808822625203));
#31290=CARTESIAN_POINT('Ctrl Pts',(2.831066145079,6.232302140706,8.671103691814));
#31291=CARTESIAN_POINT('Ctrl Pts',(2.742230088108,6.256472013443,8.550038566438));
#31292=CARTESIAN_POINT('Ctrl Pts',(2.702500721408,6.270108389296,8.478869254392));
#31293=CARTESIAN_POINT('Ctrl Pts',(2.69798283987,6.271706509569,8.47049007187));
#31294=CARTESIAN_POINT('Ctrl Pts',(3.616909366482,6.450852618565,9.046288493852));
#31295=CARTESIAN_POINT('Ctrl Pts',(3.607000542165,6.451150958213,9.046584236403));
#31296=CARTESIAN_POINT('Ctrl Pts',(3.525178152179,6.453835130108,9.047800537919));
#31297=CARTESIAN_POINT('Ctrl Pts',(3.373025288817,6.462190415094,9.031384796543));
#31298=CARTESIAN_POINT('Ctrl Pts',(3.173954011786,6.481070540639,8.965504847357));
#31299=CARTESIAN_POINT('Ctrl Pts',(2.996075229086,6.505698897314,8.862597627541));
#31300=CARTESIAN_POINT('Ctrl Pts',(2.840542553224,6.535587263935,8.724211499603));
#31301=CARTESIAN_POINT('Ctrl Pts',(2.751557670134,6.559863667414,8.602560066809));
#31302=CARTESIAN_POINT('Ctrl Pts',(2.711761832896,6.57356134326,8.531046183576));
#31303=CARTESIAN_POINT('Ctrl Pts',(2.707236393739,6.575166663517,8.522626433943));
#31304=CARTESIAN_POINT('Ctrl Pts',(3.61898478102,6.698159168706,8.862640776355));
#31305=CARTESIAN_POINT('Ctrl Pts',(3.61130310312,6.698390624919,8.862870563926));
#31306=CARTESIAN_POINT('Ctrl Pts',(3.547869039179,6.700472197892,8.863814624792));
#31307=CARTESIAN_POINT('Ctrl Pts',(3.429869177846,6.706939900386,8.851038343534));
#31308=CARTESIAN_POINT('Ctrl Pts',(3.275307153675,6.7215572598,8.799698550945));
#31309=CARTESIAN_POINT('Ctrl Pts',(3.137008498961,6.7406511827,8.719392459593));
#31310=CARTESIAN_POINT('Ctrl Pts',(3.015915940792,6.763866383704,8.611252396668));
#31311=CARTESIAN_POINT('Ctrl Pts',(2.946552922871,6.782763032102,8.516077397137));
#31312=CARTESIAN_POINT('Ctrl Pts',(2.915520842571,6.793438263292,8.460105184664));
#31313=CARTESIAN_POINT('Ctrl Pts',(2.911991831747,6.794689532614,8.453514967436));
#31314=CARTESIAN_POINT('Ctrl Pts',(3.611033207671,6.733520588822,8.556736947109));
#31315=CARTESIAN_POINT('Ctrl Pts',(3.60641524659,6.733660166175,8.55687527608));
#31316=CARTESIAN_POINT('Ctrl Pts',(3.568276611501,6.734913179705,8.557442605468));
#31317=CARTESIAN_POINT('Ctrl Pts',(3.497258450995,6.738774888522,8.54972654454));
#31318=CARTESIAN_POINT('Ctrl Pts',(3.403924438349,6.747491875044,8.51859733675));
#31319=CARTESIAN_POINT('Ctrl Pts',(3.320073171016,6.758916088725,8.469707112214));
#31320=CARTESIAN_POINT('Ctrl Pts',(3.246357276968,6.772876143129,8.403612059442));
#31321=CARTESIAN_POINT('Ctrl Pts',(3.203986574343,6.78430654263,8.345244177306));
#31322=CARTESIAN_POINT('Ctrl Pts',(3.185010131382,6.790785649759,8.310878157544));
#31323=CARTESIAN_POINT('Ctrl Pts',(3.182851831626,6.791545363384,8.306831380263));
#31324=CARTESIAN_POINT('',(3.59702142700201,6.72977603759518,8.58602404765126));
#31325=CARTESIAN_POINT('Origin',(3.57957168907,6.237540961771,8.500000000001));
#31326=CARTESIAN_POINT('',(3.164008715435,6.788581510789,8.333468366184));
#31327=CARTESIAN_POINT('Ctrl Pts',(3.597021417327,6.7297760379381,8.58602404765102));
#31328=CARTESIAN_POINT('Ctrl Pts',(3.58088597603724,6.73034837177699,8.58602214343887));
#31329=CARTESIAN_POINT('Ctrl Pts',(3.56502302749176,6.73104708591087,8.58524234323971));
#31330=CARTESIAN_POINT('Ctrl Pts',(3.54938881284648,6.73186430375203,8.58373710784466));
#31331=CARTESIAN_POINT('Ctrl Pts',(3.53334636737609,6.73270286027384,8.58219256868531));
#31332=CARTESIAN_POINT('Ctrl Pts',(3.5175438291784,6.73366625394346,8.57988406271693));
#31333=CARTESIAN_POINT('Ctrl Pts',(3.50193410093652,6.7347552796972,8.57681507176309));
#31334=CARTESIAN_POINT('Ctrl Pts',(3.49820568216472,6.73501539595293,8.57608203635687));
#31335=CARTESIAN_POINT('Ctrl Pts',(3.49448829989847,6.73528271796873,8.57530538710957));
#31336=CARTESIAN_POINT('Ctrl Pts',(3.49078140477858,6.73555732665343,8.57448474949574));
#31337=CARTESIAN_POINT('Ctrl Pts',(3.47360580500939,6.73682970386104,8.57068239125389));
#31338=CARTESIAN_POINT('Ctrl Pts',(3.45664662919491,6.7382522489223,8.565973303512));
#31339=CARTESIAN_POINT('Ctrl Pts',(3.44010684884663,6.73980100233827,8.56044841819582));
#31340=CARTESIAN_POINT('Ctrl Pts',(3.42356706849835,6.74134975575425,8.55492353287965));
#31341=CARTESIAN_POINT('Ctrl Pts',(3.40744744894976,6.74302460283963,8.54858330475174));
#31342=CARTESIAN_POINT('Ctrl Pts',(3.39192510545283,6.74479444026113,8.54156578324247));
#31343=CARTESIAN_POINT('Ctrl Pts',(3.37807378237151,6.74637375010771,8.5353037160698));
#31344=CARTESIAN_POINT('Ctrl Pts',(3.3647095305328,6.74803262883628,8.52847746681804));
#31345=CARTESIAN_POINT('Ctrl Pts',(3.35174356115493,6.74977086519574,8.5211019478325));
#31346=CARTESIAN_POINT('Ctrl Pts',(3.33862508481612,6.75152954685604,8.51363967729348));
#31347=CARTESIAN_POINT('Ctrl Pts',(3.32591360725994,6.7533695599748,8.50561478592258));
#31348=CARTESIAN_POINT('Ctrl Pts',(3.31353616043678,6.75529834751392,8.49699420783524));
#31349=CARTESIAN_POINT('Ctrl Pts',(3.31072834626721,6.75573589146461,8.49503863641172));
#31350=CARTESIAN_POINT('Ctrl Pts',(3.30793782318856,6.75617803139363,8.49305222690647));
#31351=CARTESIAN_POINT('Ctrl Pts',(3.30516393353998,6.75662490076,8.49103427713288));
#31352=CARTESIAN_POINT('Ctrl Pts',(3.29133031694917,6.75885347516771,8.48097059508209));
#31353=CARTESIAN_POINT('Ctrl Pts',(3.27790939081006,6.76119658123771,8.47014077335627));
#31354=CARTESIAN_POINT('Ctrl Pts',(3.26491581809246,6.76366283998476,8.45848214059525));
#31355=CARTESIAN_POINT('Ctrl Pts',(3.25246674010343,6.7660257503367,8.44731206200011));
#31356=CARTESIAN_POINT('Ctrl Pts',(3.24040961873387,6.76850182512087,8.43538062366922));
#31357=CARTESIAN_POINT('Ctrl Pts',(3.22879686755357,6.77110046653676,8.42261152045667));
#31358=CARTESIAN_POINT('Ctrl Pts',(3.21693015853769,6.77375593732402,8.40956317128735));
#31359=CARTESIAN_POINT('Ctrl Pts',(3.20553108667914,6.77653839520581,8.39564525193401));
#31360=CARTESIAN_POINT('Ctrl Pts',(3.19469271145958,6.7794511503701,8.38080593133939));
#31361=CARTESIAN_POINT('Ctrl Pts',(3.18448743738699,6.78219376299937,8.36683341879471));
#31362=CARTESIAN_POINT('Ctrl Pts',(3.17477900744225,6.78505201880737,8.35204337981397));
#31363=CARTESIAN_POINT('Ctrl Pts',(3.16569253133343,6.78802657658399,8.33639132777214));
#31364=CARTESIAN_POINT('Ctrl Pts',(3.16512883667855,6.78821110822191,8.33542032669666));
#31365=CARTESIAN_POINT('Ctrl Pts',(3.16456755246907,6.7883960863902,8.33444600947876));
#31366=CARTESIAN_POINT('Ctrl Pts',(3.164008715435,6.78858151078889,8.33346836618398));
#31367=CARTESIAN_POINT('Origin',(3.14655896696,6.295906630073,8.249999999787));
#31368=CARTESIAN_POINT('Ctrl Pts',(2.73755431537,6.258471820398,8.539856476492));
#31369=CARTESIAN_POINT('Ctrl Pts',(2.729007207951,6.261296617751,8.525052452183));
#31370=CARTESIAN_POINT('Ctrl Pts',(2.498328684723,6.33734641652,8.125505529738));
#31371=CARTESIAN_POINT('Ctrl Pts',(2.04242243337,6.477595338386,7.335852738906));
#31372=CARTESIAN_POINT('Ctrl Pts',(1.343393624252,6.663026878556,6.12509932556));
#31373=CARTESIAN_POINT('Ctrl Pts',(0.6974672715952,6.805597994089,5.00632206481));
#31374=CARTESIAN_POINT('Ctrl Pts',(0.2768280555865,6.882070724215,4.277753571027));
#31375=CARTESIAN_POINT('Ctrl Pts',(0.107591124226,6.91020011954,3.984626607394));
#31376=CARTESIAN_POINT('Ctrl Pts',(2.747286480821,6.572666423231,8.594189973393));
#31377=CARTESIAN_POINT('Ctrl Pts',(2.738697636674,6.575505014465,8.579313658951));
#31378=CARTESIAN_POINT('Ctrl Pts',(2.506892749498,6.651926151471,8.17781581692));
#31379=CARTESIAN_POINT('Ctrl Pts',(2.048764186804,6.792858642713,7.384313869934));
#31380=CARTESIAN_POINT('Ctrl Pts',(1.346337835851,6.979191351984,6.167675741509));
#31381=CARTESIAN_POINT('Ctrl Pts',(0.6972802940191,7.122453502016,5.043475102021));
#31382=CARTESIAN_POINT('Ctrl Pts',(0.2746058239404,7.199296224689,4.311381444782));
#31383=CARTESIAN_POINT('Ctrl Pts',(0.1045505658565,7.227561636244,4.016837097687));
#31384=CARTESIAN_POINT('Ctrl Pts',(2.960318580227,6.796105048041,8.513830792565));
#31385=CARTESIAN_POINT('Ctrl Pts',(2.951700055121,6.798953448756,8.498903069194));
#31386=CARTESIAN_POINT('Ctrl Pts',(2.719094157332,6.875638661924,8.096017836083));
#31387=CARTESIAN_POINT('Ctrl Pts',(2.259385204058,7.017057271642,7.29977857232));
#31388=CARTESIAN_POINT('Ctrl Pts',(1.554542700605,7.204030844833,6.078955545004));
#31389=CARTESIAN_POINT('Ctrl Pts',(0.9032584222318,7.347784422142,4.950898084692));
#31390=CARTESIAN_POINT('Ctrl Pts',(0.4791365868375,7.424890263994,4.216297517189));
#31391=CARTESIAN_POINT('Ctrl Pts',(0.3084993779623,7.453252403116,3.920745201756));
#31392=CARTESIAN_POINT('Ctrl Pts',(3.234909237514,6.780122314181,8.352246091786));
#31393=CARTESIAN_POINT('Ctrl Pts',(3.226292835509,6.782970013216,8.337322045735));
#31394=CARTESIAN_POINT('Ctrl Pts',(2.993744234615,6.859636336817,7.934536053757));
#31395=CARTESIAN_POINT('Ctrl Pts',(2.534148327875,7.001020174112,7.138492592334));
#31396=CARTESIAN_POINT('Ctrl Pts',(1.829478653638,7.187947905822,5.917968914001));
#31397=CARTESIAN_POINT('Ctrl Pts',(1.178353655414,7.331666330967,4.790187335));
#31398=CARTESIAN_POINT('Ctrl Pts',(0.7543353511557,7.408753351705,4.055766088685));
#31399=CARTESIAN_POINT('Ctrl Pts',(0.5837397696607,7.437108571831,3.760285873989));
#31400=CARTESIAN_POINT('',(0.584436889085312,7.43337480914178,3.82024522397442));
#31401=CARTESIAN_POINT('Origin',(0.5669871034298,6.935141265841,3.782050470377));
#31402=CARTESIAN_POINT('Origin',(-2.20586704229758,-42.6932679752466,-1.0417272484549));
#31403=CARTESIAN_POINT('Ctrl Pts',(0.1488993839097,6.882092998737,4.051886316842));
#31404=CARTESIAN_POINT('Ctrl Pts',(0.1391249419216,6.883695858063,4.036047063007));
#31405=CARTESIAN_POINT('Ctrl Pts',(0.1187380670595,6.887199773797,4.000833626095));
#31406=CARTESIAN_POINT('Ctrl Pts',(0.09068402979308,6.892584054817,3.944687824196));
#31407=CARTESIAN_POINT('Ctrl Pts',(0.06509502960357,6.898211837795,3.883612722829));
#31408=CARTESIAN_POINT('Ctrl Pts',(0.04362719886288,6.903757390935,3.820964525266));
#31409=CARTESIAN_POINT('Ctrl Pts',(0.02637474659593,6.9091924048,3.757016860335));
#31410=CARTESIAN_POINT('Ctrl Pts',(0.0134143459347,6.914489765827,3.692048579365));
#31411=CARTESIAN_POINT('Ctrl Pts',(0.004805063189619,6.919623625663,3.626343926084));
#31412=CARTESIAN_POINT('Ctrl Pts',(0.0007382764448709,6.924391993813,3.562568427967));
#31413=CARTESIAN_POINT('Ctrl Pts',(0.000710719447065,6.927386121703,3.520747207447));
#31414=CARTESIAN_POINT('Ctrl Pts',(0.001283507568449,6.928767604726,3.501041178649));
#31415=CARTESIAN_POINT('Ctrl Pts',(0.1340961482713,7.208770547067,4.09319900537));
#31416=CARTESIAN_POINT('Ctrl Pts',(0.1240204805176,7.210428200377,4.076818539986));
#31417=CARTESIAN_POINT('Ctrl Pts',(0.103007671651,7.214051571443,4.040405692018));
#31418=CARTESIAN_POINT('Ctrl Pts',(0.07408852360614,7.219620173195,3.982340497052));
#31419=CARTESIAN_POINT('Ctrl Pts',(0.04771230919604,7.225440313667,3.919181444569));
#31420=CARTESIAN_POINT('Ctrl Pts',(0.02558314411504,7.231175635589,3.854393383835));
#31421=CARTESIAN_POINT('Ctrl Pts',(0.007799466531112,7.236796549271,3.788262308255));
#31422=CARTESIAN_POINT('Ctrl Pts',(-0.005560285788121,7.24227518205,3.721074180306));
#31423=CARTESIAN_POINT('Ctrl Pts',(-0.01443475371415,7.247584520523,3.653126248775));
#31424=CARTESIAN_POINT('Ctrl Pts',(-0.01862695084338,7.252516147052,3.587168415754));
#31425=CARTESIAN_POINT('Ctrl Pts',(-0.0186554368296,7.255612364638,3.543921256501));
#31426=CARTESIAN_POINT('Ctrl Pts',(-0.01806494151223,7.257041119415,3.523540741356));
#31427=CARTESIAN_POINT('Ctrl Pts',(0.3373468469199,7.447433892025,3.99135077941));
#31428=CARTESIAN_POINT('Ctrl Pts',(0.3295060114974,7.448718119987,3.978555091384));
#31429=CARTESIAN_POINT('Ctrl Pts',(0.3131537888847,7.451525913903,3.950110871236));
#31430=CARTESIAN_POINT('Ctrl Pts',(0.2906487244678,7.455843821799,3.904752830445));
#31431=CARTESIAN_POINT('Ctrl Pts',(0.2701232225468,7.46036004213,3.85541761694));
#31432=CARTESIAN_POINT('Ctrl Pts',(0.2529031715268,7.464814116684,3.804811783341));
#31433=CARTESIAN_POINT('Ctrl Pts',(0.239065347631,7.469183247015,3.753160061754));
#31434=CARTESIAN_POINT('Ctrl Pts',(0.2286704731386,7.473445999966,3.700686137549));
#31435=CARTESIAN_POINT('Ctrl Pts',(0.2217660378869,7.477581471328,3.647623379189));
#31436=CARTESIAN_POINT('Ctrl Pts',(0.2185047232103,7.481427316599,3.596118768688));
#31437=CARTESIAN_POINT('Ctrl Pts',(0.2184826254111,7.483844809718,3.562351628979));
#31438=CARTESIAN_POINT('Ctrl Pts',(0.2189419428023,7.484961027628,3.546439410883));
#31439=CARTESIAN_POINT('Ctrl Pts',(0.6168657783813,7.431593816078,3.817389966263));
#31440=CARTESIAN_POINT('Ctrl Pts',(0.6122368361889,7.432336897234,3.809804338841));
#31441=CARTESIAN_POINT('Ctrl Pts',(0.6025805406548,7.433963020169,3.792937948481));
#31442=CARTESIAN_POINT('Ctrl Pts',(0.5892943522034,7.436467691435,3.766049222514));
#31443=CARTESIAN_POINT('Ctrl Pts',(0.5771760896146,7.439093315939,3.736802263077));
#31444=CARTESIAN_POINT('Ctrl Pts',(0.5670110510533,7.441688912623,3.706807363841));
#31445=CARTESIAN_POINT('Ctrl Pts',(0.5588435708717,7.444241808268,3.676197105016));
#31446=CARTESIAN_POINT('Ctrl Pts',(0.5527095338879,7.446739715699,3.645106950514));
#31447=CARTESIAN_POINT('Ctrl Pts',(0.548636073621,7.449170852428,3.613674065384));
#31448=CARTESIAN_POINT('Ctrl Pts',(0.5467125597304,7.451439307202,3.583175808014));
#31449=CARTESIAN_POINT('Ctrl Pts',(0.5466997109569,7.452870733248,3.563181477118));
#31450=CARTESIAN_POINT('Ctrl Pts',(0.5469704737393,7.453532628332,3.553763299103));
#31451=CARTESIAN_POINT('',(0.517449769067295,7.45443539562573,3.56771964176174));
#31452=CARTESIAN_POINT('Origin',(0.5,6.956014615875,3.532051288651));
#31453=CARTESIAN_POINT('Origin',(1.00128615094072,6.93399420435526,3.53122260992015));
#31454=CARTESIAN_POINT('Origin',(1.02905179608584,7.43196778205744,3.56615971566351));
#31455=CARTESIAN_POINT('Origin',(0.5,-42.4,0.));
#31456=CARTESIAN_POINT('',(0.517453073023311,7.54185093199608,2.00135351550442));
#31457=CARTESIAN_POINT('Origin',(0.5174497483513,-42.4,0.));
#31458=CARTESIAN_POINT('',(0.0865761666724887,7.32353683798742,1.99264208718994));
#31459=CARTESIAN_POINT('Origin',(0.5,7.0425494055,1.981381677743));
#31460=CARTESIAN_POINT('Ctrl Pts',(1.76192394008012E-13,6.99871871675034,
2.87370766691651));
#31461=CARTESIAN_POINT('Ctrl Pts',(1.54231259874596E-8,7.01973080080283,
2.82882528737174));
#31462=CARTESIAN_POINT('Ctrl Pts',(0.00101186006621219,7.03995776878894,
2.78388483535249));
#31463=CARTESIAN_POINT('Ctrl Pts',(0.00280079850515474,7.05927952278183,
2.73936883200046));
#31464=CARTESIAN_POINT('Ctrl Pts',(0.00380243770965784,7.07009790863444,
2.71444400886818));
#31465=CARTESIAN_POINT('Ctrl Pts',(0.00504780239427035,7.08063350065316,
2.68965236124658));
#31466=CARTESIAN_POINT('Ctrl Pts',(0.00649712134266744,7.09087208606895,
2.66507931910599));
#31467=CARTESIAN_POINT('Ctrl Pts',(0.00834719043383405,7.10394173539352,
2.63371160271029));
#31468=CARTESIAN_POINT('Ctrl Pts',(0.0105243960090612,7.11652241623467,
2.60269882830759));
#31469=CARTESIAN_POINT('Ctrl Pts',(0.0130034531449881,7.12880850553544,
2.57159451211062));
#31470=CARTESIAN_POINT('Ctrl Pts',(0.0155308113112305,7.14133397244602,
2.53988417094641));
#31471=CARTESIAN_POINT('Ctrl Pts',(0.0183721278706122,7.15355382103671,
2.50807870852747));
#31472=CARTESIAN_POINT('Ctrl Pts',(0.0215529360858484,7.16566375687849,
2.47570186213225));
#31473=CARTESIAN_POINT('Ctrl Pts',(0.0220616550255212,7.16760054567682,
2.47052370807403));
#31474=CARTESIAN_POINT('Ctrl Pts',(0.0225791610344311,7.16953449172451,
2.4653309317779));
#31475=CARTESIAN_POINT('Ctrl Pts',(0.0231056752009869,7.17146635677458,
2.46012157690981));
#31476=CARTESIAN_POINT('Ctrl Pts',(0.0275243378057489,7.18767913963284,
2.41640313016578));
#31477=CARTESIAN_POINT('Ctrl Pts',(0.0325718997016025,7.20374050194306,
2.37151833744122));
#31478=CARTESIAN_POINT('Ctrl Pts',(0.0383080237529643,7.21973440599729,
2.32497070432694));
#31479=CARTESIAN_POINT('Ctrl Pts',(0.0417209920364785,7.22925070773307,
2.29727506977142));
#31480=CARTESIAN_POINT('Ctrl Pts',(0.0453785461739025,7.23874266445839,
2.2689906890865));
#31481=CARTESIAN_POINT('Ctrl Pts',(0.0493002060250779,7.24822255917105,
2.24001235735313));
#31482=CARTESIAN_POINT('Ctrl Pts',(0.057002047233522,7.26684035023923,2.18310112130363));
#31483=CARTESIAN_POINT('Ctrl Pts',(0.0657293147569602,7.2854118098693,2.12351422610049));
#31484=CARTESIAN_POINT('Ctrl Pts',(0.0754853867527238,7.30367502560143,
2.06149859167507));
#31485=CARTESIAN_POINT('Ctrl Pts',(0.0790459994374604,7.31034043742169,
2.0388651327704));
#31486=CARTESIAN_POINT('Ctrl Pts',(0.0827431515438966,7.31696481318815,
2.01590821646725));
#31487=CARTESIAN_POINT('Ctrl Pts',(0.0865752842352255,7.32353562251123,
1.99264001890475));
#31488=CARTESIAN_POINT('Ctrl Pts',(-0.001081260139012,7.014309618948,2.906543661707));
#31489=CARTESIAN_POINT('Ctrl Pts',(-0.001018369255986,7.016400799091,2.902147314851));
#31490=CARTESIAN_POINT('Ctrl Pts',(0.0001871679450522,7.050992423812,2.829131820991));
#31491=CARTESIAN_POINT('Ctrl Pts',(0.007507857493721,7.113697217666,2.687558940315));
#31492=CARTESIAN_POINT('Ctrl Pts',(0.02870561913676,7.197032885506,2.474508650036));
#31493=CARTESIAN_POINT('Ctrl Pts',(0.05928519434814,7.274597632677,2.249119982873));
#31494=CARTESIAN_POINT('Ctrl Pts',(0.08618036230883,7.322967042458,2.086634502438));
#31495=CARTESIAN_POINT('Ctrl Pts',(0.1018793569146,7.347090408829,1.998560749934));
#31496=CARTESIAN_POINT('Ctrl Pts',(0.1027383636877,7.348399198641,1.993759888543));
#31497=CARTESIAN_POINT('Ctrl Pts',(0.02046330720855,6.777047057716,2.691466056719));
#31498=CARTESIAN_POINT('Ctrl Pts',(0.01962993973341,6.778769180525,2.687387423694));
#31499=CARTESIAN_POINT('Ctrl Pts',(0.005955867276291,6.807367774017,2.619615027721));
#31500=CARTESIAN_POINT('Ctrl Pts',(-0.01530270840099,6.862722393628,2.487237441822));
#31501=CARTESIAN_POINT('Ctrl Pts',(-0.03473413003973,6.944167200619,2.285821170463));
#31502=CARTESIAN_POINT('Ctrl Pts',(-0.04384970159776,7.027302511007,2.070790001253));
#31503=CARTESIAN_POINT('Ctrl Pts',(-0.0427213547525,7.084289791949,1.914480858456));
#31504=CARTESIAN_POINT('Ctrl Pts',(-0.04008670908316,7.114174883662,1.829403670676));
#31505=CARTESIAN_POINT('Ctrl Pts',(-0.03993718883914,7.115800914289,1.824765062074));
#31506=CARTESIAN_POINT('Ctrl Pts',(-0.2045700640878,6.606399527962,2.53896888117));
#31507=CARTESIAN_POINT('Ctrl Pts',(-0.2060475584221,6.608724880767,2.535166077691));
#31508=CARTESIAN_POINT('Ctrl Pts',(-0.2303376413689,6.647382899417,2.471943726365));
#31509=CARTESIAN_POINT('Ctrl Pts',(-0.2695762730753,6.723518668901,2.347474954217));
#31510=CARTESIAN_POINT('Ctrl Pts',(-0.3093746426751,6.838297728139,2.155847204795));
#31511=CARTESIAN_POINT('Ctrl Pts',(-0.3336343557535,6.95779484596,1.949271087601));
#31512=CARTESIAN_POINT('Ctrl Pts',(-0.3389528302416,7.041205966119,1.797815533392));
#31513=CARTESIAN_POINT('Ctrl Pts',(-0.3385904718372,7.085346251581,1.715024763658));
#31514=CARTESIAN_POINT('Ctrl Pts',(-0.3385612404185,7.087749102285,1.710509733302));
#31515=CARTESIAN_POINT('Ctrl Pts',(-0.5251165549145,6.61692265344,2.551423432733));
#31516=CARTESIAN_POINT('Ctrl Pts',(-0.526553642486,6.620418575498,2.547669410243));
#31517=CARTESIAN_POINT('Ctrl Pts',(-0.5500696128295,6.678435587297,2.485249607032));
#31518=CARTESIAN_POINT('Ctrl Pts',(-0.5846190863906,6.789533452527,2.362093983857));
#31519=CARTESIAN_POINT('Ctrl Pts',(-0.6108498439799,6.950494605875,2.171838228225));
#31520=CARTESIAN_POINT('Ctrl Pts',(-0.6155364367152,7.112735107433,1.966138843811));
#31521=CARTESIAN_POINT('Ctrl Pts',(-0.6036539839724,7.222637721349,1.814955916913));
#31522=CARTESIAN_POINT('Ctrl Pts',(-0.5932464655588,7.279957162664,1.732206546957));
#31523=CARTESIAN_POINT('Ctrl Pts',(-0.5926675754179,7.283074933677,1.727693462271));
#31524=CARTESIAN_POINT('Origin',(-0.3268616990873,7.604510051501,2.00392196632));
#31525=CARTESIAN_POINT('Origin',(-0.4999999999811,6.998719488534,2.873707297836));
#31526=CARTESIAN_POINT('Origin',(-0.5,3.8,0.));
#31527=CARTESIAN_POINT('',(-0.0201845395642384,5.74664288092434,3.67572020421874));
#31528=CARTESIAN_POINT('Ctrl Pts',(1.00945995400332E-15,6.252471626846,
3.532050807569));
#31529=CARTESIAN_POINT('Ctrl Pts',(1.06255127647422E-8,6.22355721500666,
3.54358362457381));
#31530=CARTESIAN_POINT('Ctrl Pts',(-0.000148869025013445,6.19495270787919,
3.5545016156147));
#31531=CARTESIAN_POINT('Ctrl Pts',(-0.000440295003910586,6.16703450720138,
3.56471173966722));
#31532=CARTESIAN_POINT('Ctrl Pts',(-0.000483686983627105,6.16287761630882,
3.56623197989243));
#31533=CARTESIAN_POINT('Ctrl Pts',(-0.000530204467916582,6.15873593010086,
3.56773661403369));
#31534=CARTESIAN_POINT('Ctrl Pts',(-0.000579789846082578,6.15461067703008,
3.56922542745825));
#31535=CARTESIAN_POINT('Ctrl Pts',(-0.000834392425583689,6.1334290280892,
3.57686993380889));
#31536=CARTESIAN_POINT('Ctrl Pts',(-0.00116909302387783,6.11268021448515,
3.58408901216498));
#31537=CARTESIAN_POINT('Ctrl Pts',(-0.0015949163214279,6.09188868636396,
3.59105101267837));
#31538=CARTESIAN_POINT('Ctrl Pts',(-0.00180900395429268,6.08143550293149,
3.59455123969387));
#31539=CARTESIAN_POINT('Ctrl Pts',(-0.00204636565207327,6.07097134948497,
3.59798577949579));
#31540=CARTESIAN_POINT('Ctrl Pts',(-0.002310032817556,6.06043519420868,
3.60137127125052));
#31541=CARTESIAN_POINT('Ctrl Pts',(-0.00286123018430172,6.03840931535766,
3.6084486566236));
#31542=CARTESIAN_POINT('Ctrl Pts',(-0.00352621841082366,6.01607131827214,
3.61531684209279));
#31543=CARTESIAN_POINT('Ctrl Pts',(-0.00434184921916814,5.99321851908052,
3.62196888132449));
#31544=CARTESIAN_POINT('Ctrl Pts',(-0.00469241156114277,5.98339626773429,
3.6248279622078));
#31545=CARTESIAN_POINT('Ctrl Pts',(-0.0050709858485351,5.97347906253195,
3.62764657225949));
#31546=CARTESIAN_POINT('Ctrl Pts',(-0.00548143949275076,5.96345175192577,
3.63042137614233));
#31547=CARTESIAN_POINT('Ctrl Pts',(-0.00627128196887642,5.94415603863468,
3.63576097538934));
#31548=CARTESIAN_POINT('Ctrl Pts',(-0.00717855499112012,5.92445507963207,
3.64093636106214));
#31549=CARTESIAN_POINT('Ctrl Pts',(-0.00824695910249482,5.9042812924823,
3.6458748404254));
#31550=CARTESIAN_POINT('Ctrl Pts',(-0.00902554440236525,5.88957991315374,
3.64947369164192));
#31551=CARTESIAN_POINT('Ctrl Pts',(-0.00988991053435746,5.874627728668,
3.65294614153715));
#31552=CARTESIAN_POINT('Ctrl Pts',(-0.0108620715118211,5.85940771717124,
3.6562497499432));
#31553=CARTESIAN_POINT('Ctrl Pts',(-0.0108621699993018,5.8594061752655,
3.65625008462447));
#31554=CARTESIAN_POINT('Ctrl Pts',(-0.010862268487912,5.85940463335719,
3.6562504193038));
#31555=CARTESIAN_POINT('Ctrl Pts',(-0.0108623669776518,5.85940309144632,
3.65625075398118));
#31556=CARTESIAN_POINT('Ctrl Pts',(-0.0118020552639595,5.84469175611481,
3.65944390298656));
#31557=CARTESIAN_POINT('Ctrl Pts',(-0.012843753824908,5.82974410458742,
3.66246313874807));
#31558=CARTESIAN_POINT('Ctrl Pts',(-0.0140227868938516,5.81454018579014,
3.66525725177376));
#31559=CARTESIAN_POINT('Ctrl Pts',(-0.0150765914048981,5.8009511197697,
3.66775459386569));
#31560=CARTESIAN_POINT('Ctrl Pts',(-0.0162400356832888,5.78715707091662,
3.67007226537261));
#31561=CARTESIAN_POINT('Ctrl Pts',(-0.0175467950230611,5.7731696367615,
3.67214302747442));
#31562=CARTESIAN_POINT('Ctrl Pts',(-0.0183660613490072,5.76440028387387,
3.67344128156561));
#31563=CARTESIAN_POINT('Ctrl Pts',(-0.0192418228542866,5.75555543595967,
3.67464188759342));
#31564=CARTESIAN_POINT('Ctrl Pts',(-0.0201846418813895,5.74664479462204,
3.67572037342067));
#31565=CARTESIAN_POINT('Ctrl Pts',(-0.0201846820169889,5.74664441529799,
3.67572041933158));
#31566=CARTESIAN_POINT('Ctrl Pts',(-0.0201847221527103,5.74664403597382,
3.67572046524226));
#31567=CARTESIAN_POINT('Ctrl Pts',(-0.0201847622885535,5.74664365664953,
3.67572051115272));
#31568=CARTESIAN_POINT('Origin',(-0.5,3.8,0.));
#31569=CARTESIAN_POINT('Origin',(-0.5,5.812461179705,3.800000000024));
#31570=CARTESIAN_POINT('Ctrl Pts',(0.1458532199875,6.271988053784,4.052080103981));
#31571=CARTESIAN_POINT('Ctrl Pts',(0.1469209552276,6.265500255559,4.053835336582));
#31572=CARTESIAN_POINT('Ctrl Pts',(0.1548191992219,6.217130452916,4.066727704464));
#31573=CARTESIAN_POINT('Ctrl Pts',(0.1686877140563,6.126928446731,4.08805599936));
#31574=CARTESIAN_POINT('Ctrl Pts',(0.1862467344624,5.996365514295,4.111423817831));
#31575=CARTESIAN_POINT('Ctrl Pts',(0.2017409989679,5.856602279246,4.127313273259));
#31576=CARTESIAN_POINT('Ctrl Pts',(0.214005833747,5.696109622742,4.13198287192));
#31577=CARTESIAN_POINT('Ctrl Pts',(0.2165291553049,5.564635500454,4.119507848871));
#31578=CARTESIAN_POINT('Ctrl Pts',(0.2121000073809,5.485266618107,4.101280410414));
#31579=CARTESIAN_POINT('Ctrl Pts',(0.2114977825543,5.476027053408,4.099020181562));
#31580=CARTESIAN_POINT('Ctrl Pts',(0.04343936334695,6.270350607014,3.883896132752));
#31581=CARTESIAN_POINT('Ctrl Pts',(0.04416828941248,6.264404627156,3.88585256665));
#31582=CARTESIAN_POINT('Ctrl Pts',(0.04955358456158,6.220092655311,3.900265951108));
#31583=CARTESIAN_POINT('Ctrl Pts',(0.05891618512559,6.137723881081,3.924730474888));
#31584=CARTESIAN_POINT('Ctrl Pts',(0.07051173903919,6.01940133794,3.953533205108));
#31585=CARTESIAN_POINT('Ctrl Pts',(0.08040336843717,5.894063634032,3.976422191027));
#31586=CARTESIAN_POINT('Ctrl Pts',(0.08764358238867,5.752421718795,3.991109125861));
#31587=CARTESIAN_POINT('Ctrl Pts',(0.08809976070129,5.639482864577,3.989538930058));
#31588=CARTESIAN_POINT('Ctrl Pts',(0.08415878673266,5.573169980138,3.980095150633));
#31589=CARTESIAN_POINT('Ctrl Pts',(0.08363892228445,5.565474898,3.978885877421));
#31590=CARTESIAN_POINT('Ctrl Pts',(-0.006377890669527,6.268771084875,3.693389188242));
#31591=CARTESIAN_POINT('Ctrl Pts',(-0.00603236671339,6.263346825442,3.695441735005));
#31592=CARTESIAN_POINT('Ctrl Pts',(-0.003495091272066,6.222949053301,3.710593058645));
#31593=CARTESIAN_POINT('Ctrl Pts',(0.0007007410215009,6.148232643904,3.736740844206));
#31594=CARTESIAN_POINT('Ctrl Pts',(0.005295480516823,6.042135280344,3.768916440852));
#31595=CARTESIAN_POINT('Ctrl Pts',(0.008404965977148,5.931514095113,3.796677725173));
#31596=CARTESIAN_POINT('Ctrl Pts',(0.009229009165082,5.809512435811,3.819120678812));
#31597=CARTESIAN_POINT('Ctrl Pts',(0.006530259998911,5.716291958244,3.826913774935));
#31598=CARTESIAN_POINT('Ctrl Pts',(0.002550540157001,5.664026167199,3.825603599923));
#31599=CARTESIAN_POINT('Ctrl Pts',(0.002053792328862,5.657994551734,3.825373242286));
#31600=CARTESIAN_POINT('Ctrl Pts',(0.0005956750778858,6.267382470588,3.496598442174));
#31601=CARTESIAN_POINT('Ctrl Pts',(0.000545483402435,6.262415908922,3.498633921431));
#31602=CARTESIAN_POINT('Ctrl Pts',(0.0001394489138727,6.225459160862,3.513677978239));
#31603=CARTESIAN_POINT('Ctrl Pts',(-0.001057340209199,6.157569980829,3.539914341205));
#31604=CARTESIAN_POINT('Ctrl Pts',(-0.003911350084333,6.062653324111,3.573116790386));
#31605=CARTESIAN_POINT('Ctrl Pts',(-0.008192514736,5.965800631096,3.603212932189));
#31606=CARTESIAN_POINT('Ctrl Pts',(-0.0146360016265,5.862575188833,3.630497592084));
#31607=CARTESIAN_POINT('Ctrl Pts',(-0.0213118426677,5.788596065785,3.645324129995));
#31608=CARTESIAN_POINT('Ctrl Pts',(-0.02585396611666,5.750185809919,3.650812719882));
#31609=CARTESIAN_POINT('Ctrl Pts',(-0.02638878731888,5.745796594557,3.651406820841));
#31610=CARTESIAN_POINT('Origin',(1.,6.252471673428,3.532050807569));
#31611=CARTESIAN_POINT('Origin',(0.9394500501458,5.615008433104,3.427175219049));
#31612=CARTESIAN_POINT('Ctrl Pts',(0.09069279366311,5.616670622145,3.956220996979));
#31613=CARTESIAN_POINT('Ctrl Pts',(0.08945616748986,5.611892456011,3.954079097617));
#31614=CARTESIAN_POINT('Ctrl Pts',(0.08238462062046,5.583998454902,3.941830819151));
#31615=CARTESIAN_POINT('Ctrl Pts',(0.06901185007231,5.525746410592,3.918668501123));
#31616=CARTESIAN_POINT('Ctrl Pts',(0.0509683933199,5.437857521209,3.887416317284));
#31617=CARTESIAN_POINT('Ctrl Pts',(0.03265833413454,5.340814192582,3.855702364485));
#31618=CARTESIAN_POINT('Ctrl Pts',(0.0195624461478,5.266338417057,3.833019621122));
#31619=CARTESIAN_POINT('Ctrl Pts',(0.01244523448206,5.224602654389,3.820692248908));
#31620=CARTESIAN_POINT('Ctrl Pts',(0.01153465633603,5.219243031459,3.819115081295));
#31621=CARTESIAN_POINT('Ctrl Pts',(0.03425063267428,5.671857593246,3.865525883381));
#31622=CARTESIAN_POINT('Ctrl Pts',(0.03286492200821,5.666497275129,3.863125762102));
#31623=CARTESIAN_POINT('Ctrl Pts',(0.02500759929367,5.635488104076,3.849516479949));
#31624=CARTESIAN_POINT('Ctrl Pts',(0.01074391216856,5.57326828928,3.82481104915));
#31625=CARTESIAN_POINT('Ctrl Pts',(-0.008050805571124,5.481693915529,3.792257643109));
#31626=CARTESIAN_POINT('Ctrl Pts',(-0.02689492653263,5.381798763955,3.759618668181));
#31627=CARTESIAN_POINT('Ctrl Pts',(-0.04025534178605,5.305812877369,3.73647775015));
#31628=CARTESIAN_POINT('Ctrl Pts',(-0.04749710773029,5.263345244532,3.723934643602));
#31629=CARTESIAN_POINT('Ctrl Pts',(-0.04842335115087,5.257893246949,3.722330342938));
#31630=CARTESIAN_POINT('Ctrl Pts',(-0.002995698117571,5.726448488071,3.765079625067));
#31631=CARTESIAN_POINT('Ctrl Pts',(-0.004528883010469,5.720512305815,3.762424070936));
#31632=CARTESIAN_POINT('Ctrl Pts',(-0.01316349438033,5.68642161187,3.747468485341));
#31633=CARTESIAN_POINT('Ctrl Pts',(-0.02830847524902,5.620276882606,3.721236608974));
#31634=CARTESIAN_POINT('Ctrl Pts',(-0.04784633958708,5.525056831524,3.687396035277));
#31635=CARTESIAN_POINT('Ctrl Pts',(-0.06721875390343,5.422340659634,3.653842029412));
#31636=CARTESIAN_POINT('Ctrl Pts',(-0.08084083925938,5.344860972747,3.630247885476));
#31637=CARTESIAN_POINT('Ctrl Pts',(-0.08820581416463,5.301669374694,3.617491374745));
#31638=CARTESIAN_POINT('Ctrl Pts',(-0.08914755365818,5.2961260002,3.615860234094));
#31639=CARTESIAN_POINT('Ctrl Pts',(-0.01985090485308,5.778691398179,3.65810570186));
#31640=CARTESIAN_POINT('Ctrl Pts',(-0.02152522102488,5.772204120019,3.655205701185));
#31641=CARTESIAN_POINT('Ctrl Pts',(-0.03090368943386,5.735164441195,3.638961717408));
#31642=CARTESIAN_POINT('Ctrl Pts',(-0.04689205909801,5.665263610215,3.611269048736));
#31643=CARTESIAN_POINT('Ctrl Pts',(-0.06714110689197,5.566554684409,3.576196669184));
#31644=CARTESIAN_POINT('Ctrl Pts',(-0.08701909236977,5.461138825856,3.541766988369));
#31645=CARTESIAN_POINT('Ctrl Pts',(-0.1008915932553,5.382229587848,3.517739112028));
#31646=CARTESIAN_POINT('Ctrl Pts',(-0.108374477833,5.338345162724,3.504778375744));
#31647=CARTESIAN_POINT('Ctrl Pts',(-0.1093310469044,5.33271434149,3.50312154951));
#31648=CARTESIAN_POINT('Ctrl Pts',(-0.0201840365334425,5.74664296949069,
3.67572052170447));
#31649=CARTESIAN_POINT('Ctrl Pts',(-0.0210927252446989,5.7269006225596,
3.68266762453094));
#31650=CARTESIAN_POINT('Ctrl Pts',(-0.0217041190570385,5.70714963688255,
3.68923829806003));
#31651=CARTESIAN_POINT('Ctrl Pts',(-0.0220696690856361,5.68759667513464,
3.69543690080271));
#31652=CARTESIAN_POINT('Ctrl Pts',(-0.0224351127454171,5.66804940296473,
3.70163369985783));
#31653=CARTESIAN_POINT('Ctrl Pts',(-0.0225555467297995,5.64870011852324,
3.70745776399795));
#31654=CARTESIAN_POINT('Ctrl Pts',(-0.0224800830796922,5.62980882412369,
3.71292583377142));
#31655=CARTESIAN_POINT('Ctrl Pts',(-0.0224679836683386,5.62677990170056,
3.71380255289918));
#31656=CARTESIAN_POINT('Ctrl Pts',(-0.0224508333255254,5.62376285473207,
3.71467015812384));
#31657=CARTESIAN_POINT('Ctrl Pts',(-0.0224288160121262,5.62075886263511,
3.71552876206813));
#31658=CARTESIAN_POINT('Ctrl Pts',(-0.0224288112348433,5.6207582108335,
3.7155289483667));
#31659=CARTESIAN_POINT('Ctrl Pts',(-0.0224288064573312,5.62075755903251,
3.71552913466485));
#31660=CARTESIAN_POINT('Ctrl Pts',(-0.02242880167959,5.62075690723214,3.71552932096257));
#31661=CARTESIAN_POINT('Ctrl Pts',(-0.0223037157913754,5.60369214283302,
3.72040677554117));
#31662=CARTESIAN_POINT('Ctrl Pts',(-0.0220235154826046,5.58704134367518,
3.72499898065695));
#31663=CARTESIAN_POINT('Ctrl Pts',(-0.0216232495575363,5.57048317754424,
3.72940007283941));
#31664=CARTESIAN_POINT('Ctrl Pts',(-0.021196012066042,5.55280925398874,
3.73409772873791));
#31665=CARTESIAN_POINT('Ctrl Pts',(-0.0206318069207095,5.53524104924983,
3.73857826340128));
#31666=CARTESIAN_POINT('Ctrl Pts',(-0.0199233159681402,5.51741218968596,
3.74297341795032));
#31667=CARTESIAN_POINT('Ctrl Pts',(-0.0197209598352948,5.5123199876454,
3.74422874305303));
#31668=CARTESIAN_POINT('Ctrl Pts',(-0.0195065456981628,5.50720666188784,
3.74547717429369));
#31669=CARTESIAN_POINT('Ctrl Pts',(-0.019279233338892,5.50206401593398,
3.74672192155617));
#31670=CARTESIAN_POINT('Ctrl Pts',(-0.0192792117831918,5.50206352826435,
3.74672203959374));
#31671=CARTESIAN_POINT('Ctrl Pts',(-0.0192791902273797,5.50206304059445,
3.74672215763127));
#31672=CARTESIAN_POINT('Ctrl Pts',(-0.0192791686714558,5.50206255292428,
3.74672227566876));
#31673=CARTESIAN_POINT('Ctrl Pts',(-0.017975161601807,5.47256136556275,
3.7538628518065));
#31674=CARTESIAN_POINT('Ctrl Pts',(-0.0162581453164372,5.44206985804176,
3.76084820516659));
#31675=CARTESIAN_POINT('Ctrl Pts',(-0.0141475466666794,5.41086175160518,
3.76759619439652));
#31676=CARTESIAN_POINT('Ctrl Pts',(-0.0133952540300333,5.39973806938421,
3.77000141843588));
#31677=CARTESIAN_POINT('Ctrl Pts',(-0.0125933460890804,5.38852361999037,
3.77237640057866));
#31678=CARTESIAN_POINT('Ctrl Pts',(-0.0117438815315688,5.37723190413217,
3.77471733200074));
#31679=CARTESIAN_POINT('Ctrl Pts',(-0.00936709712271081,5.34563791476123,
3.78126721010574));
#31680=CARTESIAN_POINT('Ctrl Pts',(-0.00661723154578303,5.31343729109814,
3.78755503811181));
#31681=CARTESIAN_POINT('Ctrl Pts',(-0.00350446402653477,5.28057655596057,
3.79358521521042));
#31682=CARTESIAN_POINT('Ctrl Pts',(-0.00238348478125948,5.26874264872339,
3.79575682080932));
#31683=CARTESIAN_POINT('Ctrl Pts',(-0.00121532087410187,5.25682357467516,
3.79789500125968));
#31684=CARTESIAN_POINT('Ctrl Pts',(-1.96584511304227E-8,5.24481852186864,
3.79999996595058));
#31685=CARTESIAN_POINT('Ctrl Pts',(0.01313183742357,5.24106019073,3.823805869142));
#31686=CARTESIAN_POINT('Ctrl Pts',(0.01303186504026,5.246042423464,3.82385436109));
#31687=CARTESIAN_POINT('Ctrl Pts',(0.01123027883061,5.335368565326,3.82471367541));
#31688=CARTESIAN_POINT('Ctrl Pts',(0.007608839441613,5.499707692812,3.825952350517));
#31689=CARTESIAN_POINT('Ctrl Pts',(0.002704317645799,5.694405545869,3.826393794893));
#31690=CARTESIAN_POINT('Ctrl Pts',(-0.0002703855975803,5.80461369123,3.826069286647));
#31691=CARTESIAN_POINT('Ctrl Pts',(-0.001263515685967,5.840827121397,3.825885856397));
#31692=CARTESIAN_POINT('Ctrl Pts',(-0.1220155422729,5.119490788538,3.559282264932));
#31693=CARTESIAN_POINT('Ctrl Pts',(-0.1210052566975,5.124318427941,3.558834796486));
#31694=CARTESIAN_POINT('Ctrl Pts',(-0.1028036746347,5.210842870579,3.550915651627));
#31695=CARTESIAN_POINT('Ctrl Pts',(-0.06637047516781,5.369103572629,3.539852558725));
#31696=CARTESIAN_POINT('Ctrl Pts',(-0.01740572866676,5.553685032541,3.537170858724));
#31697=CARTESIAN_POINT('Ctrl Pts',(0.0121187820176,5.65630378412,3.541453508646));
#31698=CARTESIAN_POINT('Ctrl Pts',(0.02195442675914,5.689769064298,3.543633877626));
#31699=CARTESIAN_POINT('Ctrl Pts',(-0.4243708118278,5.033379764573,3.494607553578));
#31700=CARTESIAN_POINT('Ctrl Pts',(-0.4230739478696,5.038097901175,3.492966852937));
#31701=CARTESIAN_POINT('Ctrl Pts',(-0.3995937923544,5.122637821518,3.463646745943));
#31702=CARTESIAN_POINT('Ctrl Pts',(-0.3487237350521,5.276593004014,3.413015804354));
#31703=CARTESIAN_POINT('Ctrl Pts',(-0.2708767291411,5.454008738366,3.365007313026));
#31704=CARTESIAN_POINT('Ctrl Pts',(-0.2195329377535,5.551251709049,3.345376679572));
#31705=CARTESIAN_POINT('Ctrl Pts',(-0.2018836868802,5.582770397361,3.339993364003));
#31706=CARTESIAN_POINT('Ctrl Pts',(-0.690961983047,5.040533704331,3.673198060413));
#31707=CARTESIAN_POINT('Ctrl Pts',(-0.6903946011995,5.045260938217,3.670467876084));
#31708=CARTESIAN_POINT('Ctrl Pts',(-0.6799039890485,5.12996572889,3.621490833281));
#31709=CARTESIAN_POINT('Ctrl Pts',(-0.649906360366,5.284278605745,3.530587976371));
#31710=CARTESIAN_POINT('Ctrl Pts',(-0.587552850239,5.46228965492,3.42547705607));
#31711=CARTESIAN_POINT('Ctrl Pts',(-0.5397170591493,5.559979235235,3.369465755669));
#31712=CARTESIAN_POINT('Ctrl Pts',(-0.5225146677869,5.591659642689,3.351668795617));
#31713=CARTESIAN_POINT('Origin',(-0.4330128001874,5.244818804908,4.049999829751));
#31714=CARTESIAN_POINT('Ctrl Pts',(0.1654598431239,3.783166653544,4.090816155837));
#31715=CARTESIAN_POINT('Ctrl Pts',(0.1654730736086,3.788777525565,4.090839257161));
#31716=CARTESIAN_POINT('Ctrl Pts',(0.1656678333893,3.954021206316,4.091179620988));
#31717=CARTESIAN_POINT('Ctrl Pts',(0.1547815560753,4.279983877015,4.072101699741));
#31718=CARTESIAN_POINT('Ctrl Pts',(0.1051279211205,4.770778970143,3.985157894746));
#31719=CARTESIAN_POINT('Ctrl Pts',(0.04760955067503,5.097085532837,3.884627779379));
#31720=CARTESIAN_POINT('Ctrl Pts',(0.01060629140589,5.266200668492,3.820069159091));
#31721=CARTESIAN_POINT('Ctrl Pts',(0.009485886370904,5.271290271532,3.818114554136));
#31722=CARTESIAN_POINT('Ctrl Pts',(0.07652291896167,3.784112020329,3.897696692716));
#31723=CARTESIAN_POINT('Ctrl Pts',(0.07653599330915,3.789407784645,3.897718314989));
#31724=CARTESIAN_POINT('Ctrl Pts',(0.0767284685246,3.945371305455,3.898036864973));
#31725=CARTESIAN_POINT('Ctrl Pts',(0.06596551784964,4.253028048728,3.880183155471));
#31726=CARTESIAN_POINT('Ctrl Pts',(0.0168611100287,4.716461525162,3.798792241893));
#31727=CARTESIAN_POINT('Ctrl Pts',(-0.04005056496638,5.02485756519,3.704621421695));
#31728=CARTESIAN_POINT('Ctrl Pts',(-0.07668074739283,5.184805550002,3.644109787065));
#31729=CARTESIAN_POINT('Ctrl Pts',(-0.07778986614245,5.189619370843,3.642277679814));
#31730=CARTESIAN_POINT('Ctrl Pts',(-0.1058150099763,3.784941987692,3.788344136719));
#31731=CARTESIAN_POINT('Ctrl Pts',(-0.1058022557404,3.789961110452,3.788364161886));
#31732=CARTESIAN_POINT('Ctrl Pts',(-0.1056144643264,3.937777260311,3.788659124856));
#31733=CARTESIAN_POINT('Ctrl Pts',(-0.1161245714929,4.22936306796,3.772131316596));
#31734=CARTESIAN_POINT('Ctrl Pts',(-0.1641029572589,4.669106290867,3.69671684643));
#31735=CARTESIAN_POINT('Ctrl Pts',(-0.2197707890137,4.962460172974,3.60930175649));
#31736=CARTESIAN_POINT('Ctrl Pts',(-0.2556360916169,5.114903105384,3.553035639076));
#31737=CARTESIAN_POINT('Ctrl Pts',(-0.2567220712945,5.119491329578,3.551331993798));
#31738=CARTESIAN_POINT('Ctrl Pts',(-0.3180638821296,3.785367561021,3.800835044669));
#31739=CARTESIAN_POINT('Ctrl Pts',(-0.3180515005168,3.790244834956,3.800853910787));
#31740=CARTESIAN_POINT('Ctrl Pts',(-0.3178691612411,3.933883317182,3.801131726569));
#31741=CARTESIAN_POINT('Ctrl Pts',(-0.3280849481318,4.217229080328,3.785569830272));
#31742=CARTESIAN_POINT('Ctrl Pts',(-0.3747525977687,4.645202358463,3.714474358092));
#31743=CARTESIAN_POINT('Ctrl Pts',(-0.4289725446736,4.931620126345,3.631859088419));
#31744=CARTESIAN_POINT('Ctrl Pts',(-0.4639474956053,5.080833363824,3.578558730809));
#31745=CARTESIAN_POINT('Ctrl Pts',(-0.4650065404483,5.085324729669,3.576944781319));
#31746=CARTESIAN_POINT('Origin',(-0.2886751345948,3.799999998586,4.3));
#31747=CARTESIAN_POINT('Ctrl Pts',(0.009474644443544,2.328658952906,3.818094956611));
#31748=CARTESIAN_POINT('Ctrl Pts',(0.0105988341721,2.333765482268,3.820056164338));
#31749=CARTESIAN_POINT('Ctrl Pts',(0.04385068457141,2.485729493349,3.878069544614));
#31750=CARTESIAN_POINT('Ctrl Pts',(0.09915489585668,2.792156941505,3.974710259671));
#31751=CARTESIAN_POINT('Ctrl Pts',(0.1527218994168,3.281111771178,4.068490389354));
#31752=CARTESIAN_POINT('Ctrl Pts',(0.1656911157868,3.626085089004,4.091220199701));
#31753=CARTESIAN_POINT('Ctrl Pts',(0.1654730928139,3.811221437351,4.090839298692));
#31754=CARTESIAN_POINT('Ctrl Pts',(0.1654598554814,3.816831728666,4.090816203645));
#31755=CARTESIAN_POINT('Ctrl Pts',(-0.07780099826889,2.410332609439,3.642259301122));
#31756=CARTESIAN_POINT('Ctrl Pts',(-0.07668813260086,2.415162439761,3.644097597749));
#31757=CARTESIAN_POINT('Ctrl Pts',(-0.04377154882854,2.558889003431,3.698474311926));
#31758=CARTESIAN_POINT('Ctrl Pts',(0.01095237427205,2.848518182611,3.789008170026));
#31759=CARTESIAN_POINT('Ctrl Pts',(0.06392943237314,3.310252236621,3.87680411232));
#31760=CARTESIAN_POINT('Ctrl Pts',(0.07675144997308,3.635852231929,3.89807481882));
#31761=CARTESIAN_POINT('Ctrl Pts',(0.07653600950347,3.810591236453,3.897718345495));
#31762=CARTESIAN_POINT('Ctrl Pts',(0.07652293033348,3.815886452588,3.897696729126));
#31763=CARTESIAN_POINT('Ctrl Pts',(-0.2567329809627,2.48046290541,3.551314900382));
#31764=CARTESIAN_POINT('Ctrl Pts',(-0.2556433318135,2.485066389654,3.553024302123));
#31765=CARTESIAN_POINT('Ctrl Pts',(-0.2234141096054,2.622049040122,3.60358597455));
#31766=CARTESIAN_POINT('Ctrl Pts',(-0.1698798897507,2.897605700672,3.68764162277));
#31767=CARTESIAN_POINT('Ctrl Pts',(-0.1181123341796,3.335834773715,3.769004622719));
#31768=CARTESIAN_POINT('Ctrl Pts',(-0.1055921025872,3.644427145636,3.788694227807));
#31769=CARTESIAN_POINT('Ctrl Pts',(-0.1058022484245,3.810037961682,3.788364190593));
#31770=CARTESIAN_POINT('Ctrl Pts',(-0.1058150033307,3.8150565647,3.788344170967));
#31771=CARTESIAN_POINT('Ctrl Pts',(-0.4650171874696,2.514630471845,3.576928594623));
#31772=CARTESIAN_POINT('Ctrl Pts',(-0.4639545633057,2.519136776674,3.57854799889));
#31773=CARTESIAN_POINT('Ctrl Pts',(-0.4325254583033,2.653217278719,3.626444651451));
#31774=CARTESIAN_POINT('Ctrl Pts',(-0.3803761020868,2.922327221957,3.705906449542));
#31775=CARTESIAN_POINT('Ctrl Pts',(-0.3300164573371,3.348951543072,3.782627702705));
#31776=CARTESIAN_POINT('Ctrl Pts',(-0.3178475171024,3.648824045183,3.801164748326));
#31777=CARTESIAN_POINT('Ctrl Pts',(-0.3180514997693,3.809754263313,3.800853950596));
#31778=CARTESIAN_POINT('Ctrl Pts',(-0.318063877219,3.814631031964,3.800835089794));
#31779=CARTESIAN_POINT('Origin',(-0.4330127019009,2.355181672278,4.049999999985));
#31780=CARTESIAN_POINT('Ctrl Pts',(-0.01268225231146,1.827199165611,3.694029057209));
#31781=CARTESIAN_POINT('Ctrl Pts',(-0.01301759300711,1.860931244349,3.712030310352));
#31782=CARTESIAN_POINT('Ctrl Pts',(-0.01039416625468,1.95192169302,3.759169815227));
#31783=CARTESIAN_POINT('Ctrl Pts',(0.007243775571969,2.110691864198,3.834329624173));
#31784=CARTESIAN_POINT('Ctrl Pts',(0.03200461518363,2.243916778438,3.889613928573));
#31785=CARTESIAN_POINT('Ctrl Pts',(0.04752295460543,2.315712820635,3.91708532505));
#31786=CARTESIAN_POINT('Ctrl Pts',(0.0486419497013,2.320840670637,3.919035840936));
#31787=CARTESIAN_POINT('Ctrl Pts',(-0.06997922130649,1.944219997842,3.474398904349));
#31788=CARTESIAN_POINT('Ctrl Pts',(-0.07032634590019,1.976515219533,3.491637536804));
#31789=CARTESIAN_POINT('Ctrl Pts',(-0.06761185180598,2.063452898229,3.53664207313));
#31790=CARTESIAN_POINT('Ctrl Pts',(-0.04957368891527,2.214589162901,3.607995942418));
#31791=CARTESIAN_POINT('Ctrl Pts',(-0.02442010395647,2.341021383202,3.6602310987));
#31792=CARTESIAN_POINT('Ctrl Pts',(-0.008697103908191,2.409075148295,3.686137285925));
#31793=CARTESIAN_POINT('Ctrl Pts',(-0.007563534861443,2.413935321588,3.687976404913));
#31794=CARTESIAN_POINT('Ctrl Pts',(-0.2743702035042,2.014941453006,3.338610219497));
#31795=CARTESIAN_POINT('Ctrl Pts',(-0.2747593638729,2.049740450048,3.357212410043));
#31796=CARTESIAN_POINT('Ctrl Pts',(-0.2717200123951,2.142267225392,3.404879810831));
#31797=CARTESIAN_POINT('Ctrl Pts',(-0.2522541723024,2.299455101574,3.47783355744));
#31798=CARTESIAN_POINT('Ctrl Pts',(-0.22569957768,2.428417376632,3.529601984769));
#31799=CARTESIAN_POINT('Ctrl Pts',(-0.2092465078358,2.497297199027,3.554946751002));
#31800=CARTESIAN_POINT('Ctrl Pts',(-0.2080609502775,2.502213777215,3.556744267749));
#31801=CARTESIAN_POINT('Ctrl Pts',(-0.5292956670928,2.005952905416,3.350813053175));
#31802=CARTESIAN_POINT('Ctrl Pts',(-0.5297372563374,2.046013462642,3.372260800848));
#31803=CARTESIAN_POINT('Ctrl Pts',(-0.5262927283777,2.151130768936,3.426130893777));
#31804=CARTESIAN_POINT('Ctrl Pts',(-0.5050462261996,2.325196838465,3.505334511686));
#31805=CARTESIAN_POINT('Ctrl Pts',(-0.4767442304242,2.464816654345,3.559439123932));
#31806=CARTESIAN_POINT('Ctrl Pts',(-0.4593805852738,2.538700617836,3.585491487078));
#31807=CARTESIAN_POINT('Ctrl Pts',(-0.4581301853469,2.543971035405,3.587336850206));
#31808=CARTESIAN_POINT('',(-0.020178900715945,1.85334863830895,3.67573612706027));
#31809=CARTESIAN_POINT('Ctrl Pts',(5.78773784938718E-13,2.355181672324,
3.80000000000086));
#31810=CARTESIAN_POINT('Ctrl Pts',(-0.00259348412084394,2.32958325346104,
3.79550811878464));
#31811=CARTESIAN_POINT('Ctrl Pts',(-0.0050129340853925,2.30398482576912,
3.79079385831531));
#31812=CARTESIAN_POINT('Ctrl Pts',(-0.00722157512980347,2.27856539847399,
3.78588019449874));
#31813=CARTESIAN_POINT('Ctrl Pts',(-0.0094302161742131,2.25314597117887,
3.78096653068217));
#31814=CARTESIAN_POINT('Ctrl Pts',(-0.0114322186707008,2.22790547510456,
3.77585564649884));
#31815=CARTESIAN_POINT('Ctrl Pts',(-0.0132303451805874,2.20242095353657,
3.77044240629286));
#31816=CARTESIAN_POINT('Ctrl Pts',(-0.0145671608308309,2.18347450728612,
3.76641793738809));
#31817=CARTESIAN_POINT('Ctrl Pts',(-0.0157899159720803,2.16439402966783,
3.76222640653729));
#31818=CARTESIAN_POINT('Ctrl Pts',(-0.0168856972943328,2.14510636267199,
3.75782462812579));
#31819=CARTESIAN_POINT('Ctrl Pts',(-0.0172638315745967,2.13845053825764,
3.75630565415014));
#31820=CARTESIAN_POINT('Ctrl Pts',(-0.0176267490905933,2.13177009729399,
3.75476161339509));
#31821=CARTESIAN_POINT('Ctrl Pts',(-0.0179734794456808,2.12506244269226,
3.75319088822452));
#31822=CARTESIAN_POINT('Ctrl Pts',(-0.0190646827361773,2.1039526244559,
3.74824762193864));
#31823=CARTESIAN_POINT('Ctrl Pts',(-0.0199991533623702,2.08257197318519,
3.74303980220404));
#31824=CARTESIAN_POINT('Ctrl Pts',(-0.020737879582049,2.06065772311987,
3.73745866791453));
#31825=CARTESIAN_POINT('Ctrl Pts',(-0.0209141010770433,2.05543012755698,
3.73612730075569));
#31826=CARTESIAN_POINT('Ctrl Pts',(-0.0210789980621449,2.05017229709023,
3.73477465577134));
#31827=CARTESIAN_POINT('Ctrl Pts',(-0.0212316696078731,2.04488092819401,
3.7333992003443));
#31828=CARTESIAN_POINT('Ctrl Pts',(-0.021644207299719,2.03058298484946,
3.72968254702556));
#31829=CARTESIAN_POINT('Ctrl Pts',(-0.0219699971594484,2.01604450125176,
3.72580198438638));
#31830=CARTESIAN_POINT('Ctrl Pts',(-0.0221928799302953,2.00089825894294,
3.72161269769981));
#31831=CARTESIAN_POINT('Ctrl Pts',(-0.0223982579968669,1.98694156794618,
3.71775242803099));
#31832=CARTESIAN_POINT('Ctrl Pts',(-0.0225164979983158,1.97246858060208,
3.7136298178958));
#31833=CARTESIAN_POINT('Ctrl Pts',(-0.0225031916269554,1.95721439476657,
3.70912669446936));
#31834=CARTESIAN_POINT('Ctrl Pts',(-0.0225017100281382,1.95551591641515,
3.70862529388752));
#31835=CARTESIAN_POINT('Ctrl Pts',(-0.0224985391601981,1.95380776921443,
3.70811923182651));
#31836=CARTESIAN_POINT('Ctrl Pts',(-0.0224936160594434,1.95209019693844,
3.70760844201206));
#31837=CARTESIAN_POINT('Ctrl Pts',(-0.0224399754837185,1.93337606324044,
3.70204303494726));
#31838=CARTESIAN_POINT('Ctrl Pts',(-0.022180408083899,1.91354025838126,
3.69591382635628));
#31839=CARTESIAN_POINT('Ctrl Pts',(-0.0216189713074668,1.89293208130006,
3.68916541028671));
#31840=CARTESIAN_POINT('Ctrl Pts',(-0.0212669316344575,1.88001006367398,
3.68493392726637));
#31841=CARTESIAN_POINT('Ctrl Pts',(-0.0207956678806571,1.86678504453139,
3.68045958413581));
#31842=CARTESIAN_POINT('Ctrl Pts',(-0.020176966977485,1.85334980564532,
3.67573540519852));
#31843=CARTESIAN_POINT('Origin',(-0.5,1.78753882025,3.8));
#31844=CARTESIAN_POINT('Ctrl Pts',(0.01155951010132,2.380682544795,3.819157949804));
#31845=CARTESIAN_POINT('Ctrl Pts',(0.01246241576851,2.375339654434,3.820721864307));
#31846=CARTESIAN_POINT('Ctrl Pts',(0.0169512535827,2.348900772593,3.828496902369));
#31847=CARTESIAN_POINT('Ctrl Pts',(0.02510386697286,2.301991385,3.842617643754));
#31848=CARTESIAN_POINT('Ctrl Pts',(0.03620327875676,2.240589380903,3.861842388624));
#31849=CARTESIAN_POINT('Ctrl Pts',(0.04760543423679,2.180147839132,3.881591501305));
#31850=CARTESIAN_POINT('Ctrl Pts',(0.05961053663961,2.119669925868,3.902384948596));
#31851=CARTESIAN_POINT('Ctrl Pts',(0.07279883802991,2.057561847955,3.925227756676));
#31852=CARTESIAN_POINT('Ctrl Pts',(0.08339615424009,2.012042225791,3.943582846774));
#31853=CARTESIAN_POINT('Ctrl Pts',(0.08936855627525,1.988452335483,3.953927350542));
#31854=CARTESIAN_POINT('Ctrl Pts',(0.09055372500124,1.983862542045,3.955980122991));
#31855=CARTESIAN_POINT('Ctrl Pts',(-0.04842903935518,2.342223142484,3.722320777306));
#31856=CARTESIAN_POINT('Ctrl Pts',(-0.04750543477618,2.336759152394,3.723920396082));
#31857=CARTESIAN_POINT('Ctrl Pts',(-0.04291667013141,2.309736402476,3.731867928017));
#31858=CARTESIAN_POINT('Ctrl Pts',(-0.03459915065528,2.261875354762,3.746274291935));
#31859=CARTESIAN_POINT('Ctrl Pts',(-0.02322915381834,2.198975091133,3.765967704986));
#31860=CARTESIAN_POINT('Ctrl Pts',(-0.01151371840005,2.136868627655,3.786259434136));
#31861=CARTESIAN_POINT('Ctrl Pts',(0.0009395902779249,2.074121416472,3.807829197551));
#31862=CARTESIAN_POINT('Ctrl Pts',(0.01478980849077,2.00888405034,3.831818479172));
#31863=CARTESIAN_POINT('Ctrl Pts',(0.02612878395871,1.960130298146,3.851458160798));
#31864=CARTESIAN_POINT('Ctrl Pts',(0.03276598174019,1.933903035583,3.862954124575));
#31865=CARTESIAN_POINT('Ctrl Pts',(0.03409521153101,1.928749916997,3.865256418107));
#31866=CARTESIAN_POINT('Ctrl Pts',(-0.0891849279982,2.304179010464,3.615799475541));
#31867=CARTESIAN_POINT('Ctrl Pts',(-0.08824084421946,2.298595247152,3.61743441963));
#31868=CARTESIAN_POINT('Ctrl Pts',(-0.08355321678755,2.270995008595,3.625552608771));
#31869=CARTESIAN_POINT('Ctrl Pts',(-0.07507257221585,2.222192578715,3.640241510491));
#31870=CARTESIAN_POINT('Ctrl Pts',(-0.06343491265144,2.157810236795,3.660398530094));
#31871=CARTESIAN_POINT('Ctrl Pts',(-0.05140958072686,2.094056832808,3.681227015441));
#31872=CARTESIAN_POINT('Ctrl Pts',(-0.03851290641217,2.029064832183,3.703564710746));
#31873=CARTESIAN_POINT('Ctrl Pts',(-0.02400792010097,1.96073197423,3.728688083965));
#31874=CARTESIAN_POINT('Ctrl Pts',(-0.01193529529924,1.908779020696,3.749598483488));
#31875=CARTESIAN_POINT('Ctrl Pts',(-0.004640481584497,1.879942869568,3.762233471476));
#31876=CARTESIAN_POINT('Ctrl Pts',(-0.003168746593044,1.87423250976,3.764782591257));
#31877=CARTESIAN_POINT('Ctrl Pts',(-0.1094003325662,2.267770953937,3.503012226299));
#31878=CARTESIAN_POINT('Ctrl Pts',(-0.1084366464606,2.262072587335,3.504680983176));
#31879=CARTESIAN_POINT('Ctrl Pts',(-0.1036543927112,2.233919770715,3.512962516607));
#31880=CARTESIAN_POINT('Ctrl Pts',(-0.09501763858581,2.184216444809,3.527921804991));
#31881=CARTESIAN_POINT('Ctrl Pts',(-0.08312382769833,2.118415764526,3.54852249276));
#31882=CARTESIAN_POINT('Ctrl Pts',(-0.07080192702584,2.053086250209,3.569864649964));
#31883=CARTESIAN_POINT('Ctrl Pts',(-0.05748095495493,1.985946002084,3.592937250614));
#31884=CARTESIAN_POINT('Ctrl Pts',(-0.0423493602444,1.914650780515,3.619145941414));
#31885=CARTESIAN_POINT('Ctrl Pts',(-0.02957463824225,1.859636214095,3.641272408901));
#31886=CARTESIAN_POINT('Ctrl Pts',(-0.02165049076681,1.828303375201,3.654997434942));
#31887=CARTESIAN_POINT('Ctrl Pts',(-0.02004237931471,1.822059739515,3.657782765687));
#31888=CARTESIAN_POINT('Origin',(0.9394619912652,1.984948516829,3.427195899532));
#31889=CARTESIAN_POINT('Ctrl Pts',(0.2115271085781,2.123801978059,4.099083165178));
#31890=CARTESIAN_POINT('Ctrl Pts',(0.2121262002231,2.114600129107,4.101333173451));
#31891=CARTESIAN_POINT('Ctrl Pts',(0.2164404968357,2.037191262064,4.119100527721));
#31892=CARTESIAN_POINT('Ctrl Pts',(0.2139962921771,1.899196368833,4.13258925162));
#31893=CARTESIAN_POINT('Ctrl Pts',(0.199524436147,1.716490317037,4.126202722674));
#31894=CARTESIAN_POINT('Ctrl Pts',(0.1774106709109,1.531708228466,4.100979757227));
#31895=CARTESIAN_POINT('Ctrl Pts',(0.1581803697853,1.403457455766,4.072215873524));
#31896=CARTESIAN_POINT('Ctrl Pts',(0.1469204644944,1.334496569053,4.053834130917));
#31897=CARTESIAN_POINT('Ctrl Pts',(0.1458524770939,1.328006904403,4.052078570375));
#31898=CARTESIAN_POINT('Ctrl Pts',(0.08366135428003,2.034390998194,3.978928836562));
#31899=CARTESIAN_POINT('Ctrl Pts',(0.08417860878662,2.026727285286,3.980132428517));
#31900=CARTESIAN_POINT('Ctrl Pts',(0.08801831539764,1.962051030615,3.989335305632));
#31901=CARTESIAN_POINT('Ctrl Pts',(0.08768495610394,1.843574140367,3.991294021376));
#31902=CARTESIAN_POINT('Ctrl Pts',(0.0790739523643,1.682126401741,3.97369060683));
#31903=CARTESIAN_POINT('Ctrl Pts',(0.06477019106634,1.515735601788,3.939795644756));
#31904=CARTESIAN_POINT('Ctrl Pts',(0.05184529653118,1.398767721864,3.906400952433));
#31905=CARTESIAN_POINT('Ctrl Pts',(0.04416796124159,1.3355924808,3.885851412206));
#31906=CARTESIAN_POINT('Ctrl Pts',(0.0434388747213,1.329644894934,3.883894614747));
#31907=CARTESIAN_POINT('Ctrl Pts',(0.002069708769611,1.941910036321,3.825396483512));
#31908=CARTESIAN_POINT('Ctrl Pts',(0.002564130319744,1.935902935356,3.825625402323));
#31909=CARTESIAN_POINT('Ctrl Pts',(0.006443211256808,1.884925816002,3.826897945044));
#31910=CARTESIAN_POINT('Ctrl Pts',(0.009358963854998,1.787220641492,3.81893556933));
#31911=CARTESIAN_POINT('Ctrl Pts',(0.008197891072037,1.647895242108,3.792711139866));
#31912=CARTESIAN_POINT('Ctrl Pts',(0.003243085717919,1.500137582073,3.75300481842));
#31913=CARTESIAN_POINT('Ctrl Pts',(-0.002415465510452,1.394244822581,3.717041504595));
#31914=CARTESIAN_POINT('Ctrl Pts',(-0.00603250719455,1.336650568951,3.695440705072));
#31915=CARTESIAN_POINT('Ctrl Pts',(-0.006378080860699,1.33122498004,3.693387794139));
#31916=CARTESIAN_POINT('Ctrl Pts',(-0.02637845939937,1.854145254949,3.651412310807));
#31917=CARTESIAN_POINT('Ctrl Pts',(-0.02584594427012,1.849773768258,3.650820359384));
#31918=CARTESIAN_POINT('Ctrl Pts',(-0.021416839685,1.812308948769,3.645464381648));
#31919=CARTESIAN_POINT('Ctrl Pts',(-0.01438725808483,1.734880389255,3.630025108279));
#31920=CARTESIAN_POINT('Ctrl Pts',(-0.007136546264389,1.616678829914,3.598501355566));
#31921=CARTESIAN_POINT('Ctrl Pts',(-0.001990551510268,1.486227398703,3.556333582309));
#31922=CARTESIAN_POINT('Ctrl Pts',(-3.359111288803E-5,1.390269550117,3.520080091633));
#31923=CARTESIAN_POINT('Ctrl Pts',(0.0005455399378233,1.337581750887,3.498633078821));
#31924=CARTESIAN_POINT('Ctrl Pts',(0.0005958023632368,1.332614129104,3.496597269846));
#31925=CARTESIAN_POINT('Ctrl Pts',(-0.0201796772031231,1.8533485682179,
3.67573602729754));
#31926=CARTESIAN_POINT('Ctrl Pts',(-0.0180484169316047,1.8332062091452,
3.67329927372651));
#31927=CARTESIAN_POINT('Ctrl Pts',(-0.0161673154615857,1.81251453951732,
3.67012899402731));
#31928=CARTESIAN_POINT('Ctrl Pts',(-0.0144832545962451,1.79133257575351,
3.66632891140682));
#31929=CARTESIAN_POINT('Ctrl Pts',(-0.0132428308424302,1.77573063906237,
3.66352989573825));
#31930=CARTESIAN_POINT('Ctrl Pts',(-0.0121097653213558,1.75986214367113,
3.66038763081213));
#31931=CARTESIAN_POINT('Ctrl Pts',(-0.0110658077287692,1.74375337710359,
3.65693080646843));
#31932=CARTESIAN_POINT('Ctrl Pts',(-0.0110657287678007,1.74375215869796,
3.65693054500743));
#31933=CARTESIAN_POINT('Ctrl Pts',(-0.0110656498073422,1.74375094029096,
3.65693028354462));
#31934=CARTESIAN_POINT('Ctrl Pts',(-0.0110655708473939,1.74374972188258,
3.65693002208001));
#31935=CARTESIAN_POINT('Ctrl Pts',(-0.00930360226254986,1.71656128866799,
3.65109551441564));
#31936=CARTESIAN_POINT('Ctrl Pts',(-0.00779274517230981,1.68868734172387,
3.64437242260396));
#31937=CARTESIAN_POINT('Ctrl Pts',(-0.00648446807086871,1.6598387869057,
3.63673330275129));
#31938=CARTESIAN_POINT('Ctrl Pts',(-0.00596516871011799,1.64838782131198,
3.63370107811644));
#31939=CARTESIAN_POINT('Ctrl Pts',(-0.00547802320827809,1.63678336231907,
3.6305239294403));
#31940=CARTESIAN_POINT('Ctrl Pts',(-0.00502072425409526,1.62500842706159,
3.62719837418674));
#31941=CARTESIAN_POINT('Ctrl Pts',(-0.0038958181749634,1.59604335698791,
3.61901786713113));
#31942=CARTESIAN_POINT('Ctrl Pts',(-0.00295103873268496,1.56604766064031,
3.60994448283711));
#31943=CARTESIAN_POINT('Ctrl Pts',(-0.00219243495539221,1.53482829685866,
3.59984407614345));
#31944=CARTESIAN_POINT('Ctrl Pts',(-0.00186572146376575,1.52138282288031,
3.59549405939358));
#31945=CARTESIAN_POINT('Ctrl Pts',(-0.00157359566811571,1.50771092696239,
3.59095334765681));
#31946=CARTESIAN_POINT('Ctrl Pts',(-0.00131664102690395,1.49380028354877,
3.58621075218851));
#31947=CARTESIAN_POINT('Ctrl Pts',(-0.000714403889778184,1.46119722946308,
3.57509529965609));
#31948=CARTESIAN_POINT('Ctrl Pts',(-0.000305670842863149,1.42727766026637,
3.56287477923549));
#31949=CARTESIAN_POINT('Ctrl Pts',(-0.000118133862968915,1.39214305106515,
3.54946527329762));
#31950=CARTESIAN_POINT('Ctrl Pts',(-3.98644057114186E-5,1.37747945354596,
3.54386875173457));
#31951=CARTESIAN_POINT('Ctrl Pts',(-4.70921629019157E-9,1.36260469734931,
3.53806544891218));
#31952=CARTESIAN_POINT('Ctrl Pts',(4.91088626388035E-16,1.34752836903785,
3.5320508077706));
#31953=CARTESIAN_POINT('Origin',(-0.5,3.8,0.));
#31954=CARTESIAN_POINT('Origin',(-0.5,3.8,0.));
#31955=CARTESIAN_POINT('Origin',(-0.5,3.8,0.));
#31956=CARTESIAN_POINT('',(-1.,3.76739364408005,3.29983890903081));
#31957=CARTESIAN_POINT('Origin',(-1.,3.8,0.));
#31958=CARTESIAN_POINT('Origin',(-0.5,3.76739364408005,3.29983890903081));
#31959=CARTESIAN_POINT('Origin',(-0.5,3.8,0.));
#31960=CARTESIAN_POINT('Origin',(-0.5,3.8,0.));
#31961=CARTESIAN_POINT('',(-0.0201844691181272,1.85335594570995,-3.67572064370324));
#31962=CARTESIAN_POINT('Ctrl Pts',(-0.0201847187606871,1.85335594052431,
-3.67572046601124));
#31963=CARTESIAN_POINT('Ctrl Pts',(-0.0178286956184653,1.83115373899016,
-3.67305838240737));
#31964=CARTESIAN_POINT('Ctrl Pts',(-0.0158360667308249,1.80880940789044,
-3.66956936811219));
#31965=CARTESIAN_POINT('Ctrl Pts',(-0.014084148622304,1.78626234395626,
-3.6654249360026));
#31966=CARTESIAN_POINT('Ctrl Pts',(-0.0137453719972492,1.7819023124072,
-3.66462350771893));
#31967=CARTESIAN_POINT('Ctrl Pts',(-0.0134157389998275,1.77753464578999,
-3.66379760651892));
#31968=CARTESIAN_POINT('Ctrl Pts',(-0.0130945604005602,1.77315882973048,
-3.66294851672634));
#31969=CARTESIAN_POINT('Ctrl Pts',(-0.0111124584923371,1.74615418688884,
-3.65770849605876));
#31970=CARTESIAN_POINT('Ctrl Pts',(-0.00945014572111559,1.71884148228237,
-3.65158466669008));
#31971=CARTESIAN_POINT('Ctrl Pts',(-0.00803275747314458,1.69159897117484,
-3.64485043816951));
#31972=CARTESIAN_POINT('Ctrl Pts',(-0.0066153692251727,1.6643564600673,
-3.63811620964893));
#31973=CARTESIAN_POINT('Ctrl Pts',(-0.00544334631616801,1.63718405974905,
-3.63077174059948));
#31974=CARTESIAN_POINT('Ctrl Pts',(-0.0044617006739997,1.61012025342433,
-3.62294164204283));
#31975=CARTESIAN_POINT('Ctrl Pts',(-0.00360980208403964,1.58663355164868,
-3.61614647112462));
#31976=CARTESIAN_POINT('Ctrl Pts',(-0.00290086724187045,1.5632287435596,
-3.60898422005949));
#31977=CARTESIAN_POINT('Ctrl Pts',(-0.00230378770602957,1.53931614496347,
-3.6012916794294));
#31978=CARTESIAN_POINT('Ctrl Pts',(-0.00221285046229865,1.53567417488035,
-3.60012007933226));
#31979=CARTESIAN_POINT('Ctrl Pts',(-0.00212456287768805,1.53202042666967,
-3.59893609696379));
#31980=CARTESIAN_POINT('Ctrl Pts',(-0.00203887417552023,1.52835281933648,
-3.59773906580883));
#31981=CARTESIAN_POINT('Ctrl Pts',(-0.00146807360102199,1.5039216829106,
-3.58976524833164));
#31982=CARTESIAN_POINT('Ctrl Pts',(-0.0010109478997301,1.47887566655908,
-3.58121621087756));
#31983=CARTESIAN_POINT('Ctrl Pts',(-0.000671404729556291,1.45271668694635,
-3.57185779465556));
#31984=CARTESIAN_POINT('Ctrl Pts',(-0.000625299613279142,1.44916467087687,
-3.57058705530343));
#31985=CARTESIAN_POINT('Ctrl Pts',(-0.000581394318175335,1.44559214758773,
-3.56930132189872));
#31986=CARTESIAN_POINT('Ctrl Pts',(-0.000539729159247049,1.4419978838711,
-3.56799993917551));
#31987=CARTESIAN_POINT('Ctrl Pts',(-0.000191219093601024,1.41193350595798,
-3.55711446579763));
#31988=CARTESIAN_POINT('Ctrl Pts',(9.14699587802441E-12,1.3803466764801,
-3.54514076878014));
#31989=CARTESIAN_POINT('Ctrl Pts',(0.,1.347528369805,-3.53205080767908));
#31990=CARTESIAN_POINT('Origin',(-0.4999999999811,0.6012805114691,-2.873707297839));
#31991=CARTESIAN_POINT('Origin',(-0.5,1.7875388203,-3.800000000026));
#31992=CARTESIAN_POINT('Ctrl Pts',(-0.02638274264885,1.854145296489,-3.651397889487));
#31993=CARTESIAN_POINT('Ctrl Pts',(-0.02584988028328,1.849776362744,-3.650806899679));
#31994=CARTESIAN_POINT('Ctrl Pts',(-0.02244403090875,1.820986653244,-3.646694311958));
#31995=CARTESIAN_POINT('Ctrl Pts',(-0.01704332156225,1.765138511257,-3.636247413713));
#31996=CARTESIAN_POINT('Ctrl Pts',(-0.011276325478,1.685711356068,-3.617149671255));
#31997=CARTESIAN_POINT('Ctrl Pts',(-0.006856393552252,1.605666931733,-3.594547441496));
#31998=CARTESIAN_POINT('Ctrl Pts',(-0.003478222547858,1.523897199579,-3.568495084708));
#31999=CARTESIAN_POINT('Ctrl Pts',(-0.0009679363545506,1.437662225789,-3.538088485335));
#32000=CARTESIAN_POINT('Ctrl Pts',(0.0001515744128949,1.373436283524,-3.513228241255));
#32001=CARTESIAN_POINT('Ctrl Pts',(0.0005455151103873,1.337581706695,-3.498632990864));
#32002=CARTESIAN_POINT('Ctrl Pts',(0.0005957202757987,1.332613906773,-3.496597029118));
#32003=CARTESIAN_POINT('Ctrl Pts',(0.00205755759891,1.941929047829,-3.825367870495));
#32004=CARTESIAN_POINT('Ctrl Pts',(0.002553460349221,1.935923592207,-3.825601796816));
#32005=CARTESIAN_POINT('Ctrl Pts',(0.005541994612222,1.896743544731,-3.826597574823));
#32006=CARTESIAN_POINT('Ctrl Pts',(0.008399401037005,1.825089858117,-3.822450688835));
#32007=CARTESIAN_POINT('Ctrl Pts',(0.009008797399017,1.729047222386,-3.808392608073));
#32008=CARTESIAN_POINT('Ctrl Pts',(0.007576840272114,1.635755871874,-3.788775319885));
#32009=CARTESIAN_POINT('Ctrl Pts',(0.004676582779189,1.542788345155,-3.764464411949));
#32010=CARTESIAN_POINT('Ctrl Pts',(0.0004113178430084,1.446514215098,-3.734924187794));
#32011=CARTESIAN_POINT('Ctrl Pts',(-0.003570928637939,1.375843575995,-3.710140370327));
#32012=CARTESIAN_POINT('Ctrl Pts',(-0.006032522862356,1.336650553949,-3.695440720027));
#32013=CARTESIAN_POINT('Ctrl Pts',(-0.006378128922918,1.331224937371,-3.693387619733));
#32014=CARTESIAN_POINT('Ctrl Pts',(0.08364112782225,2.034430165208,-3.978886092457));
#32015=CARTESIAN_POINT('Ctrl Pts',(0.08416102368134,2.026767191475,-3.98009867518));
#32016=CARTESIAN_POINT('Ctrl Pts',(0.0871248314785,1.977053136641,-3.987203326034));
#32017=CARTESIAN_POINT('Ctrl Pts',(0.08809270195467,1.889253530143,-3.991157591204));
#32018=CARTESIAN_POINT('Ctrl Pts',(0.08428392479652,1.775987832278,-3.984476044373));
#32019=CARTESIAN_POINT('Ctrl Pts',(0.07759850531386,1.66873570053,-3.970038442414));
#32020=CARTESIAN_POINT('Ctrl Pts',(0.06890748642892,1.563749976296,-3.949586172014));
#32021=CARTESIAN_POINT('Ctrl Pts',(0.05826440232022,1.4564802135,-3.92303550761));
#32022=CARTESIAN_POINT('Ctrl Pts',(0.04939263231509,1.378583011643,-3.899835567345));
#32023=CARTESIAN_POINT('Ctrl Pts',(0.04416795177121,1.335592487269,-3.885851523854));
#32024=CARTESIAN_POINT('Ctrl Pts',(0.04343885083342,1.329645016683,-3.883894494899));
#32025=CARTESIAN_POINT('Ctrl Pts',(0.2114992793448,2.123860789188,-4.099027540324));
#32026=CARTESIAN_POINT('Ctrl Pts',(0.2121021010075,2.114658850969,-4.101290124628));
#32027=CARTESIAN_POINT('Ctrl Pts',(0.2154358527566,2.055153999154,-4.11498983687));
#32028=CARTESIAN_POINT('Ctrl Pts',(0.2153270381774,1.952227455737,-4.128164339508));
#32029=CARTESIAN_POINT('Ctrl Pts',(0.2082114888224,1.822581159193,-4.130575153272));
#32030=CARTESIAN_POINT('Ctrl Pts',(0.1973133334883,1.701829778055,-4.123075893756));
#32031=CARTESIAN_POINT('Ctrl Pts',(0.1838067564356,1.585017290136,-4.108274582941));
#32032=CARTESIAN_POINT('Ctrl Pts',(0.1677205468331,1.466721163078,-4.086584965633));
#32033=CARTESIAN_POINT('Ctrl Pts',(0.1545831460761,1.381423951742,-4.066343003277));
#32034=CARTESIAN_POINT('Ctrl Pts',(0.1469204577389,1.334496587465,-4.053834324906));
#32035=CARTESIAN_POINT('Ctrl Pts',(0.1458524654956,1.328007161482,-4.05207848873));
#32036=CARTESIAN_POINT('Origin',(0.9394505533555,1.984989544106,-3.427176090634));
#32037=CARTESIAN_POINT('Origin',(1.,1.347528370653,-3.532050807569));
#32038=CARTESIAN_POINT('Origin',(1.,7.013523051583,-3.532050807569));
#32039=CARTESIAN_POINT('Origin',(1.00128642976697,0.666005481541297,-3.53122253848802));
#32040=CARTESIAN_POINT('Ctrl Pts',(0.1488993956888,0.7179069965694,-4.051886351638));
#32041=CARTESIAN_POINT('Ctrl Pts',(0.1385570697474,0.7162110101831,-4.035126874871));
#32042=CARTESIAN_POINT('Ctrl Pts',(0.1176862605854,0.7126138946773,-3.998941337807));
#32043=CARTESIAN_POINT('Ctrl Pts',(0.08933527303172,0.7071386038102,-3.94173474656));
#32044=CARTESIAN_POINT('Ctrl Pts',(0.06394561213802,0.7015141325995,-3.880575776974));
#32045=CARTESIAN_POINT('Ctrl Pts',(0.04268217099292,0.6959732845635,-3.817856726743));
#32046=CARTESIAN_POINT('Ctrl Pts',(0.0256383433447,0.6905443235702,-3.753851548948));
#32047=CARTESIAN_POINT('Ctrl Pts',(0.01289006426926,0.6852543476883,-3.688839944825));
#32048=CARTESIAN_POINT('Ctrl Pts',(0.004495469108308,0.6801291657042,-3.623106745103));
#32049=CARTESIAN_POINT('Ctrl Pts',(0.0007024534571773,0.675450952114,-3.560399066502));
#32050=CARTESIAN_POINT('Ctrl Pts',(0.0007422179452603,0.6725379290189,-3.519663636229));
#32051=CARTESIAN_POINT('Ctrl Pts',(0.001283538221875,0.6712323506797,-3.501040402923));
#32052=CARTESIAN_POINT('Ctrl Pts',(0.1340962252224,0.3912294572926,-4.093199135617));
#32053=CARTESIAN_POINT('Ctrl Pts',(0.1234350361148,0.3894754713328,-4.075866781342));
#32054=CARTESIAN_POINT('Ctrl Pts',(0.1019235019593,0.3857557331309,-4.038448847312));
#32055=CARTESIAN_POINT('Ctrl Pts',(0.0726982435266,0.3800930011241,-3.979286595073));
#32056=CARTESIAN_POINT('Ctrl Pts',(0.04652749766874,0.3742762828842,-3.91604080453));
#32057=CARTESIAN_POINT('Ctrl Pts',(0.02460901325779,0.3685458257877,-3.851179458001));
#32058=CARTESIAN_POINT('Ctrl Pts',(0.007040378848643,0.3629311721167,-3.784988888268));
#32059=CARTESIAN_POINT('Ctrl Pts',(-0.006100719778655,0.3574601784024,-3.717755935732));
#32060=CARTESIAN_POINT('Ctrl Pts',(-0.01475389334159,0.3521598165628,-3.649778458152));
#32061=CARTESIAN_POINT('Ctrl Pts',(-0.01866387237992,0.347321433533,-3.584924958567));
#32062=CARTESIAN_POINT('Ctrl Pts',(-0.01862296859118,0.3443090775689,-3.542800463296));
#32063=CARTESIAN_POINT('Ctrl Pts',(-0.01806492014634,0.342958842281,-3.523540054914));
#32064=CARTESIAN_POINT('Ctrl Pts',(0.3373468963971,0.1525661114051,-3.991350865212));
#32065=CARTESIAN_POINT('Ctrl Pts',(0.3290504156986,0.1512072534401,-3.977811610559));
#32066=CARTESIAN_POINT('Ctrl Pts',(0.3123100833698,0.1483247372964,-3.948582265489));
#32067=CARTESIAN_POINT('Ctrl Pts',(0.2895668155851,0.1439336916915,-3.902367297901));
#32068=CARTESIAN_POINT('Ctrl Pts',(0.269201233379,0.1394199538792,-3.85296441848));
#32069=CARTESIAN_POINT('Ctrl Pts',(0.25214516126,0.1349694701275,-3.802301466759));
#32070=CARTESIAN_POINT('Ctrl Pts',(0.2384747042055,0.1306050036345,-3.750603437919));
#32071=CARTESIAN_POINT('Ctrl Pts',(0.2282499930638,0.1263479786245,-3.69809469861));
#32072=CARTESIAN_POINT('Ctrl Pts',(0.2215177543611,0.1222192691329,-3.645009086964));
#32073=CARTESIAN_POINT('Ctrl Pts',(0.2184760069348,0.1184459109448,-3.594367048629));
#32074=CARTESIAN_POINT('Ctrl Pts',(0.2185078803864,0.1160938128734,-3.561476552185));
#32075=CARTESIAN_POINT('Ctrl Pts',(0.2189419602036,0.1150389389891,-3.546438857281));
#32076=CARTESIAN_POINT('Ctrl Pts',(0.6168657267359,0.1684061772862,-3.817389898812));
#32077=CARTESIAN_POINT('Ctrl Pts',(0.6119679285382,0.1676199374555,-3.809363691671));
#32078=CARTESIAN_POINT('Ctrl Pts',(0.6020823810763,0.165950450196,-3.792031641834));
#32079=CARTESIAN_POINT('Ctrl Pts',(0.5886555921188,0.1634031025247,-3.76463500526));
#32080=CARTESIAN_POINT('Ctrl Pts',(0.5766317967327,0.1607786261806,-3.735348089483));
#32081=CARTESIAN_POINT('Ctrl Pts',(0.5665636211538,0.1581848012789,-3.705319562176));
#32082=CARTESIAN_POINT('Ctrl Pts',(0.5584949951317,0.1556342834582,-3.674682152124));
#32083=CARTESIAN_POINT('Ctrl Pts',(0.5524614350958,0.1531393609817,-3.643571720386));
#32084=CARTESIAN_POINT('Ctrl Pts',(0.5484896191243,0.1507118028103,-3.612125698284));
#32085=CARTESIAN_POINT('Ctrl Pts',(0.5466956284192,0.1484857128208,-3.58213862691));
#32086=CARTESIAN_POINT('Ctrl Pts',(0.5467146013709,0.1470928739485,-3.56266364575));
#32087=CARTESIAN_POINT('Ctrl Pts',(0.5469704950681,0.1464673385908,-3.55376282921));
#32088=CARTESIAN_POINT('',(0.51744976844956,0.145564598942594,-3.56771956646391));
#32089=CARTESIAN_POINT('Origin',(0.5,0.6439853787897,-3.532051214103));
#32090=CARTESIAN_POINT('',(0.584436854370166,0.166625187839343,-3.82024516063688));
#32091=CARTESIAN_POINT('Origin',(0.5669870682482,0.6648587286911,-3.78205040944));
#32092=CARTESIAN_POINT('Origin',(1.0290517906493,0.168032215480016,-3.56615971227102));
#32093=CARTESIAN_POINT('Origin',(0.5,50.,0.));
#32094=CARTESIAN_POINT('Origin',(0.5174497483513,50.,0.));
#32095=CARTESIAN_POINT('Ctrl Pts',(1.76192394008012E-13,0.60128128325064,
-2.87370766691881));
#32096=CARTESIAN_POINT('Ctrl Pts',(1.54230945546585E-8,0.580269199198493,
-2.82882528737468));
#32097=CARTESIAN_POINT('Ctrl Pts',(0.00101186006611363,0.560042231212748,
-2.78388483535608));
#32098=CARTESIAN_POINT('Ctrl Pts',(0.00280079850496784,0.540720477220154,
-2.73936883200466));
#32099=CARTESIAN_POINT('Ctrl Pts',(0.00380243770949192,0.529902091366951,
-2.71444400887096));
#32100=CARTESIAN_POINT('Ctrl Pts',(0.0050478023941539,0.519366499347649,
-2.68965236124796));
#32101=CARTESIAN_POINT('Ctrl Pts',(0.00649712134262853,0.509127913931286,
-2.66507931910599));
#32102=CARTESIAN_POINT('Ctrl Pts',(0.00834719043388274,0.496058264606053,
-2.63371160270872));
#32103=CARTESIAN_POINT('Ctrl Pts',(0.01052439600924,0.483477583764246,-2.60269882830449));
#32104=CARTESIAN_POINT('Ctrl Pts',(0.0130034531453356,0.471191494462817,
-2.57159451210596));
#32105=CARTESIAN_POINT('Ctrl Pts',(0.0155308113117525,0.458666027551556,
-2.53988417094012));
#32106=CARTESIAN_POINT('Ctrl Pts',(0.0183721278713497,0.446446178960187,
-2.50807870851953));
#32107=CARTESIAN_POINT('Ctrl Pts',(0.0215529360868368,0.434336243117764,
-2.47570186212255));
#32108=CARTESIAN_POINT('Ctrl Pts',(0.0220616550262061,0.43239945432063,
-2.47052370806755));
#32109=CARTESIAN_POINT('Ctrl Pts',(0.0225791610348015,0.430465508274142,
-2.46533093177464));
#32110=CARTESIAN_POINT('Ctrl Pts',(0.0231056752010314,0.428533643225277,
-2.46012157690981));
#32111=CARTESIAN_POINT('Ctrl Pts',(0.027524337805662,0.412320860367524,
-2.41640313016732));
#32112=CARTESIAN_POINT('Ctrl Pts',(0.0325718997013263,0.396259498057867,
-2.37151833744439));
#32113=CARTESIAN_POINT('Ctrl Pts',(0.0383080237524296,0.380265594004233,
-2.32497070433188));
#32114=CARTESIAN_POINT('Ctrl Pts',(0.0417209920361136,0.370749292267901,
-2.29727506977478));
#32115=CARTESIAN_POINT('Ctrl Pts',(0.0453785461737294,0.36125733554204,
-2.26899068908822));
#32116=CARTESIAN_POINT('Ctrl Pts',(0.0493002060251221,0.351777440828857,
-2.24001235735313));
#32117=CARTESIAN_POINT('Ctrl Pts',(0.0570020472340432,0.333159649759522,
-2.18310112129989));
#32118=CARTESIAN_POINT('Ctrl Pts',(0.0657293147580703,0.314588190128329,
-2.12351422609263));
#32119=CARTESIAN_POINT('Ctrl Pts',(0.0754853867545444,0.296324974395133,
-2.06149859166281));
#32120=CARTESIAN_POINT('Ctrl Pts',(0.0790459994386625,0.289659562576123,
-2.03886513276211));
#32121=CARTESIAN_POINT('Ctrl Pts',(0.0827431515444289,0.283035186810901,
-2.01590821646305));
#32122=CARTESIAN_POINT('Ctrl Pts',(0.0865752842350387,0.276464377489038,
-1.99264001890476));
#32123=CARTESIAN_POINT('Ctrl Pts',(-0.001081260139011,0.5856903810519,-2.906543661707));
#32124=CARTESIAN_POINT('Ctrl Pts',(-0.001018369255986,0.5835992009094,-2.902147314851));
#32125=CARTESIAN_POINT('Ctrl Pts',(0.0001871679450526,0.5490075761878,-2.829131820991));
#32126=CARTESIAN_POINT('Ctrl Pts',(0.007507857493721,0.4863027823338,-2.687558940315));
#32127=CARTESIAN_POINT('Ctrl Pts',(0.02870561913676,0.4029671144941,-2.474508650036));
#32128=CARTESIAN_POINT('Ctrl Pts',(0.05928519434814,0.3254023673231,-2.249119982873));
#32129=CARTESIAN_POINT('Ctrl Pts',(0.08618036230882,0.2770329575424,-2.086634502439));
#32130=CARTESIAN_POINT('Ctrl Pts',(0.1018793569146,0.2529095911706,-1.998560749934));
#32131=CARTESIAN_POINT('Ctrl Pts',(0.1027383636877,0.2516008013594,-1.993759888543));
#32132=CARTESIAN_POINT('Ctrl Pts',(0.02046330720854,0.8229529422841,-2.691466056719));
#32133=CARTESIAN_POINT('Ctrl Pts',(0.01962993973341,0.8212308194753,-2.687387423694));
#32134=CARTESIAN_POINT('Ctrl Pts',(0.005955867276286,0.7926322259833,-2.619615027721));
#32135=CARTESIAN_POINT('Ctrl Pts',(-0.01530270840099,0.7372776063719,-2.487237441822));
#32136=CARTESIAN_POINT('Ctrl Pts',(-0.03473413003973,0.6558327993806,-2.285821170463));
#32137=CARTESIAN_POINT('Ctrl Pts',(-0.04384970159776,0.5726974889928,-2.070790001253));
#32138=CARTESIAN_POINT('Ctrl Pts',(-0.04272135475251,0.5157102080513,-1.914480858456));
#32139=CARTESIAN_POINT('Ctrl Pts',(-0.04008670908317,0.4858251163379,-1.829403670676));
#32140=CARTESIAN_POINT('Ctrl Pts',(-0.03993718883915,0.484199085711,-1.824765062074));
#32141=CARTESIAN_POINT('Ctrl Pts',(-0.2045700640878,0.9936004720384,-2.53896888117));
#32142=CARTESIAN_POINT('Ctrl Pts',(-0.2060475584221,0.9912751192331,-2.535166077691));
#32143=CARTESIAN_POINT('Ctrl Pts',(-0.2303376413689,0.952617100583,-2.471943726365));
#32144=CARTESIAN_POINT('Ctrl Pts',(-0.2695762730753,0.8764813310992,-2.347474954217));
#32145=CARTESIAN_POINT('Ctrl Pts',(-0.3093746426751,0.761702271861,-2.155847204795));
#32146=CARTESIAN_POINT('Ctrl Pts',(-0.3336343557535,0.6422051540402,-1.949271087601));
#32147=CARTESIAN_POINT('Ctrl Pts',(-0.3389528302416,0.5587940338812,-1.797815533392));
#32148=CARTESIAN_POINT('Ctrl Pts',(-0.3385904718372,0.5146537484191,-1.715024763658));
#32149=CARTESIAN_POINT('Ctrl Pts',(-0.3385612404185,0.5122508977145,-1.710509733302));
#32150=CARTESIAN_POINT('Ctrl Pts',(-0.5251165549145,0.9830773465599,-2.551423432733));
#32151=CARTESIAN_POINT('Ctrl Pts',(-0.526553642486,0.9795814245021,-2.547669410243));
#32152=CARTESIAN_POINT('Ctrl Pts',(-0.5500696128295,0.9215644127028,-2.485249607032));
#32153=CARTESIAN_POINT('Ctrl Pts',(-0.5846190863906,0.8104665474727,-2.362093983857));
#32154=CARTESIAN_POINT('Ctrl Pts',(-0.6108498439799,0.6495053941253,-2.171838228225));
#32155=CARTESIAN_POINT('Ctrl Pts',(-0.6155364367152,0.4872648925674,-1.966138843811));
#32156=CARTESIAN_POINT('Ctrl Pts',(-0.6036539839724,0.3773622786505,-1.814955916913));
#32157=CARTESIAN_POINT('Ctrl Pts',(-0.5932464655588,0.320042837336,-1.732206546957));
#32158=CARTESIAN_POINT('Ctrl Pts',(-0.5926675754179,0.3169250663232,-1.727693462271));
#32159=CARTESIAN_POINT('Origin',(6.513074473852,50.,0.));
#32160=CARTESIAN_POINT('',(3.164008715435,0.8114184892106,-8.333468366184));
#32161=CARTESIAN_POINT('Origin',(-2.18195397800361,50.0038044976864,1.00000511325181));
#32162=CARTESIAN_POINT('',(3.59702142554264,0.870223962352941,-8.58602404765116));
#32163=CARTESIAN_POINT('Ctrl Pts',(3.597021417327,0.87022396206158,-8.58602404765099));
#32164=CARTESIAN_POINT('Ctrl Pts',(3.58096741891376,0.869654514666955,-8.58602213943295));
#32165=CARTESIAN_POINT('Ctrl Pts',(3.56518530891056,0.868960131303695,-8.58525072062108));
#32166=CARTESIAN_POINT('Ctrl Pts',(3.54962915365496,0.86814840013051,-8.58376106038573));
#32167=CARTESIAN_POINT('Ctrl Pts',(3.53367433186178,0.867315866255697,-8.58223322377077));
#32168=CARTESIAN_POINT('Ctrl Pts',(3.5179562710213,0.866359828090631,-8.57994970308851));
#32169=CARTESIAN_POINT('Ctrl Pts',(3.50242592358464,0.865279182771811,-8.57691263234756));
#32170=CARTESIAN_POINT('Ctrl Pts',(3.49841119994216,0.864999826992535,-8.57612752436738));
#32171=CARTESIAN_POINT('Ctrl Pts',(3.49440906403718,0.864712099679328,-8.57529179512774));
#32172=CARTESIAN_POINT('Ctrl Pts',(3.49041879141317,0.86441589178025,-8.5744049385936));
#32173=CARTESIAN_POINT('Ctrl Pts',(3.47318074105317,0.863136268265153,-8.57057370222505));
#32174=CARTESIAN_POINT('Ctrl Pts',(3.45615454157413,0.861705014691857,-8.56582824079013));
#32175=CARTESIAN_POINT('Ctrl Pts',(3.43955788599333,0.860147262011866,-8.56026314162774));
#32176=CARTESIAN_POINT('Ctrl Pts',(3.42296123041252,0.858589509331876,-8.55469804246534));
#32177=CARTESIAN_POINT('Ctrl Pts',(3.40679497637281,0.856905386133462,-8.54831381496211));
#32178=CARTESIAN_POINT('Ctrl Pts',(3.3912488155045,0.855128074940696,-8.54125787790699));
#32179=CARTESIAN_POINT('Ctrl Pts',(3.37733685737159,0.853537593592125,-8.53494365655481));
#32180=CARTESIAN_POINT('Ctrl Pts',(3.36393280439972,0.851868343374866,-8.52806545984737));
#32181=CARTESIAN_POINT('Ctrl Pts',(3.35094736280191,0.850121891066415,-8.52064611424454));
#32182=CARTESIAN_POINT('Ctrl Pts',(3.33776993736112,0.848349618255577,-8.51311707699429));
#32183=CARTESIAN_POINT('Ctrl Pts',(3.3250228795613,0.846497749897992,-8.50503043014873));
#32184=CARTESIAN_POINT('Ctrl Pts',(3.31263028034128,0.844560035369382,-8.49636064042773));
#32185=CARTESIAN_POINT('Ctrl Pts',(3.30994179241995,0.844139661724381,-8.49447979004828));
#32186=CARTESIAN_POINT('Ctrl Pts',(3.30727007445323,0.843715221628018,-8.49257132260828));
#32187=CARTESIAN_POINT('Ctrl Pts',(3.30461450965066,0.843286609495757,-8.49063469802249));
#32188=CARTESIAN_POINT('Ctrl Pts',(3.29113505661424,0.841111005608376,-8.48080453303156));
#32189=CARTESIAN_POINT('Ctrl Pts',(3.27807398602321,0.83883055992351,-8.47026397611444));
#32190=CARTESIAN_POINT('Ctrl Pts',(3.26541716603687,0.83643339600023,-8.45893822789531));
#32191=CARTESIAN_POINT('Ctrl Pts',(3.25276034605054,0.83403623207695,-8.44761247967618));
#32192=CARTESIAN_POINT('Ctrl Pts',(3.24050695686514,0.831522216147609,-8.43550102903084));
#32193=CARTESIAN_POINT('Ctrl Pts',(3.22869302733891,0.828876288150112,-8.42249729172191));
#32194=CARTESIAN_POINT('Ctrl Pts',(3.21687909781269,0.826230360152616,-8.40949355441297));
#32195=CARTESIAN_POINT('Ctrl Pts',(3.20550581979188,0.823454018197384,-8.3956060278045));
#32196=CARTESIAN_POINT('Ctrl Pts',(3.19468036961139,0.820544747804952,-8.38078442938157));
#32197=CARTESIAN_POINT('Ctrl Pts',(3.18439707445734,0.817781178103046,-8.36670511917307));
#32198=CARTESIAN_POINT('Ctrl Pts',(3.17460781391463,0.814897544462127,-8.3517823765314));
#32199=CARTESIAN_POINT('Ctrl Pts',(3.1654515788303,0.811894466193472,-8.33597579569462));
#32200=CARTESIAN_POINT('Ctrl Pts',(3.16496884457052,0.811736138152337,-8.33514244246269));
#32201=CARTESIAN_POINT('Ctrl Pts',(3.16448788193827,0.811577479019006,-8.33430663436432));
#32202=CARTESIAN_POINT('Ctrl Pts',(3.164008715435,0.811418489210709,-8.33346836618398));
#32203=CARTESIAN_POINT('',(8.976377188873,1.060990939343,-8.586352585191));
#32204=CARTESIAN_POINT('',(8.976377188873,1.060990939343,-8.586352585191));
#32205=CARTESIAN_POINT('',(9.31255006972063,1.05006965735451,-8.45517202507966));
#32206=CARTESIAN_POINT('Ctrl Pts',(9.31255006975118,1.05006965736242,-8.45517202511191));
#32207=CARTESIAN_POINT('Ctrl Pts',(9.29074436206343,1.05275215314808,-8.4751756322404));
#32208=CARTESIAN_POINT('Ctrl Pts',(9.24411157801294,1.05729799350007,-8.51091803751234));
#32209=CARTESIAN_POINT('Ctrl Pts',(9.165072559821,1.061654875619,-8.551962189244));
#32210=CARTESIAN_POINT('Ctrl Pts',(9.076498905396,1.06329068312,-8.579231767789));
#32211=CARTESIAN_POINT('Ctrl Pts',(9.010839296144,1.062212801702,-8.586352781299));
#32212=CARTESIAN_POINT('Ctrl Pts',(8.976377188873,1.060990939343,-8.586352585191));
#32213=CARTESIAN_POINT('',(9.312550081826,1.050069655877,8.455172014035));
#32214=CARTESIAN_POINT('Ctrl Pts',(9.31255008182614,1.05006965587323,8.45517201403565));
#32215=CARTESIAN_POINT('Ctrl Pts',(9.49007071210251,1.02822813488135,8.29230332198047));
#32216=CARTESIAN_POINT('Ctrl Pts',(9.65651258488126,1.00678323034589,8.12919423308374));
#32217=CARTESIAN_POINT('Ctrl Pts',(9.81265533312651,0.985967919259792,7.96715327562526));
#32218=CARTESIAN_POINT('Ctrl Pts',(9.91037358013901,0.972941148992121,7.86574377383911));
#32219=CARTESIAN_POINT('Ctrl Pts',(10.0040580861799,0.960159921215438,7.76475277538954));
#32220=CARTESIAN_POINT('Ctrl Pts',(10.0938999473117,0.947671072743482,7.66450248813446));
#32221=CARTESIAN_POINT('Ctrl Pts',(10.3272989795294,0.915226451604224,7.40406353762623));
#32222=CARTESIAN_POINT('Ctrl Pts',(10.5347649834303,0.884750855204011,7.14862472245941));
#32223=CARTESIAN_POINT('Ctrl Pts',(10.7224474183718,0.856238063271469,6.89835151627484));
#32224=CARTESIAN_POINT('Ctrl Pts',(10.8811575891838,0.832126749501755,6.68671262041556));
#32225=CARTESIAN_POINT('Ctrl Pts',(11.0257204619308,0.809423428647549,6.47876703586414));
#32226=CARTESIAN_POINT('Ctrl Pts',(11.1579073453267,0.788181410825779,6.27570406781082));
#32227=CARTESIAN_POINT('Ctrl Pts',(11.1820378297224,0.784303717620428,6.23863527810894));
#32228=CARTESIAN_POINT('Ctrl Pts',(11.2057558983319,0.780474581389037,6.20172921156834));
#32229=CARTESIAN_POINT('Ctrl Pts',(11.2290723264035,0.776694143780084,6.16499312259368));
#32230=CARTESIAN_POINT('Ctrl Pts',(11.3801162342959,0.752204454868684,5.92701660138878));
#32231=CARTESIAN_POINT('Ctrl Pts',(11.5143056099425,0.729762942807907,5.6961725140216));
#32232=CARTESIAN_POINT('Ctrl Pts',(11.6344821728398,0.709301052844758,5.4738978660678));
#32233=CARTESIAN_POINT('Ctrl Pts',(11.7107469682605,0.696315810012572,5.3328409898791));
#32234=CARTESIAN_POINT('Ctrl Pts',(11.7813688975902,0.684121567187845,5.19523616882854));
#32235=CARTESIAN_POINT('Ctrl Pts',(11.8476896250997,0.672536043374578,5.05958779379219));
#32236=CARTESIAN_POINT('Ctrl Pts',(11.8858757940816,0.665865326892857,4.98148413049149));
#32237=CARTESIAN_POINT('Ctrl Pts',(11.922636015886,0.659397410760076,4.90402899576009));
#32238=CARTESIAN_POINT('Ctrl Pts',(11.9582263932854,0.653105260710028,4.82693636246589));
#32239=CARTESIAN_POINT('Ctrl Pts',(12.0138665013185,0.643268447106797,4.70641382917198));
#32240=CARTESIAN_POINT('Ctrl Pts',(12.0666476079204,0.633858069994158,4.58677779179511));
#32241=CARTESIAN_POINT('Ctrl Pts',(12.1173228696912,0.62473393238632,4.46626573472694));
#32242=CARTESIAN_POINT('Ctrl Pts',(12.1553590195886,0.617885481019554,4.37581105315446));
#32243=CARTESIAN_POINT('Ctrl Pts',(12.1922087795171,0.611199318424728,4.28486276143975));
#32244=CARTESIAN_POINT('Ctrl Pts',(12.228190632975,0.604635414006047,4.19267444498864));
#32245=CARTESIAN_POINT('Ctrl Pts',(12.3030650772989,0.590976620789059,4.00084027570298));
#32246=CARTESIAN_POINT('Ctrl Pts',(12.3741800556164,0.577857432420985,3.8036351343973));
#32247=CARTESIAN_POINT('Ctrl Pts',(12.4404245679778,0.565505899387503,3.60230507783802));
#32248=CARTESIAN_POINT('Ctrl Pts',(12.4484277147215,0.56401368323476,3.57798194631935));
#32249=CARTESIAN_POINT('Ctrl Pts',(12.4563597741263,0.562532608961203,3.5535986150842));
#32250=CARTESIAN_POINT('Ctrl Pts',(12.464218787137,0.561063026203705,3.52915728605649));
#32251=CARTESIAN_POINT('Ctrl Pts',(12.5124093904619,0.552051706382368,3.37928574489733));
#32252=CARTESIAN_POINT('Ctrl Pts',(12.5578532049559,0.543476675480936,3.22723289499543));
#32253=CARTESIAN_POINT('Ctrl Pts',(12.6001398201956,0.535458492472166,3.0744237536238));
#32254=CARTESIAN_POINT('Ctrl Pts',(12.621831189404,0.531345480185951,2.99603867869846));
#32255=CARTESIAN_POINT('Ctrl Pts',(12.6426918091358,0.527378158798193,2.91745465204444));
#32256=CARTESIAN_POINT('Ctrl Pts',(12.6626662843985,0.523567463387693,2.83886428776322));
#32257=CARTESIAN_POINT('Ctrl Pts',(12.7215803462743,0.512327941835709,2.60706457722144));
#32258=CARTESIAN_POINT('Ctrl Pts',(12.7727864647236,0.502444177432,2.3752102436452));
#32259=CARTESIAN_POINT('Ctrl Pts',(12.8167780306484,0.493907647680068,2.14242044261879));
#32260=CARTESIAN_POINT('Ctrl Pts',(12.8607695965732,0.485371117928113,1.90963064159175));
#32261=CARTESIAN_POINT('Ctrl Pts',(12.8975465474492,0.478183617519471,1.67590541472795));
#32262=CARTESIAN_POINT('Ctrl Pts',(12.9271424461252,0.472377045483412,1.44075450338083));
#32263=CARTESIAN_POINT('Ctrl Pts',(12.9567383448012,0.466570473447369,1.20560359203433));
#32264=CARTESIAN_POINT('Ctrl Pts',(12.9791530291776,0.462149468731758,0.96902683662872));
#32265=CARTESIAN_POINT('Ctrl Pts',(12.9942386480785,0.459169239074605,0.73151377154081));
#32266=CARTESIAN_POINT('Ctrl Pts',(13.0082305889908,0.456405070263105,0.511219941075852));
#32267=CARTESIAN_POINT('Ctrl Pts',(13.0159175203803,0.454882747634876,0.290120603906445));
#32268=CARTESIAN_POINT('Ctrl Pts',(13.0172425512059,0.4546204544462,0.0692015228525397));
#32269=CARTESIAN_POINT('Ctrl Pts',(13.017346122044,0.454599952337965,0.0519334156099304));
#32270=CARTESIAN_POINT('Ctrl Pts',(13.017410823298,0.454587122295236,0.0346664098812243));
#32271=CARTESIAN_POINT('Ctrl Pts',(13.0174366277985,0.454581959570064,0.0174009764857553));
#32272=CARTESIAN_POINT('Ctrl Pts',(13.0177440857389,0.454520446236328,-0.18831486759474));
#32273=CARTESIAN_POINT('Ctrl Pts',(13.0125295252215,0.455551756192601,-0.393807569883898));
#32274=CARTESIAN_POINT('Ctrl Pts',(13.0019394769544,0.45764683830302,-0.598013646668176));
#32275=CARTESIAN_POINT('Ctrl Pts',(13.0002697828882,0.457977162214662,-0.630210069772016));
#32276=CARTESIAN_POINT('Ctrl Pts',(12.9984664613338,0.458333824773382,-0.662374510521939));
#32277=CARTESIAN_POINT('Ctrl Pts',(12.9965300866001,0.458716594295993,-0.694502802839669));
#32278=CARTESIAN_POINT('Ctrl Pts',(12.9823122392856,0.461527082645403,-0.930405051873085));
#32279=CARTESIAN_POINT('Ctrl Pts',(12.9609214508078,0.465744725558995,-1.16435847740544));
#32280=CARTESIAN_POINT('Ctrl Pts',(12.9326414173885,0.471297941890548,-1.39637104020632));
#32281=CARTESIAN_POINT('Ctrl Pts',(12.9043613839692,0.476851158222116,-1.62838360300783));
#32282=CARTESIAN_POINT('Ctrl Pts',(12.869192221051,0.48373663979444,-1.85845528305323));
#32283=CARTESIAN_POINT('Ctrl Pts',(12.82705600053,0.491912777488324,-2.08731283346696));
#32284=CARTESIAN_POINT('Ctrl Pts',(12.7998529196691,0.497191279738091,-2.23506292525406));
#32285=CARTESIAN_POINT('Ctrl Pts',(12.7697455696918,0.503013587051361,-2.38230669762676));
#32286=CARTESIAN_POINT('Ctrl Pts',(12.7371408773064,0.509290643047791,-2.52753835000035));
#32287=CARTESIAN_POINT('Ctrl Pts',(12.7192425213279,0.512736434880241,-2.60726331053068));
#32288=CARTESIAN_POINT('Ctrl Pts',(12.7005916000993,0.516318323710831,-2.68638196014036));
#32289=CARTESIAN_POINT('Ctrl Pts',(12.6812554291551,0.520014935422878,-2.76464550962589));
#32290=CARTESIAN_POINT('Ctrl Pts',(12.648171622478,0.526339765069595,-2.89855289741836));
#32291=CARTESIAN_POINT('Ctrl Pts',(12.6130816730533,0.533003982417723,-3.02995702677085));
#32292=CARTESIAN_POINT('Ctrl Pts',(12.5769266936441,0.539847245472529,-3.15699014733577));
#32293=CARTESIAN_POINT('Ctrl Pts',(12.5534567855764,0.544289531359666,-3.23945335738117));
#32294=CARTESIAN_POINT('Ctrl Pts',(12.5295380821316,0.5488060716748,-3.32007471391683));
#32295=CARTESIAN_POINT('Ctrl Pts',(12.5054280206103,0.55334139293425,-3.39834398359222));
#32296=CARTESIAN_POINT('Ctrl Pts',(12.4687205620638,0.560246398837261,-3.51750858918807));
#32297=CARTESIAN_POINT('Ctrl Pts',(12.4315703607089,0.567188752539699,-3.63122182488701));
#32298=CARTESIAN_POINT('Ctrl Pts',(12.3938089815623,0.574190012215269,-3.74118823375633));
#32299=CARTESIAN_POINT('Ctrl Pts',(12.368560570584,0.578871268187638,-3.81471513207661));
#32300=CARTESIAN_POINT('Ctrl Pts',(12.3430389223144,0.583580059796604,-3.88656691042724));
#32301=CARTESIAN_POINT('Ctrl Pts',(12.3171936877466,0.588335665706033,-3.95725256130275));
#32302=CARTESIAN_POINT('Ctrl Pts',(12.2775531412705,0.595629653175207,-4.06566782143062));
#32303=CARTESIAN_POINT('Ctrl Pts',(12.2371513505869,0.603031170835373,-4.17133971598129));
#32304=CARTESIAN_POINT('Ctrl Pts',(12.1952061173948,0.610646478849638,-4.27627436264688));
#32305=CARTESIAN_POINT('Ctrl Pts',(12.1689021701395,0.615422055121253,-4.34207910852818));
#32306=CARTESIAN_POINT('Ctrl Pts',(12.1419912530875,0.620282768963302,-4.40759387782947));
#32307=CARTESIAN_POINT('Ctrl Pts',(12.1142804664268,0.625265210514748,-4.47331283655918));
#32308=CARTESIAN_POINT('Ctrl Pts',(12.0562410432107,0.635700787006872,-4.61095925222215));
#32309=CARTESIAN_POINT('Ctrl Pts',(11.994691828576,0.646677474596912,-4.7495001552316));
#32310=CARTESIAN_POINT('Ctrl Pts',(11.9300997334008,0.658068155383965,-4.88738150812178));
#32311=CARTESIAN_POINT('Ctrl Pts',(11.9146749410023,0.660788285237967,-4.92030800227241));
#32312=CARTESIAN_POINT('Ctrl Pts',(11.8990766225005,0.663531790474695,-4.95319690039001));
#32313=CARTESIAN_POINT('Ctrl Pts',(11.8833111363837,0.666296501523348,-4.98602707097243));
#32314=CARTESIAN_POINT('Ctrl Pts',(11.8071085671664,0.679659748523099,-5.14471189221277));
#32315=CARTESIAN_POINT('Ctrl Pts',(11.7270006317851,0.693522497860122,-5.30202462303339));
#32316=CARTESIAN_POINT('Ctrl Pts',(11.6438303021589,0.707707201862831,-5.45656047599039));
#32317=CARTESIAN_POINT('Ctrl Pts',(11.637738243609,0.708746202762382,-5.4678799148877));
#32318=CARTESIAN_POINT('Ctrl Pts',(11.6316297544981,0.709786908025164,-5.47918445706611));
#32319=CARTESIAN_POINT('Ctrl Pts',(11.6255051661099,0.71082923706868,-5.49047355140247));
#32320=CARTESIAN_POINT('Ctrl Pts',(11.5427080596109,0.724920278515558,-5.64308859861901));
#32321=CARTESIAN_POINT('Ctrl Pts',(11.456969029483,0.739303729464966,-5.79288102087204));
#32322=CARTESIAN_POINT('Ctrl Pts',(11.3675110472172,0.754054902312731,-5.94123279739961));
#32323=CARTESIAN_POINT('Ctrl Pts',(11.3600106655584,0.755291677650948,-5.95367098251773));
#32324=CARTESIAN_POINT('Ctrl Pts',(11.3524841412791,0.756531068057714,-5.96609903864255));
#32325=CARTESIAN_POINT('Ctrl Pts',(11.344931016417,0.757773134344475,-5.97851777921996));
#32326=CARTESIAN_POINT('Ctrl Pts',(11.2472908345613,0.773829479278541,-6.1390563788767));
#32327=CARTESIAN_POINT('Ctrl Pts',(11.1452052591543,0.790331519802546,-6.29803809444874));
#32328=CARTESIAN_POINT('Ctrl Pts',(11.0381645105898,0.807279061880735,-6.45590173342379));
#32329=CARTESIAN_POINT('Ctrl Pts',(10.9527885590251,0.820796461105002,-6.58181414132203));
#32330=CARTESIAN_POINT('Ctrl Pts',(10.8642604824445,0.834593931277089,-6.70701582823341));
#32331=CARTESIAN_POINT('Ctrl Pts',(10.7709807835768,0.848846921844718,-6.83319338638121));
#32332=CARTESIAN_POINT('Ctrl Pts',(10.7473103505908,0.852463726596192,-6.86521190134991));
#32333=CARTESIAN_POINT('Ctrl Pts',(10.7233339467609,0.856110123852281,-6.89729323502642));
#32334=CARTESIAN_POINT('Ctrl Pts',(10.6990254359918,0.859789513944065,-6.92946490307854));
#32335=CARTESIAN_POINT('Ctrl Pts',(10.5850549505516,0.877040339338839,-7.08030181201762));
#32336=CARTESIAN_POINT('Ctrl Pts',(10.463783904636,0.89501248721515,-7.23312447129108));
#32337=CARTESIAN_POINT('Ctrl Pts',(10.3326853170014,0.913883868715835,-7.38923986896025));
#32338=CARTESIAN_POINT('Ctrl Pts',(10.3256314894953,0.914899253185713,-7.39763973890598));
#32339=CARTESIAN_POINT('Ctrl Pts',(10.3185492109234,0.915917253547585,-7.4060491405237));
#32340=CARTESIAN_POINT('Ctrl Pts',(10.3114380876608,0.916937901851917,-7.41446827707697));
#32341=CARTESIAN_POINT('Ctrl Pts',(10.1793867030325,0.935891028781202,-7.57080906856405));
#32342=CARTESIAN_POINT('Ctrl Pts',(10.0373886982746,0.955753002911298,-7.73050708899526));
#32343=CARTESIAN_POINT('Ctrl Pts',(9.88185937375011,0.976697895521333,-7.89472729852672));
#32344=CARTESIAN_POINT('Ctrl Pts',(9.87335193950286,0.977843578480096,-7.9037101230772));
#32345=CARTESIAN_POINT('Ctrl Pts',(9.86480401851754,0.978992514653285,-7.9127064776283));
#32346=CARTESIAN_POINT('Ctrl Pts',(9.85621502410006,0.980144737119588,-7.92171655257824));
#32347=CARTESIAN_POINT('Ctrl Pts',(9.72378544070834,0.997910302419819,-8.06063857463946));
#32348=CARTESIAN_POINT('Ctrl Pts',(9.58159108396503,1.01646125094447,-8.20282124730524));
#32349=CARTESIAN_POINT('Ctrl Pts',(9.42910813639904,1.03558869639302,-8.34671638294721));
#32350=CARTESIAN_POINT('Ctrl Pts',(9.39090404965467,1.04038101315223,-8.38276882246198));
#32351=CARTESIAN_POINT('Ctrl Pts',(9.35205411094768,1.04520926624713,-8.41892879285433));
#32352=CARTESIAN_POINT('Ctrl Pts',(9.31255008182614,1.05006965587323,-8.45517201403564));
#32353=CARTESIAN_POINT('',(8.97637719778905,1.06099093965794,8.58635258519147));
#32354=CARTESIAN_POINT('Ctrl Pts',(8.97637719778914,1.06099093965548,8.58635258519167));
#32355=CARTESIAN_POINT('Ctrl Pts',(9.00588346338826,1.06203710363627,8.58635283430845));
#32356=CARTESIAN_POINT('Ctrl Pts',(9.03507097655644,1.0626130135361,8.58373842531847));
#32357=CARTESIAN_POINT('Ctrl Pts',(9.0639558049948,1.06272750014265,8.57854965874974));
#32358=CARTESIAN_POINT('Ctrl Pts',(9.09284063634256,1.06284198676072,8.57336089165838));
#32359=CARTESIAN_POINT('Ctrl Pts',(9.12142278435739,1.06249500887076,8.56559777366992));
#32360=CARTESIAN_POINT('Ctrl Pts',(9.14965453611679,1.06165426531512,8.55506327251998));
#32361=CARTESIAN_POINT('Ctrl Pts',(9.1778862878762,1.06081352175948,8.54452877137005));
#32362=CARTESIAN_POINT('Ctrl Pts',(9.20576764744961,1.05947889774048,8.53122290709537));
#32363=CARTESIAN_POINT('Ctrl Pts',(9.23305292402205,1.05757790867323,8.51473702651423));
#32364=CARTESIAN_POINT('Ctrl Pts',(9.26033820059449,1.05567691960598,8.4982511459331));
#32365=CARTESIAN_POINT('Ctrl Pts',(9.28702740061108,1.05320938365932,8.47858528069288));
#32366=CARTESIAN_POINT('Ctrl Pts',(9.31255008182614,1.05006965587323,8.45517201403565));
#32367=CARTESIAN_POINT('',(3.597021417327,0.8702239620615,8.586024047651));
#32368=CARTESIAN_POINT('Ctrl Pts',(3.470944033211,1.387996652244,8.999136656895));
#32369=CARTESIAN_POINT('Ctrl Pts',(3.506806407087,1.389267971531,8.999136656895));
#32370=CARTESIAN_POINT('Ctrl Pts',(4.139999211345,1.41171464956,8.999136656895));
#32371=CARTESIAN_POINT('Ctrl Pts',(5.370898212047,1.455350900996,8.999136656895));
#32372=CARTESIAN_POINT('Ctrl Pts',(7.164016762305,1.518920709268,8.999136656895));
#32373=CARTESIAN_POINT('Ctrl Pts',(8.39566724421,1.562587003558,8.999136656895));
#32374=CARTESIAN_POINT('Ctrl Pts',(9.029611555595,1.585063001874,8.999136656895));
#32375=CARTESIAN_POINT('Ctrl Pts',(9.065473930934,1.586334475758,8.999136656895));
#32376=CARTESIAN_POINT('Ctrl Pts',(3.480853549823,1.108461217464,9.015595309496));
#32377=CARTESIAN_POINT('Ctrl Pts',(3.516715931365,1.109732537023,9.015595309496));
#32378=CARTESIAN_POINT('Ctrl Pts',(4.149908870976,1.13217921985,9.015595309496));
#32379=CARTESIAN_POINT('Ctrl Pts',(5.380808135343,1.175815480634,9.015595309496));
#32380=CARTESIAN_POINT('Ctrl Pts',(7.173927071209,1.239385302576,9.015595309496));
#32381=CARTESIAN_POINT('Ctrl Pts',(8.405577819023,1.283051606293,9.015595309496));
#32382=CARTESIAN_POINT('Ctrl Pts',(9.03952226756,1.305527609472,9.015595309496));
#32383=CARTESIAN_POINT('Ctrl Pts',(9.075384650659,1.306799083631,9.015595309496));
#32384=CARTESIAN_POINT('Ctrl Pts',(3.488452624763,0.8941005377045,8.835315254871));
#32385=CARTESIAN_POINT('Ctrl Pts',(3.524315012182,0.8953718574718,8.835315254871));
#32386=CARTESIAN_POINT('Ctrl Pts',(4.157508055588,0.9178185439784,8.835315254871));
#32387=CARTESIAN_POINT('Ctrl Pts',(5.388407522147,0.9614548119297,8.835315254871));
#32388=CARTESIAN_POINT('Ctrl Pts',(7.181526753714,1.025024644355,8.835315254871));
#32389=CARTESIAN_POINT('Ctrl Pts',(8.413177705439,1.068690955302,8.835315254871));
#32390=CARTESIAN_POINT('Ctrl Pts',(9.047122259151,1.09116696221,8.835315254871));
#32391=CARTESIAN_POINT('Ctrl Pts',(9.0829846482,1.092438436579,8.835315254871));
#32392=CARTESIAN_POINT('Ctrl Pts',(3.489583140862,0.8622100508379,8.556943446236));
#32393=CARTESIAN_POINT('Ctrl Pts',(3.525445529156,0.8634813706362,8.556943446236));
#32394=CARTESIAN_POINT('Ctrl Pts',(4.158638588003,0.8859280576902,8.556943446236));
#32395=CARTESIAN_POINT('Ctrl Pts',(5.389538084642,0.9295643267078,8.556943446236));
#32396=CARTESIAN_POINT('Ctrl Pts',(7.182657360201,0.9931341606926,8.556943446236));
#32397=CARTESIAN_POINT('Ctrl Pts',(8.414308342262,1.036800472715,8.556943446236));
#32398=CARTESIAN_POINT('Ctrl Pts',(9.048252911621,1.059276480178,8.556943446236));
#32399=CARTESIAN_POINT('Ctrl Pts',(9.084115301555,1.060547954579,8.556943446236));
#32400=CARTESIAN_POINT('',(8.95892745008388,1.55316848628071,8.99999999999969));
#32401=CARTESIAN_POINT('',(3.579571669199,1.362459037518,9.));
#32402=CARTESIAN_POINT('Origin',(8.95892745079,1.553168486242,8.499999999999));
#32403=CARTESIAN_POINT('Origin',(3.002221399786,0.,9.));
#32404=CARTESIAN_POINT('',(8.958927440406,6.046831514125,9.));
#32405=CARTESIAN_POINT('',(8.958927440406,6.046831514125,9.));
#32406=CARTESIAN_POINT('',(8.958927440406,6.046831514125,9.));
#32407=CARTESIAN_POINT('Ctrl Pts',(9.065473909596,6.013665524999,8.999136656895));
#32408=CARTESIAN_POINT('Ctrl Pts',(9.02961154137,6.01493699863,8.999136656895));
#32409=CARTESIAN_POINT('Ctrl Pts',(8.3956669983,6.037413005161,8.999136656895));
#32410=CARTESIAN_POINT('Ctrl Pts',(7.164016284709,6.081079307665,8.999136656895));
#32411=CARTESIAN_POINT('Ctrl Pts',(5.370897734451,6.144649115935,8.999136656895));
#32412=CARTESIAN_POINT('Ctrl Pts',(4.139998972687,6.1882853589,8.999136656895));
#32413=CARTESIAN_POINT('Ctrl Pts',(3.506806407366,6.210732028459,8.999136656895));
#32414=CARTESIAN_POINT('Ctrl Pts',(3.470944033629,6.212003347741,8.999136656895));
#32415=CARTESIAN_POINT('Ctrl Pts',(9.07538462932,6.293200917125,9.015595309496));
#32416=CARTESIAN_POINT('Ctrl Pts',(9.039522253334,6.294472391032,9.015595309496));
#32417=CARTESIAN_POINT('Ctrl Pts',(8.405577573112,6.316948402425,9.015595309496));
#32418=CARTESIAN_POINT('Ctrl Pts',(7.173926593613,6.360614714356,9.015595309496));
#32419=CARTESIAN_POINT('Ctrl Pts',(5.380807657748,6.424184536297,9.015595309496));
#32420=CARTESIAN_POINT('Ctrl Pts',(4.149908632317,6.46782078861,9.015595309496));
#32421=CARTESIAN_POINT('Ctrl Pts',(3.516715931643,6.490267462967,9.015595309496));
#32422=CARTESIAN_POINT('Ctrl Pts',(3.480853550242,6.491538782521,9.015595309496));
#32423=CARTESIAN_POINT('Ctrl Pts',(9.082984626861,6.507561564177,8.835315254871));
#32424=CARTESIAN_POINT('Ctrl Pts',(9.047122244925,6.508833038295,8.835315254871));
#32425=CARTESIAN_POINT('Ctrl Pts',(8.413177459528,6.531309053417,8.835315254871));
#32426=CARTESIAN_POINT('Ctrl Pts',(7.181526276118,6.574975372577,8.835315254871));
#32427=CARTESIAN_POINT('Ctrl Pts',(5.388407044551,6.638545205002,8.835315254871));
#32428=CARTESIAN_POINT('Ctrl Pts',(4.157507816929,6.682181464482,8.835315254872));
#32429=CARTESIAN_POINT('Ctrl Pts',(3.524315012461,6.704628142518,8.835315254871));
#32430=CARTESIAN_POINT('Ctrl Pts',(3.488452625181,6.705899462281,8.835315254871));
#32431=CARTESIAN_POINT('Ctrl Pts',(9.084115280216,6.539452046178,8.556943446236));
#32432=CARTESIAN_POINT('Ctrl Pts',(9.048252897395,6.540723520327,8.556943446236));
#32433=CARTESIAN_POINT('Ctrl Pts',(8.414308096351,6.563199536004,8.556943446236));
#32434=CARTESIAN_POINT('Ctrl Pts',(7.182656882606,6.60686585624,8.556943446236));
#32435=CARTESIAN_POINT('Ctrl Pts',(5.389537607047,6.670435690223,8.556943446236));
#32436=CARTESIAN_POINT('Ctrl Pts',(4.158638349345,6.71407195077,8.556943446236));
#32437=CARTESIAN_POINT('Ctrl Pts',(3.525445529435,6.736518629354,8.556943446236));
#32438=CARTESIAN_POINT('Ctrl Pts',(3.489583141281,6.737789949147,8.556943446236));
#32439=CARTESIAN_POINT('',(8.976377188873,6.539009060657,8.586352585191));
#32440=CARTESIAN_POINT('Origin',(8.958927440522,6.046831514122,8.5));
#32441=CARTESIAN_POINT('',(8.976377188873,6.539009060657,8.586352585191));
#32442=CARTESIAN_POINT('Origin',(6.513075547481,-42.4,0.));
#32443=CARTESIAN_POINT('',(0.01744974833006,7.599368653176,-0.04689126965526));
#32444=CARTESIAN_POINT('Ctrl Pts',(0.01744974833006,7.599368653176,-0.04689126965526));
#32445=CARTESIAN_POINT('Ctrl Pts',(0.067537433307,7.597493189218,-0.1814388238612));
#32446=CARTESIAN_POINT('Ctrl Pts',(0.1639979857046,7.592799454319,-0.4404924525001));
#32447=CARTESIAN_POINT('Ctrl Pts',(0.2891401437734,7.583879367514,-0.8017214821274));
#32448=CARTESIAN_POINT('Ctrl Pts',(0.3899548010611,7.573764858792,-1.138584886082));
#32449=CARTESIAN_POINT('Ctrl Pts',(0.4632860851713,7.563044638479,-1.451600247463));
#32450=CARTESIAN_POINT('Ctrl Pts',(0.5076215437038,7.552188980092,-1.74099111528));
#32451=CARTESIAN_POINT('Ctrl Pts',(0.5174627880836,7.545233335246,-1.917359950681));
#32452=CARTESIAN_POINT('Ctrl Pts',(0.5174549507661,7.541860021273,-2.001305923414));
#32453=CARTESIAN_POINT('',(0.0174497466342403,7.59936861534601,0.0468912686245114));
#32454=CARTESIAN_POINT('Ctrl Pts',(0.0174497479590823,7.59936865318618,
0.0468912686587025));
#32455=CARTESIAN_POINT('Ctrl Pts',(0.0157883609905255,7.59943085569528,
0.0424282636034863));
#32456=CARTESIAN_POINT('Ctrl Pts',(0.0143880925278573,7.59948328325758,
0.0380261499363122));
#32457=CARTESIAN_POINT('Ctrl Pts',(0.013231809680605,7.59952657327597,0.0337070287048825));
#32458=CARTESIAN_POINT('Ctrl Pts',(0.0120755267436379,7.59956986329772,
0.0293879071383306));
#32459=CARTESIAN_POINT('Ctrl Pts',(0.0111632296353382,7.59960402079665,
0.0251517780061871));
#32460=CARTESIAN_POINT('Ctrl Pts',(0.0104662607819539,7.59963011599904,
0.0209620713759419));
#32461=CARTESIAN_POINT('Ctrl Pts',(0.00976929192856706,7.59965621120143,
0.0167723647456966));
#32462=CARTESIAN_POINT('Ctrl Pts',(0.00928765138822166,7.59967424577191,
0.0126290806250674));
#32463=CARTESIAN_POINT('Ctrl Pts',(0.00900722076910609,7.59968474284106,
0.00847390165808531));
#32464=CARTESIAN_POINT('Ctrl Pts',(0.00872679014999053,7.59969523991021,
0.00431872269110327));
#32465=CARTESIAN_POINT('Ctrl Pts',(0.00864756965336628,7.59969820524141,
0.000151648877503578));
#32466=CARTESIAN_POINT('Ctrl Pts',(0.00879065645843391,7.59969285107069,
-0.00415254496086243));
#32467=CARTESIAN_POINT('Ctrl Pts',(0.00893374326350403,7.59968749689997,
-0.00845673879921733));
#32468=CARTESIAN_POINT('Ctrl Pts',(0.00929913705893244,7.59967381431182,
-0.0128980526607187));
#32469=CARTESIAN_POINT('Ctrl Pts',(0.00993647955041976,7.59964995114117,
-0.0174909161469611));
#32470=CARTESIAN_POINT('Ctrl Pts',(0.0105738220419093,7.59962608797053,
-0.0220837796332035));
#32471=CARTESIAN_POINT('Ctrl Pts',(0.0114831132109058,7.59959204368608,
-0.0268281927446774));
#32472=CARTESIAN_POINT('Ctrl Pts',(0.012718653611351,7.59954578593001,-0.0317313795031946));
#32473=CARTESIAN_POINT('Ctrl Pts',(0.0139541940117949,7.59949952817393,
-0.0366345662617119));
#32474=CARTESIAN_POINT('Ctrl Pts',(0.0155159835261466,7.59944105358036,
-0.0416965266648994));
#32475=CARTESIAN_POINT('Ctrl Pts',(0.0174497483299296,7.59936865317228,
-0.0468912696552633));
#32476=CARTESIAN_POINT('Ctrl Pts',(0.5174542977566,7.541857836025,2.00131664892));
#32477=CARTESIAN_POINT('Ctrl Pts',(0.5174639416778,7.545246037484,1.917084695768));
#32478=CARTESIAN_POINT('Ctrl Pts',(0.5075557516817,7.552220151835,1.740184484561));
#32479=CARTESIAN_POINT('Ctrl Pts',(0.4629797196809,7.563104735101,1.449958596358));
#32480=CARTESIAN_POINT('Ctrl Pts',(0.3893196154358,7.573844231286,1.1361637114));
#32481=CARTESIAN_POINT('Ctrl Pts',(0.2880099327634,7.583976642822,0.798235513827));
#32482=CARTESIAN_POINT('Ctrl Pts',(0.1627480055576,7.592869536741,0.4370888248364));
#32483=CARTESIAN_POINT('Ctrl Pts',(0.06701238076274,7.597512638594,0.1800461148998));
#32484=CARTESIAN_POINT('Ctrl Pts',(0.01744974438142,7.599368539647,0.04689126959107));
#32485=CARTESIAN_POINT('',(9.31255006808369,6.54993034244276,8.45517202657257));
#32486=CARTESIAN_POINT('Ctrl Pts',(9.31255006811848,6.54993034243673,8.45517202660968));
#32487=CARTESIAN_POINT('Ctrl Pts',(9.29078297542864,6.54725259653745,8.47514021267117));
#32488=CARTESIAN_POINT('Ctrl Pts',(9.24421410184042,6.5427099915477,8.51085124868992));
#32489=CARTESIAN_POINT('Ctrl Pts',(9.165144091791,6.538346690073,8.551938784869));
#32490=CARTESIAN_POINT('Ctrl Pts',(9.076493701984,6.536708784041,8.579235860742));
#32491=CARTESIAN_POINT('Ctrl Pts',(9.010833592703,6.537787400757,8.586352779966));
#32492=CARTESIAN_POINT('Ctrl Pts',(8.976377188873,6.539009060657,8.586352585191));
#32493=CARTESIAN_POINT('',(9.312550081826,6.549930344123,-8.455172014035));
#32494=CARTESIAN_POINT('Ctrl Pts',(9.31255008182585,6.54993034411883,-8.45517201403428));
#32495=CARTESIAN_POINT('Ctrl Pts',(9.49006778755429,6.57177150512728,-8.29230600605519));
#32496=CARTESIAN_POINT('Ctrl Pts',(9.65650776248302,6.59321615075835,-8.12919896342003));
#32497=CARTESIAN_POINT('Ctrl Pts',(9.81264940133939,6.61403129349834,-7.96715940976441));
#32498=CARTESIAN_POINT('Ctrl Pts',(9.91032159555209,6.62705191169574,-7.86579785835051));
#32499=CARTESIAN_POINT('Ctrl Pts',(10.0039641012073,6.63982725131886,-7.76485417052757));
#32500=CARTESIAN_POINT('Ctrl Pts',(10.0937676900692,6.65231053633801,-7.6646501042644));
#32501=CARTESIAN_POINT('Ctrl Pts',(10.327133934128,6.68474996749384,-7.40425687410953));
#32502=CARTESIAN_POINT('Ctrl Pts',(10.5345775074028,6.71522144323954,-7.14885927793018));
#32503=CARTESIAN_POINT('Ctrl Pts',(10.7222455610682,6.74373128167272,-6.89862060649505));
#32504=CARTESIAN_POINT('Ctrl Pts',(10.8809434226423,6.76784007539014,-6.6870111116223));
#32505=CARTESIAN_POINT('Ctrl Pts',(11.0254997683209,6.79054170685715,-6.47909014035725));
#32506=CARTESIAN_POINT('Ctrl Pts',(11.1576842327289,6.81178273634758,-6.27604679436481));
#32507=CARTESIAN_POINT('Ctrl Pts',(11.1818144212986,6.81566027255665,-6.23898136274571));
#32508=CARTESIAN_POINT('Ctrl Pts',(11.2055323259985,6.81948927456683,-6.20207848992696));
#32509=CARTESIAN_POINT('Ctrl Pts',(11.2288487120883,6.82326959994322,-6.16534542921002));
#32510=CARTESIAN_POINT('Ctrl Pts',(11.3798915764977,6.84775843672311,-5.92738974054291));
#32511=CARTESIAN_POINT('Ctrl Pts',(11.5140851958374,6.87019999476148,-5.69655946408425));
#32512=CARTESIAN_POINT('Ctrl Pts',(11.6342642086962,6.89066182319112,-5.47430110068892));
#32513=CARTESIAN_POINT('Ctrl Pts',(11.7106680870889,6.90367044269832,-5.33300021491302));
#32514=CARTESIAN_POINT('Ctrl Pts',(11.7814080028223,6.9158851657,-5.19516484270745));
#32515=CARTESIAN_POINT('Ctrl Pts',(11.8478285723651,6.92748831032456,-5.059302800753));
#32516=CARTESIAN_POINT('Ctrl Pts',(11.8858838311325,6.93413626101579,-4.98146147540998));
#32517=CARTESIAN_POINT('Ctrl Pts',(11.9225212010676,6.94058246134619,-4.90426784694912));
#32518=CARTESIAN_POINT('Ctrl Pts',(11.9579935739301,6.94685356935787,-4.82744073960209));
#32519=CARTESIAN_POINT('Ctrl Pts',(12.0136308210525,6.95668959548248,-4.70693995512574));
#32520=CARTESIAN_POINT('Ctrl Pts',(12.0664022350456,6.96609804028853,-4.58734137006994));
#32521=CARTESIAN_POINT('Ctrl Pts',(12.1170636741229,6.97521944844119,-4.46688154635999));
#32522=CARTESIAN_POINT('Ctrl Pts',(12.1550776589322,6.98206372837619,-4.37649410391776));
#32523=CARTESIAN_POINT('Ctrl Pts',(12.1919036639809,6.98874536971883,-4.28562167942354));
#32524=CARTESIAN_POINT('Ctrl Pts',(12.2278610179747,6.99530451591579,-4.19351816197963));
#32525=CARTESIAN_POINT('Ctrl Pts',(12.3036863575555,7.00913616459135,-3.99929417964824));
#32526=CARTESIAN_POINT('Ctrl Pts',(12.3756475796478,7.02241272830797,-3.79959416133987));
#32527=CARTESIAN_POINT('Ctrl Pts',(12.4426100541845,7.03490158145942,-3.59565695221801));
#32528=CARTESIAN_POINT('Ctrl Pts',(12.4497213980101,7.03622788442778,-3.57399903675229));
#32529=CARTESIAN_POINT('Ctrl Pts',(12.4567763648866,7.03754535193983,-3.55229333798136));
#32530=CARTESIAN_POINT('Ctrl Pts',(12.4637735958284,7.03885374058288,-3.5305413429469));
#32531=CARTESIAN_POINT('Ctrl Pts',(12.5119042445602,7.0478535284571,-3.38091963674243));
#32532=CARTESIAN_POINT('Ctrl Pts',(12.557302921659,7.05641954217032,-3.22910687206369));
#32533=CARTESIAN_POINT('Ctrl Pts',(12.5995564877654,7.06443093497975,-3.07653040949109));
#32534=CARTESIAN_POINT('Ctrl Pts',(12.6212883256478,7.06855135145082,-2.99805734189386));
#32535=CARTESIAN_POINT('Ctrl Pts',(12.6421882040919,7.07252589140287,-2.9193823077654));
#32536=CARTESIAN_POINT('Ctrl Pts',(12.6621999153949,7.07634349842331,-2.84069977527412));
#32537=CARTESIAN_POINT('Ctrl Pts',(12.7211207226989,7.08758374090974,-2.60903351420746));
#32538=CARTESIAN_POINT('Ctrl Pts',(12.7723429523916,7.09747019371598,-2.37730275152345));
#32539=CARTESIAN_POINT('Ctrl Pts',(12.8163549825881,7.10601028713707,-2.14465728986177));
#32540=CARTESIAN_POINT('Ctrl Pts',(12.8603670127847,7.11455038055818,-1.91201182819948));
#32541=CARTESIAN_POINT('Ctrl Pts',(12.897168786403,7.12174247559519,-1.67845171591279));
#32542=CARTESIAN_POINT('Ctrl Pts',(12.9267985558583,7.12755549034134,-1.44348407101859));
#32543=CARTESIAN_POINT('Ctrl Pts',(12.9564283253135,7.13336850508748,-1.20851642612503));
#32544=CARTESIAN_POINT('Ctrl Pts',(12.9788859304009,7.13779785482601,-0.972141090669652));
#32545=CARTESIAN_POINT('Ctrl Pts',(12.9940272207165,7.14078900135936,-0.734834418582472));
#32546=CARTESIAN_POINT('Ctrl Pts',(13.0081495807623,7.14357885925213,-0.513497254138357));
#32547=CARTESIAN_POINT('Ctrl Pts',(13.0159070855893,7.14511512893504,-0.291349846503961));
#32548=CARTESIAN_POINT('Ctrl Pts',(13.0172415248565,7.14537934085419,-0.0693735202517211));
#32549=CARTESIAN_POINT('Ctrl Pts',(13.0173378048379,7.14539840378144,-0.0533578969940196));
#32550=CARTESIAN_POINT('Ctrl Pts',(13.0174006486339,7.14541086733759,-0.0373431644940472));
#32551=CARTESIAN_POINT('Ctrl Pts',(13.0174300343815,7.14541673509063,-0.0213296913672406));
#32552=CARTESIAN_POINT('Ctrl Pts',(13.0178083424561,7.1454922757367,0.18482556027766));
#32553=CARTESIAN_POINT('Ctrl Pts',(13.0126413842003,7.14447031469605,0.390772161360061));
#32554=CARTESIAN_POINT('Ctrl Pts',(13.002072435279,7.14237940736248,0.595449151127796));
#32555=CARTESIAN_POINT('Ctrl Pts',(13.0004419032247,7.14205683115785,0.627025838182427));
#32556=CARTESIAN_POINT('Ctrl Pts',(12.9986827984263,7.14170891390931,0.658572308601473));
#32557=CARTESIAN_POINT('Ctrl Pts',(12.9967956469798,7.14133587053571,0.690084668584461));
#32558=CARTESIAN_POINT('Ctrl Pts',(12.98267616487,7.13854479658696,0.925857056562666));
#32559=CARTESIAN_POINT('Ctrl Pts',(12.96138904957,7.13434741615559,1.15972000730305));
#32560=CARTESIAN_POINT('Ctrl Pts',(12.9332147976316,7.12881461129494,1.39166038958121));
#32561=CARTESIAN_POINT('Ctrl Pts',(12.9050405456931,7.12328180643427,1.62360077185999));
#32562=CARTESIAN_POINT('Ctrl Pts',(12.8699792798543,7.11641709407502,1.85361857379828));
#32563=CARTESIAN_POINT('Ctrl Pts',(12.8279470458181,7.10826026606875,2.0824641655611));
#32564=CARTESIAN_POINT('Ctrl Pts',(12.8007150614312,7.10297559305513,2.23072941304998));
#32565=CARTESIAN_POINT('Ctrl Pts',(12.7705565767191,7.09714263522302,2.37850234504309));
#32566=CARTESIAN_POINT('Ctrl Pts',(12.7378726221699,7.0908498865513,2.5242836001386));
#32567=CARTESIAN_POINT('Ctrl Pts',(12.7201092935788,7.08742985479754,2.60351392499996));
#32568=CARTESIAN_POINT('Ctrl Pts',(12.7015999944259,7.08387493863183,2.68215598443196));
#32569=CARTESIAN_POINT('Ctrl Pts',(12.6824091040699,7.08020576750035,2.75996937505813));
#32570=CARTESIAN_POINT('Ctrl Pts',(12.6495024648307,7.0739142360242,2.89339607521678));
#32571=CARTESIAN_POINT('Ctrl Pts',(12.6145916946915,7.06728319522948,3.0243863246274));
#32572=CARTESIAN_POINT('Ctrl Pts',(12.5786086920348,7.06047129381164,3.15107197859204));
#32573=CARTESIAN_POINT('Ctrl Pts',(12.5549949651851,7.05600100596649,3.2342090212963));
#32574=CARTESIAN_POINT('Ctrl Pts',(12.5309194709636,7.05145403211695,3.31549230343964));
#32575=CARTESIAN_POINT('Ctrl Pts',(12.5066455815884,7.04688726462086,3.39439455486266));
#32576=CARTESIAN_POINT('Ctrl Pts',(12.4698582463404,7.03996628033685,3.51397174869596));
#32577=CARTESIAN_POINT('Ctrl Pts',(12.4326160731218,7.03300607735472,3.62808101585939));
#32578=CARTESIAN_POINT('Ctrl Pts',(12.3947586326729,7.02598632415325,3.73841820624057));
#32579=CARTESIAN_POINT('Ctrl Pts',(12.36957114144,7.02131590877062,3.81182826731294));
#32580=CARTESIAN_POINT('Ctrl Pts',(12.3441112978653,7.01661793652144,3.88356855430558));
#32581=CARTESIAN_POINT('Ctrl Pts',(12.3183318538247,7.01187380074364,3.95413799035498));
#32582=CARTESIAN_POINT('Ctrl Pts',(12.2787528679277,7.00459016488451,4.06248271298572));
#32583=CARTESIAN_POINT('Ctrl Pts',(12.2384205239071,6.99720034784702,4.16806748038133));
#32584=CARTESIAN_POINT('Ctrl Pts',(12.1965545931921,6.98959831045675,4.27289989604193));
#32585=CARTESIAN_POINT('Ctrl Pts',(12.1701654562908,6.9848065573058,4.33897837372818));
#32586=CARTESIAN_POINT('Ctrl Pts',(12.143167010936,6.97992941935173,4.40475788634172));
#32587=CARTESIAN_POINT('Ctrl Pts',(12.1153638613582,6.9749297741696,4.4707406291853));
#32588=CARTESIAN_POINT('Ctrl Pts',(12.057108107269,6.96445405092651,4.6089938306964));
#32589=CARTESIAN_POINT('Ctrl Pts',(11.9953185701516,6.95343331477605,4.74813799939895));
#32590=CARTESIAN_POINT('Ctrl Pts',(11.9304543037742,6.94199424071378,4.88662589555805));
#32591=CARTESIAN_POINT('Ctrl Pts',(11.9152484660004,6.93931263011078,4.91909098921037));
#32592=CARTESIAN_POINT('Ctrl Pts',(11.8998736555181,6.93660825499467,4.95152003275441));
#32593=CARTESIAN_POINT('Ctrl Pts',(11.8843357862834,6.93388316062605,4.98389312313398));
#32594=CARTESIAN_POINT('Ctrl Pts',(11.8086189668404,6.9206036385013,5.14164882322728));
#32595=CARTESIAN_POINT('Ctrl Pts',(11.7290301761305,6.90682801104577,5.29807576163209));
#32596=CARTESIAN_POINT('Ctrl Pts',(11.6464112725892,6.89273303439849,5.4517622729065));
#32597=CARTESIAN_POINT('Ctrl Pts',(11.6397533860299,6.89159718350298,5.46414717894979));
#32598=CARTESIAN_POINT('Ctrl Pts',(11.6330758218434,6.89045928657576,5.47651429096273));
#32599=CARTESIAN_POINT('Ctrl Pts',(11.6263790205946,6.88931945061147,5.48886287145605));
#32600=CARTESIAN_POINT('Ctrl Pts',(11.5435350300419,6.87521890374586,5.64162321893096));
#32601=CARTESIAN_POINT('Ctrl Pts',(11.4577474733856,6.8608259726941,5.79154821698368));
#32602=CARTESIAN_POINT('Ctrl Pts',(11.3682432763548,6.846065870727,5.94001812062533));
#32603=CARTESIAN_POINT('Ctrl Pts',(11.3607295496616,6.84482678501008,5.95248191914141));
#32604=CARTESIAN_POINT('Ctrl Pts',(11.3531896306147,6.84358508150389,5.96493546126059));
#32605=CARTESIAN_POINT('Ctrl Pts',(11.3456230618551,6.84234069947685,5.97737956249348));
#32606=CARTESIAN_POINT('Ctrl Pts',(11.2479228365551,6.82627312535388,6.13805893153611));
#32607=CARTESIAN_POINT('Ctrl Pts',(11.1457793596027,6.80976046367597,6.29716413816969));
#32608=CARTESIAN_POINT('Ctrl Pts',(11.0386838093546,6.79280313264702,6.45513601625609));
#32609=CARTESIAN_POINT('Ctrl Pts',(10.95324778463,6.77927533480954,6.58115889256326));
#32610=CARTESIAN_POINT('Ctrl Pts',(10.8646603995461,6.76546788162356,6.70646106814643));
#32611=CARTESIAN_POINT('Ctrl Pts',(10.7713246513584,6.7512056589261,6.83272795168484));
#32612=CARTESIAN_POINT('Ctrl Pts',(10.7476624078654,6.74758993619637,6.86473881356154));
#32613=CARTESIAN_POINT('Ctrl Pts',(10.723694981797,6.74394472515823,6.89681165784147));
#32614=CARTESIAN_POINT('Ctrl Pts',(10.6993963518299,6.74026664072237,6.92897390289576));
#32615=CARTESIAN_POINT('Ctrl Pts',(10.5856732127626,6.72305236533453,7.07950055694885));
#32616=CARTESIAN_POINT('Ctrl Pts',(10.4646950372019,6.70512194294707,7.23198551458773));
#32617=CARTESIAN_POINT('Ctrl Pts',(10.33394473404,6.68629743059677,7.38773991203805));
#32618=CARTESIAN_POINT('Ctrl Pts',(10.3265618155478,6.68523448973181,7.39653470633959));
#32619=CARTESIAN_POINT('Ctrl Pts',(10.319147739752,6.68416868431552,7.40533992386218));
#32620=CARTESIAN_POINT('Ctrl Pts',(10.3117020534887,6.68309997728696,7.41415580027921));
#32621=CARTESIAN_POINT('Ctrl Pts',(10.1797693680289,6.66416318848558,7.57036735812084));
#32622=CARTESIAN_POINT('Ctrl Pts',(10.0379117757277,6.64431961626695,7.72992583955895));
#32623=CARTESIAN_POINT('Ctrl Pts',(9.88255009909747,6.6233951338071,7.89399787690877));
#32624=CARTESIAN_POINT('Ctrl Pts',(9.87386552973313,6.62222547521898,7.90316934711957));
#32625=CARTESIAN_POINT('Ctrl Pts',(9.86513876411273,6.62105242549219,7.9123549200861));
#32626=CARTESIAN_POINT('Ctrl Pts',(9.85636917706876,6.61987594930949,7.92155479929637));
#32627=CARTESIAN_POINT('Ctrl Pts',(9.72396192532252,6.60211297172393,8.06045879973815));
#32628=CARTESIAN_POINT('Ctrl Pts',(9.58179259770183,6.5835647569172,8.20262298986108));
#32629=CARTESIAN_POINT('Ctrl Pts',(9.42933843780151,6.56444019510331,8.3464990344189));
#32630=CARTESIAN_POINT('Ctrl Pts',(9.39106011623076,6.55963838367691,8.38262355541271));
#32631=CARTESIAN_POINT('Ctrl Pts',(9.35213342239554,6.554800491868,8.41885602797014));
#32632=CARTESIAN_POINT('Ctrl Pts',(9.31255008182585,6.54993034411883,8.45517201403428));
#32633=CARTESIAN_POINT('',(8.9763771992842,6.53900906028642,-8.58635258519104));
#32634=CARTESIAN_POINT('Ctrl Pts',(8.9763771992841,6.53900906028359,-8.58635258519028));
#32635=CARTESIAN_POINT('Ctrl Pts',(9.00583001265153,6.53796479114675,-8.58635283579333));
#32636=CARTESIAN_POINT('Ctrl Pts',(9.03498268830907,6.53738830563828,-8.5837487457709));
#32637=CARTESIAN_POINT('Ctrl Pts',(9.06385871107003,6.53727288613592,-8.57856709206617));
#32638=CARTESIAN_POINT('Ctrl Pts',(9.09273473723344,6.53715746661995,-8.57338543775088));
#32639=CARTESIAN_POINT('Ctrl Pts',(9.12133411192538,6.53750315525565,-8.56562622650716));
#32640=CARTESIAN_POINT('Ctrl Pts',(9.14958717399502,6.53834372961078,-8.55508840261447));
#32641=CARTESIAN_POINT('Ctrl Pts',(9.17784023606467,6.53918430396591,-8.54455057872178));
#32642=CARTESIAN_POINT('Ctrl Pts',(9.20574698943828,6.54051987479979,-8.5312341615105));
#32643=CARTESIAN_POINT('Ctrl Pts',(9.23304466248228,6.54242151574695,-8.51474201807231));
#32644=CARTESIAN_POINT('Ctrl Pts',(9.26034233552627,6.54432315669411,-8.49824987463412));
#32645=CARTESIAN_POINT('Ctrl Pts',(9.2870309347497,6.54679105138876,-8.47858203692904));
#32646=CARTESIAN_POINT('Ctrl Pts',(9.31255008182585,6.54993034411882,-8.45517201403432));
#32647=CARTESIAN_POINT('',(3.597021417327,6.729776037938,-8.586024047651));
#32648=CARTESIAN_POINT('',(3.597021417327,6.729776037938,-8.586024047651));
#32649=CARTESIAN_POINT('Ctrl Pts',(3.16400873497919,6.78858150430047,-8.33346840037428));
#32650=CARTESIAN_POINT('Ctrl Pts',(3.18245003661732,6.78246267353839,-8.3657297019323));
#32651=CARTESIAN_POINT('Ctrl Pts',(3.20356756071657,6.77677099112735,-8.39472009582055));
#32652=CARTESIAN_POINT('Ctrl Pts',(3.22736110799477,6.77142291886836,-8.42102585955313));
#32653=CARTESIAN_POINT('Ctrl Pts',(3.25115466367853,6.76607484472005,-8.44733163257876));
#32654=CARTESIAN_POINT('Ctrl Pts',(3.27762421818746,6.76106964013681,-8.4709526470973));
#32655=CARTESIAN_POINT('Ctrl Pts',(3.30517534476285,6.75662306506702,-8.49104256326221));
#32656=CARTESIAN_POINT('Ctrl Pts',(3.33272647133824,6.75217648999722,-8.51113247942711));
#32657=CARTESIAN_POINT('Ctrl Pts',(3.36135919392955,6.74828922022634,-8.52769141414516));
#32658=CARTESIAN_POINT('Ctrl Pts',(3.39171144247602,6.7448188976879,-8.54146863707291));
#32659=CARTESIAN_POINT('Ctrl Pts',(3.42206369102248,6.74134857514947,-8.55524586000065));
#32660=CARTESIAN_POINT('Ctrl Pts',(3.45413545171913,6.73829481040069,-8.56624130320908));
#32661=CARTESIAN_POINT('Ctrl Pts',(3.48830827981827,6.73574096876752,-8.57393475975479));
#32662=CARTESIAN_POINT('Ctrl Pts',(3.52248110791741,6.73318712713436,-8.5816282163005));
#32663=CARTESIAN_POINT('Ctrl Pts',(3.55875500812843,6.73113334144666,-8.58601970949189));
#32664=CARTESIAN_POINT('Ctrl Pts',(3.59702141732687,6.72977603793439,-8.58602404765039));
#32665=CARTESIAN_POINT('Ctrl Pts',(2.697976245788,6.271708668204,-8.470478867963));
#32666=CARTESIAN_POINT('Ctrl Pts',(2.702496487236,6.270109776492,-8.478862059423));
#32667=CARTESIAN_POINT('Ctrl Pts',(2.741553495773,6.256704437972,-8.548825392175));
#32668=CARTESIAN_POINT('Ctrl Pts',(2.830094460866,6.232525054952,-8.670029259093));
#32669=CARTESIAN_POINT('Ctrl Pts',(2.985002282807,6.202729543589,-8.80802165731));
#32670=CARTESIAN_POINT('Ctrl Pts',(3.162329083555,6.1782271165,-8.910329310933));
#32671=CARTESIAN_POINT('Ctrl Pts',(3.360770749574,6.15933536047,-8.97640494805));
#32672=CARTESIAN_POINT('Ctrl Pts',(3.512848176858,6.150922384735,-8.993154038482));
#32673=CARTESIAN_POINT('Ctrl Pts',(3.596210811008,6.148187398446,-8.991916537819));
#32674=CARTESIAN_POINT('Ctrl Pts',(3.60609432629,6.147889718194,-8.991622140839));
#32675=CARTESIAN_POINT('Ctrl Pts',(2.707229788595,6.575168830057,-8.522615175531));
#32676=CARTESIAN_POINT('Ctrl Pts',(2.711757591597,6.573562734905,-8.531038953485));
#32677=CARTESIAN_POINT('Ctrl Pts',(2.750879945687,6.560097135082,-8.601341018487));
#32678=CARTESIAN_POINT('Ctrl Pts',(2.839569240021,6.535811141223,-8.72313186267));
#32679=CARTESIAN_POINT('Ctrl Pts',(2.99473765246,6.505889438864,-8.861792775667));
#32680=CARTESIAN_POINT('Ctrl Pts',(3.172364230425,6.481288731968,-8.96459655693));
#32681=CARTESIAN_POINT('Ctrl Pts',(3.371142968843,6.462327820356,-9.030993747717));
#32682=CARTESIAN_POINT('Ctrl Pts',(3.523479741901,6.453890770661,-9.047826127655));
#32683=CARTESIAN_POINT('Ctrl Pts',(3.606984714449,6.45115151872,-9.04658424048));
#32684=CARTESIAN_POINT('Ctrl Pts',(3.616885107666,6.450853459245,-9.046288614332));
#32685=CARTESIAN_POINT('Ctrl Pts',(2.911986675828,6.79469121972,-8.453506164382));
#32686=CARTESIAN_POINT('Ctrl Pts',(2.915517531542,6.793439346699,-8.460099530006));
#32687=CARTESIAN_POINT('Ctrl Pts',(2.94602445157,6.782944985081,-8.515123261411));
#32688=CARTESIAN_POINT('Ctrl Pts',(3.01515739146,6.764040432135,-8.610408211832));
#32689=CARTESIAN_POINT('Ctrl Pts',(3.135968450588,6.740798929991,-8.71876429852));
#32690=CARTESIAN_POINT('Ctrl Pts',(3.274071132333,6.721726401897,-8.798989801913));
#32691=CARTESIAN_POINT('Ctrl Pts',(3.428408819964,6.707046179747,-8.850734065253));
#32692=CARTESIAN_POINT('Ctrl Pts',(3.546552349393,6.700515345316,-8.863834484004));
#32693=CARTESIAN_POINT('Ctrl Pts',(3.61129082548,6.69839105866,-8.862870569862));
#32694=CARTESIAN_POINT('Ctrl Pts',(3.618965960468,6.698159820195,-8.862640873848));
#32695=CARTESIAN_POINT('Ctrl Pts',(3.182848670484,6.791546387898,-8.306825990365));
#32696=CARTESIAN_POINT('Ctrl Pts',(3.185008101237,6.790786308233,-8.310874692875));
#32697=CARTESIAN_POINT('Ctrl Pts',(3.203663420435,6.78441697955,-8.3446583261));
#32698=CARTESIAN_POINT('Ctrl Pts',(3.245894163072,6.772981061909,-8.403095186004));
#32699=CARTESIAN_POINT('Ctrl Pts',(3.319442410588,6.759004529431,-8.469324554359));
#32700=CARTESIAN_POINT('Ctrl Pts',(3.403175058521,6.747593048858,-8.518165951076));
#32701=CARTESIAN_POINT('Ctrl Pts',(3.496378554812,6.738838135146,-8.549542875217));
#32702=CARTESIAN_POINT('Ctrl Pts',(3.567485025904,6.734939152711,-8.557454533639));
#32703=CARTESIAN_POINT('Ctrl Pts',(3.606407852607,6.73366042859,-8.556875284136));
#32704=CARTESIAN_POINT('Ctrl Pts',(3.611021868203,6.733520983139,-8.556737012325));
#32705=CARTESIAN_POINT('',(3.579571669165,6.237540962482,-9.));
#32706=CARTESIAN_POINT('Ctrl Pts',(2.71354627856836,6.29590662785209,-8.50000002316856));
#32707=CARTESIAN_POINT('Ctrl Pts',(2.73271290696036,6.29276428740895,-8.53319622314795));
#32708=CARTESIAN_POINT('Ctrl Pts',(2.75362612200078,6.28969051942418,-8.56499171230839));
#32709=CARTESIAN_POINT('Ctrl Pts',(2.77608265061947,6.28670679356586,-8.59530196526257));
#32710=CARTESIAN_POINT('Ctrl Pts',(2.79626205372542,6.28402562196204,-8.62253871333666));
#32711=CARTESIAN_POINT('Ctrl Pts',(2.81768872536269,6.28141700629083,-8.6485766786427));
#32712=CARTESIAN_POINT('Ctrl Pts',(2.84025088394378,6.27889495274492,-8.67335338184266));
#32713=CARTESIAN_POINT('Ctrl Pts',(2.86150654311113,6.27651894291496,-8.6966953487301));
#32714=CARTESIAN_POINT('Ctrl Pts',(2.88377798700089,6.27421759335609,-8.718917609257));
#32715=CARTESIAN_POINT('Ctrl Pts',(2.90682907414929,6.2720086472179,-8.73987654658258));
#32716=CARTESIAN_POINT('Ctrl Pts',(2.92978054743643,6.26980924690515,-8.76074491114422));
#32717=CARTESIAN_POINT('Ctrl Pts',(2.95350429207167,6.26770154421663,-8.78036053410902));
#32718=CARTESIAN_POINT('Ctrl Pts',(2.97774532818122,6.26569567525515,-8.79862777462662));
#32719=CARTESIAN_POINT('Ctrl Pts',(2.98375967268792,6.26519800729594,-8.80315998509664));
#32720=CARTESIAN_POINT('Ctrl Pts',(2.98980578037816,6.26470656868169,-8.80760942851375));
#32721=CARTESIAN_POINT('Ctrl Pts',(2.99587961765459,6.26422143436467,-8.81197511614055));
#32722=CARTESIAN_POINT('Ctrl Pts',(3.01681927685196,6.26254892540517,-8.82702589983905));
#32723=CARTESIAN_POINT('Ctrl Pts',(3.03808451837945,6.2609566002826,-8.84108390682663));
#32724=CARTESIAN_POINT('Ctrl Pts',(3.05971475546151,6.25943353078172,-8.85424559056032));
#32725=CARTESIAN_POINT('Ctrl Pts',(3.08155208208703,6.257895879297,-8.86753328526029));
#32726=CARTESIAN_POINT('Ctrl Pts',(3.10376200877344,6.25642872123841,-8.87990776329837));
#32727=CARTESIAN_POINT('Ctrl Pts',(3.12641871308661,6.25502659177109,-8.89142795734024));
#32728=CARTESIAN_POINT('Ctrl Pts',(3.14041770081031,6.25416025247793,-8.89854598530838));
#32729=CARTESIAN_POINT('Ctrl Pts',(3.15458787574177,6.25331885754533,-8.9053370665679));
#32730=CARTESIAN_POINT('Ctrl Pts',(3.16895165114764,6.25250245441483,-8.91180655896024));
#32731=CARTESIAN_POINT('Ctrl Pts',(3.19352199871603,6.2511059337853,-8.92287312552643));
#32732=CARTESIAN_POINT('Ctrl Pts',(3.21864368964397,6.24978257411292,-8.93299444910136));
#32733=CARTESIAN_POINT('Ctrl Pts',(3.24439464561042,6.24852951272045,-8.94215563455501));
#32734=CARTESIAN_POINT('Ctrl Pts',(3.26942731660678,6.24731140362901,-8.95106128224036));
#32735=CARTESIAN_POINT('Ctrl Pts',(3.2950552167543,6.2461596666439,-8.95905977553184));
#32736=CARTESIAN_POINT('Ctrl Pts',(3.32135908871198,6.24507988147401,-8.96609031402971));
#32737=CARTESIAN_POINT('Ctrl Pts',(3.33477496679961,6.24452915395285,-8.96967613012286));
#32738=CARTESIAN_POINT('Ctrl Pts',(3.34836678575868,6.24399728208548,-8.97300936790168));
#32739=CARTESIAN_POINT('Ctrl Pts',(3.36214547754614,6.24348595006784,-8.97607676506084));
#32740=CARTESIAN_POINT('Ctrl Pts',(3.39643763297189,6.24221335631991,-8.9837108468559));
#32741=CARTESIAN_POINT('Ctrl Pts',(3.43188068992917,6.24106093218739,-8.98969329898011));
#32742=CARTESIAN_POINT('Ctrl Pts',(3.46821448374441,6.24005961143774,-8.99376551635245));
#32743=CARTESIAN_POINT('Ctrl Pts',(3.50454827755965,6.23905829068809,-8.99783773372479));
#32744=CARTESIAN_POINT('Ctrl Pts',(3.54177264129656,6.23820808731495,-8.99999965435044));
#32745=CARTESIAN_POINT('Ctrl Pts',(3.579571669165,6.237540962482,-9.00000000000001));
#32746=CARTESIAN_POINT('Origin',(3.579571668976,6.237540962483,-8.5));
#32747=CARTESIAN_POINT('Origin',(3.579571668976,17.50736,-8.));
#32748=CARTESIAN_POINT('',(3.57957168029041,1.36245903804411,-9.00000000000025));
#32749=CARTESIAN_POINT('',(3.579571669165,6.237540962482,-9.));
#32750=CARTESIAN_POINT('Ctrl Pts',(3.57957166916,1.362459037518,-9.));
#32751=CARTESIAN_POINT('Ctrl Pts',(3.53067956146749,1.36159569723168,-9.000000000009));
#32752=CARTESIAN_POINT('Ctrl Pts',(3.48229116327313,1.36042549044103,-8.99641626892138));
#32753=CARTESIAN_POINT('Ctrl Pts',(3.43474696375249,1.35897335420425,-8.9894573284164));
#32754=CARTESIAN_POINT('Ctrl Pts',(3.41174502962636,1.35827080915359,-8.98609058562344));
#32755=CARTESIAN_POINT('Ctrl Pts',(3.38893988987502,1.35750227471969,-8.98193347499698));
#32756=CARTESIAN_POINT('Ctrl Pts',(3.36636648175544,1.35667057477884,-8.97700744528496));
#32757=CARTESIAN_POINT('Ctrl Pts',(3.3375005477531,1.35560703153914,-8.97070824368423));
#32758=CARTESIAN_POINT('Ctrl Pts',(3.309008416789,1.35444019861569,-8.96314601327225));
#32759=CARTESIAN_POINT('Ctrl Pts',(3.28110543490607,1.35318521002559,-8.95442019421223));
#32760=CARTESIAN_POINT('Ctrl Pts',(3.25302206326135,1.35192210806991,-8.94563796367519));
#32761=CARTESIAN_POINT('Ctrl Pts',(3.22553607665365,1.35056970692941,-8.93567739095572));
#32762=CARTESIAN_POINT('Ctrl Pts',(3.19884192411574,1.34914343604218,-8.92468635838248));
#32763=CARTESIAN_POINT('Ctrl Pts',(3.18844693309194,1.34858803076946,-8.92040633170701));
#32764=CARTESIAN_POINT('Ctrl Pts',(3.17817170134369,1.34802142383197,-8.91597051268099));
#32765=CARTESIAN_POINT('Ctrl Pts',(3.16802641451614,1.3474445263465,-8.91138932599168));
#32766=CARTESIAN_POINT('Ctrl Pts',(3.14307589340737,1.34602575000893,-8.90012271548201));
#32767=CARTESIAN_POINT('Ctrl Pts',(3.11891002670089,1.34454473374312,-8.88798168376388));
#32768=CARTESIAN_POINT('Ctrl Pts',(3.09542161957199,1.3430008971863,-8.87498498824957));
#32769=CARTESIAN_POINT('Ctrl Pts',(3.07167229857546,1.34143991138795,-8.86184392287337));
#32770=CARTESIAN_POINT('Ctrl Pts',(3.04861489058827,1.33981470190665,-8.84782773667852));
#32771=CARTESIAN_POINT('Ctrl Pts',(3.02615772706361,1.3381246688236,-8.83290636262246));
#32772=CARTESIAN_POINT('Ctrl Pts',(3.0155596267221,1.33732709970161,-8.82586459088199));
#32773=CARTESIAN_POINT('Ctrl Pts',(3.0050955469187,1.3365150934981,-8.81862054492759));
#32774=CARTESIAN_POINT('Ctrl Pts',(2.99475796750508,1.33568858715917,-8.81116763654123));
#32775=CARTESIAN_POINT('Ctrl Pts',(2.97315509353913,1.33396140214249,-8.79559298080138));
#32776=CARTESIAN_POINT('Ctrl Pts',(2.9521153696349,1.33217089472038,-8.77911803949023));
#32777=CARTESIAN_POINT('Ctrl Pts',(2.93158843147111,1.33030591798024,-8.76165459620007));
#32778=CARTESIAN_POINT('Ctrl Pts',(2.9114806336299,1.32847902227031,-8.74454773961541));
#32779=CARTESIAN_POINT('Ctrl Pts',(2.89186441996441,1.32658066737695,-8.72649182314979));
#32780=CARTESIAN_POINT('Ctrl Pts',(2.87273094267328,1.32460037536748,-8.70737273600263));
#32781=CARTESIAN_POINT('Ctrl Pts',(2.86265638108103,1.32355767029529,-8.69730575141217));
#32782=CARTESIAN_POINT('Ctrl Pts',(2.85271634578784,1.32249224852657,-8.68694352705419));
#32783=CARTESIAN_POINT('Ctrl Pts',(2.84291467409078,1.32140258048075,-8.67626656865963));
#32784=CARTESIAN_POINT('Ctrl Pts',(2.82156544990445,1.3190291519353,-8.65301086438402));
#32785=CARTESIAN_POINT('Ctrl Pts',(2.80087871271009,1.316540693963,-8.62826131105066));
#32786=CARTESIAN_POINT('Ctrl Pts',(2.7811381471473,1.31395624459894,-8.60208297702246));
#32787=CARTESIAN_POINT('Ctrl Pts',(2.76162204893333,1.3114011826653,-8.57620231335314));
#32788=CARTESIAN_POINT('Ctrl Pts',(2.7430313720079,1.30875229993928,-8.5489252917344));
#32789=CARTESIAN_POINT('Ctrl Pts',(2.72562719938734,1.30602799237575,-8.5203641444786));
#32790=CARTESIAN_POINT('Ctrl Pts',(2.72153358428764,1.30538721117796,-8.51364631041545));
#32791=CARTESIAN_POINT('Ctrl Pts',(2.71750552908601,1.30474225723723,-8.50685764623042));
#32792=CARTESIAN_POINT('Ctrl Pts',(2.71354626504425,1.304093369931,-8.49999999974485));
#32793=CARTESIAN_POINT('Ctrl Pts',(3.606118439109,1.452111117783,-8.991622013561));
#32794=CARTESIAN_POINT('Ctrl Pts',(3.596226549993,1.451813160933,-8.991916534875));
#32795=CARTESIAN_POINT('Ctrl Pts',(3.514295435264,1.449125030121,-8.993132242195));
#32796=CARTESIAN_POINT('Ctrl Pts',(3.361902292376,1.440755734761,-8.976686868883));
#32797=CARTESIAN_POINT('Ctrl Pts',(3.162806797501,1.421866077181,-8.91075977445));
#32798=CARTESIAN_POINT('Ctrl Pts',(2.985508542217,1.397316177247,-8.80817459468));
#32799=CARTESIAN_POINT('Ctrl Pts',(2.83073332976,1.367610099334,-8.670666976124));
#32800=CARTESIAN_POINT('Ctrl Pts',(2.742180934874,1.343511145381,-8.549950688678));
#32801=CARTESIAN_POINT('Ctrl Pts',(2.702500790941,1.329891627237,-8.478869336066));
#32802=CARTESIAN_POINT('Ctrl Pts',(2.697982963143,1.328293519144,-8.470490213466));
#32803=CARTESIAN_POINT('Ctrl Pts',(3.616909261623,1.149147376315,-9.046288487242));
#32804=CARTESIAN_POINT('Ctrl Pts',(3.607000480323,1.148849039803,-9.046584238161));
#32805=CARTESIAN_POINT('Ctrl Pts',(3.524929471719,1.146156716061,-9.047804254029));
#32806=CARTESIAN_POINT('Ctrl Pts',(3.372276437766,1.137763587628,-9.031277044035));
#32807=CARTESIAN_POINT('Ctrl Pts',(3.172842746773,1.118804854858,-8.965029105095));
#32808=CARTESIAN_POINT('Ctrl Pts',(2.995244772122,1.094156444364,-8.861946457188));
#32809=CARTESIAN_POINT('Ctrl Pts',(2.840209180296,1.064324590375,-8.723772668877));
#32810=CARTESIAN_POINT('Ctrl Pts',(2.75150843471,1.040119415609,-8.602471763629));
#32811=CARTESIAN_POINT('Ctrl Pts',(2.711761902532,1.026438673235,-8.531046265659));
#32812=CARTESIAN_POINT('Ctrl Pts',(2.707236517197,1.024833365209,-8.522626576234));
#32813=CARTESIAN_POINT('Ctrl Pts',(3.618984699362,0.9018408279155,-8.862640775326));
#32814=CARTESIAN_POINT('Ctrl Pts',(3.611303055056,0.9016093738728,-8.86287056766));
#32815=CARTESIAN_POINT('Ctrl Pts',(3.547676246624,0.8995214772279,-8.863817500059));
#32816=CARTESIAN_POINT('Ctrl Pts',(3.429288349975,0.8930245062433,-8.850954493995));
#32817=CARTESIAN_POINT('Ctrl Pts',(3.274443865634,0.8783462364203,-8.799327648757));
#32818=CARTESIAN_POINT('Ctrl Pts',(3.136362160075,0.8592365357768,-8.718883846345));
#32819=CARTESIAN_POINT('Ctrl Pts',(3.015656085662,0.8360650174749,-8.610909097964));
#32820=CARTESIAN_POINT('Ctrl Pts',(2.946514523875,0.8172237841081,-8.516008288557));
#32821=CARTESIAN_POINT('Ctrl Pts',(2.915520898728,0.8065617493812,-8.460105247678));
#32822=CARTESIAN_POINT('Ctrl Pts',(2.911991930924,0.8053104895109,-8.453515076827));
#32823=CARTESIAN_POINT('Ctrl Pts',(3.611033157925,0.8664794103834,-8.55673695376));
#32824=CARTESIAN_POINT('Ctrl Pts',(3.606415217474,0.8663398338715,-8.556875282532));
#32825=CARTESIAN_POINT('Ctrl Pts',(3.568160699697,0.8650830103777,-8.557444317374));
#32826=CARTESIAN_POINT('Ctrl Pts',(3.496908759876,0.8612038910007,-8.549675924183));
#32827=CARTESIAN_POINT('Ctrl Pts',(3.403402273431,0.852450539314,-8.518372159072));
#32828=CARTESIAN_POINT('Ctrl Pts',(3.319680109389,0.8410165238057,-8.469396662616));
#32829=CARTESIAN_POINT('Ctrl Pts',(3.24619855465,0.8270823847512,-8.403401567405));
#32830=CARTESIAN_POINT('Ctrl Pts',(3.203963082135,0.8156854566047,-8.345201753149));
#32831=CARTESIAN_POINT('Ctrl Pts',(3.18501016893,0.8092143577992,-8.310878194086));
#32832=CARTESIAN_POINT('Ctrl Pts',(3.182851897331,0.8084546497716,-8.306831443972));
#32833=CARTESIAN_POINT('Origin',(3.579571686039,1.362459038122,-8.500000000001));
#32834=CARTESIAN_POINT('Origin',(3.146558966941,1.304093369921,-8.249999999753));
#32835=CARTESIAN_POINT('Ctrl Pts',(2.737554087051,1.34152810419,-8.539856081031));
#32836=CARTESIAN_POINT('Ctrl Pts',(2.729007055677,1.338703332081,-8.525052188437));
#32837=CARTESIAN_POINT('Ctrl Pts',(2.499808905038,1.26314158189,-8.128069346529));
#32838=CARTESIAN_POINT('Ctrl Pts',(2.046877238873,1.123743738896,-7.343568688376));
#32839=CARTESIAN_POINT('Ctrl Pts',(1.352547748218,0.9392672044454,-6.140954733368));
#32840=CARTESIAN_POINT('Ctrl Pts',(0.7051558095594,0.7959101378268,-5.0196390032));
#32841=CARTESIAN_POINT('Ctrl Pts',(0.2815322151021,0.7187111648313,-4.285901414315));
#32842=CARTESIAN_POINT('Ctrl Pts',(0.1075907271497,0.6897998149103,-3.984625919637));
#32843=CARTESIAN_POINT('Ctrl Pts',(2.747286251397,1.027333500649,-8.594189576059));
#32844=CARTESIAN_POINT('Ctrl Pts',(2.738697483667,1.024494934782,-8.579313393976));
#32845=CARTESIAN_POINT('Ctrl Pts',(2.508380197487,0.9485642294144,-8.18039215245));
#32846=CARTESIAN_POINT('Ctrl Pts',(2.053240695369,0.8084869567693,-7.392067410251));
#32847=CARTESIAN_POINT('Ctrl Pts',(1.355536410545,0.6231138684716,-6.183608140278));
#32848=CARTESIAN_POINT('Ctrl Pts',(0.7050060546966,0.4790619292973,-5.056856512082));
#32849=CARTESIAN_POINT('Ctrl Pts',(0.2793327299031,0.4014894447593,-4.319568686113));
#32850=CARTESIAN_POINT('Ctrl Pts',(0.1045501668528,0.3724382976097,-4.016836406632));
#32851=CARTESIAN_POINT('Ctrl Pts',(2.960318350366,0.8038948754913,-8.513830393669));
#32852=CARTESIAN_POINT('Ctrl Pts',(2.951699901941,0.8010465002312,-8.498902803114));
#32853=CARTESIAN_POINT('Ctrl Pts',(2.720586745609,0.7248534134077,-8.09860307405));
#32854=CARTESIAN_POINT('Ctrl Pts',(2.263877147047,0.5842929662415,-7.307558845036));
#32855=CARTESIAN_POINT('Ctrl Pts',(1.563772886664,0.3982822961497,-6.094942695458));
#32856=CARTESIAN_POINT('Ctrl Pts',(0.9110106540926,0.2537362002753,-4.964325343381));
#32857=CARTESIAN_POINT('Ctrl Pts',(0.4838796692276,0.1758980940347,-4.224512776108));
#32858=CARTESIAN_POINT('Ctrl Pts',(0.3084989779427,0.1467475304718,-3.920744508136));
#32859=CARTESIAN_POINT('Ctrl Pts',(3.23490900795,0.819877609831,-8.352245692761));
#32860=CARTESIAN_POINT('Ctrl Pts',(3.226292682607,0.8170299362443,-8.337321779493));
#32861=CARTESIAN_POINT('Ctrl Pts',(2.995236455471,0.7408556177653,-7.937120654688));
#32862=CARTESIAN_POINT('Ctrl Pts',(2.538639167099,0.6003297324392,-7.146270952629));
#32863=CARTESIAN_POINT('Ctrl Pts',(1.838706578788,0.4143646690566,-5.933952147802));
#32864=CARTESIAN_POINT('Ctrl Pts',(1.186103994052,0.2698539205859,-4.803611313887));
#32865=CARTESIAN_POINT('Ctrl Pts',(0.759077276717,0.1920348144671,-4.063979343274));
#32866=CARTESIAN_POINT('Ctrl Pts',(0.5837393699985,0.1628913622357,-3.760285180345));
#32867=CARTESIAN_POINT('Ctrl Pts',(9.065473909596,1.586334475001,-8.999136656895));
#32868=CARTESIAN_POINT('Ctrl Pts',(9.02961154137,1.58506300137,-8.999136656895));
#32869=CARTESIAN_POINT('Ctrl Pts',(8.395666997776,1.562586994821,-8.999136656895));
#32870=CARTESIAN_POINT('Ctrl Pts',(7.164016283661,1.518920692298,-8.999136656895));
#32871=CARTESIAN_POINT('Ctrl Pts',(5.370897733403,1.455350884028,-8.999136656895));
#32872=CARTESIAN_POINT('Ctrl Pts',(4.139998972163,1.411714641081,-8.999136656895));
#32873=CARTESIAN_POINT('Ctrl Pts',(3.506806407366,1.389267971541,-8.999136656895));
#32874=CARTESIAN_POINT('Ctrl Pts',(3.470944033629,1.387996652259,-8.999136656895));
#32875=CARTESIAN_POINT('Ctrl Pts',(9.07538462932,1.306799082875,-9.015595309496));
#32876=CARTESIAN_POINT('Ctrl Pts',(9.039522253334,1.305527608968,-9.015595309496));
#32877=CARTESIAN_POINT('Ctrl Pts',(8.405577572588,1.283051597556,-9.015595309496));
#32878=CARTESIAN_POINT('Ctrl Pts',(7.173926592565,1.239385285606,-9.015595309496));
#32879=CARTESIAN_POINT('Ctrl Pts',(5.380807656699,1.175815463665,-9.015595309496));
#32880=CARTESIAN_POINT('Ctrl Pts',(4.149908631793,1.132179211371,-9.015595309496));
#32881=CARTESIAN_POINT('Ctrl Pts',(3.516715931643,1.109732537033,-9.015595309496));
#32882=CARTESIAN_POINT('Ctrl Pts',(3.480853550242,1.108461217479,-9.015595309496));
#32883=CARTESIAN_POINT('Ctrl Pts',(9.082984626861,1.092438435823,-8.835315254872));
#32884=CARTESIAN_POINT('Ctrl Pts',(9.047122244925,1.091166961705,-8.835315254872));
#32885=CARTESIAN_POINT('Ctrl Pts',(8.413177459004,1.068690946564,-8.835315254872));
#32886=CARTESIAN_POINT('Ctrl Pts',(7.18152627507,1.025024627385,-8.835315254871));
#32887=CARTESIAN_POINT('Ctrl Pts',(5.388407043503,0.9614547949613,-8.835315254871));
#32888=CARTESIAN_POINT('Ctrl Pts',(4.157507816405,0.9178185354994,-8.835315254872));
#32889=CARTESIAN_POINT('Ctrl Pts',(3.524315012461,0.8953718574817,-8.835315254872));
#32890=CARTESIAN_POINT('Ctrl Pts',(3.488452625181,0.8941005377194,-8.835315254872));
#32891=CARTESIAN_POINT('Ctrl Pts',(9.084115280216,1.060547953822,-8.556943446236));
#32892=CARTESIAN_POINT('Ctrl Pts',(9.048252897395,1.059276479673,-8.556943446236));
#32893=CARTESIAN_POINT('Ctrl Pts',(8.414308095827,1.036800463978,-8.556943446236));
#32894=CARTESIAN_POINT('Ctrl Pts',(7.182656881557,0.9931341437232,-8.556943446236));
#32895=CARTESIAN_POINT('Ctrl Pts',(5.389537605998,0.9295643097394,-8.556943446236));
#32896=CARTESIAN_POINT('Ctrl Pts',(4.158638348821,0.8859280492112,-8.556943446236));
#32897=CARTESIAN_POINT('Ctrl Pts',(3.525445529435,0.8634813706461,-8.556943446236));
#32898=CARTESIAN_POINT('Ctrl Pts',(3.489583141281,0.8622100508528,-8.556943446236));
#32899=CARTESIAN_POINT('',(8.95892744039,1.553168485875,-9.));
#32900=CARTESIAN_POINT('',(8.95892744039,1.553168485875,-9.));
#32901=CARTESIAN_POINT('Origin',(8.958927440522,1.553168485878,-8.5));
#32902=CARTESIAN_POINT('Origin',(9.335521399786,0.,-9.));
#32903=CARTESIAN_POINT('',(8.9589274516891,6.04683151365134,-8.99999999999974));
#32904=CARTESIAN_POINT('',(3.579571669165,6.237540962482,-9.));
#32905=CARTESIAN_POINT('',(8.958927440394,6.046831514125,-9.));
#32906=CARTESIAN_POINT('Ctrl Pts',(3.470944033141,6.212003347758,-8.999136656895));
#32907=CARTESIAN_POINT('Ctrl Pts',(3.50680640704,6.21073202847,-8.999136656895));
#32908=CARTESIAN_POINT('Ctrl Pts',(4.139999211807,6.188285350424,-8.999136656895));
#32909=CARTESIAN_POINT('Ctrl Pts',(5.370898213018,6.144649098969,-8.999136656895));
#32910=CARTESIAN_POINT('Ctrl Pts',(7.164016763276,6.081079290698,-8.999136656895));
#32911=CARTESIAN_POINT('Ctrl Pts',(8.395667245888,6.037412996383,-8.999136656895));
#32912=CARTESIAN_POINT('Ctrl Pts',(9.029611557979,6.014936998041,-8.999136656895));
#32913=CARTESIAN_POINT('Ctrl Pts',(9.06547393451,6.013665524115,-8.999136656895));
#32914=CARTESIAN_POINT('Ctrl Pts',(3.480853549753,6.491538782538,-9.015595309496));
#32915=CARTESIAN_POINT('Ctrl Pts',(3.516715931318,6.490267462978,-9.015595309496));
#32916=CARTESIAN_POINT('Ctrl Pts',(4.149908871438,6.467820780133,-9.015595309496));
#32917=CARTESIAN_POINT('Ctrl Pts',(5.380808136314,6.424184519332,-9.015595309496));
#32918=CARTESIAN_POINT('Ctrl Pts',(7.17392707218,6.36061469739,-9.015595309496));
#32919=CARTESIAN_POINT('Ctrl Pts',(8.4055778207,6.316948393647,-9.015595309496));
#32920=CARTESIAN_POINT('Ctrl Pts',(9.039522269944,6.294472390443,-9.015595309496));
#32921=CARTESIAN_POINT('Ctrl Pts',(9.075384654235,6.293200916242,-9.015595309496));
#32922=CARTESIAN_POINT('Ctrl Pts',(3.488452624693,6.705899462298,-8.835315254871));
#32923=CARTESIAN_POINT('Ctrl Pts',(3.524315012135,6.70462814253,-8.835315254871));
#32924=CARTESIAN_POINT('Ctrl Pts',(4.15750805605,6.682181456005,-8.835315254872));
#32925=CARTESIAN_POINT('Ctrl Pts',(5.388407523118,6.638545188036,-8.835315254871));
#32926=CARTESIAN_POINT('Ctrl Pts',(7.181526754685,6.574975355611,-8.835315254871));
#32927=CARTESIAN_POINT('Ctrl Pts',(8.413177707116,6.531309044639,-8.835315254872));
#32928=CARTESIAN_POINT('Ctrl Pts',(9.047122261535,6.508833037706,-8.835315254871));
#32929=CARTESIAN_POINT('Ctrl Pts',(9.082984651776,6.507561563294,-8.835315254871));
#32930=CARTESIAN_POINT('Ctrl Pts',(3.489583140792,6.737789949165,-8.556943446236));
#32931=CARTESIAN_POINT('Ctrl Pts',(3.525445529109,6.736518629365,-8.556943446236));
#32932=CARTESIAN_POINT('Ctrl Pts',(4.158638588465,6.714071942293,-8.556943446236));
#32933=CARTESIAN_POINT('Ctrl Pts',(5.389538085613,6.670435673258,-8.556943446236));
#32934=CARTESIAN_POINT('Ctrl Pts',(7.182657361173,6.606865839273,-8.556943446236));
#32935=CARTESIAN_POINT('Ctrl Pts',(8.414308343939,6.563199527226,-8.556943446236));
#32936=CARTESIAN_POINT('Ctrl Pts',(9.048252914005,6.540723519738,-8.556943446236));
#32937=CARTESIAN_POINT('Ctrl Pts',(9.084115305131,6.539452045294,-8.556943446236));
#32938=CARTESIAN_POINT('Origin',(8.958927452512,6.046831513697,-8.499999999999));
#32939=CARTESIAN_POINT('Ctrl Pts',(8.927938928541,6.006828531619,-8.997867591216));
#32940=CARTESIAN_POINT('Ctrl Pts',(8.937774429904,6.00642695855,-8.998158451035));
#32941=CARTESIAN_POINT('Ctrl Pts',(9.006435353586,6.003807560836,-8.99917072319));
#32942=CARTESIAN_POINT('Ctrl Pts',(9.134996901011,6.001289846702,-8.987861041925));
#32943=CARTESIAN_POINT('Ctrl Pts',(9.310154709202,6.003639088283,-8.940357378065));
#32944=CARTESIAN_POINT('Ctrl Pts',(9.480463368067,6.012209681015,-8.858861787215));
#32945=CARTESIAN_POINT('Ctrl Pts',(9.591730727664,6.022942085977,-8.776282372617));
#32946=CARTESIAN_POINT('Ctrl Pts',(9.646942429761,6.030093692078,-8.724650169732));
#32947=CARTESIAN_POINT('Ctrl Pts',(9.653937673143,6.031033325521,-8.717912229442));
#32948=CARTESIAN_POINT('Ctrl Pts',(8.938791953801,6.291076248276,-9.02137079219));
#32949=CARTESIAN_POINT('Ctrl Pts',(8.948369630768,6.290685072941,-9.021655027771));
#32950=CARTESIAN_POINT('Ctrl Pts',(9.015230406025,6.28813382963,-9.022644820733));
#32951=CARTESIAN_POINT('Ctrl Pts',(9.140418016028,6.285686148486,-9.011601251901));
#32952=CARTESIAN_POINT('Ctrl Pts',(9.310978373003,6.287991261734,-8.965209492321));
#32953=CARTESIAN_POINT('Ctrl Pts',(9.476823523468,6.29636809076,-8.885616148791));
#32954=CARTESIAN_POINT('Ctrl Pts',(9.585183697085,6.306852394716,-8.804956031936));
#32955=CARTESIAN_POINT('Ctrl Pts',(9.638956172709,6.313838355042,-8.75451988478));
#32956=CARTESIAN_POINT('Ctrl Pts',(9.645769129904,6.31475622189,-8.747937965196));
#32957=CARTESIAN_POINT('Ctrl Pts',(8.953058757155,6.511404577949,-8.840488172299));
#32958=CARTESIAN_POINT('Ctrl Pts',(8.960489665714,6.511101332867,-8.840709539929));
#32959=CARTESIAN_POINT('Ctrl Pts',(9.01236154992,6.509123086244,-8.841480762696));
#32960=CARTESIAN_POINT('Ctrl Pts',(9.109456153971,6.507217777614,-8.83288514462));
#32961=CARTESIAN_POINT('Ctrl Pts',(9.241735947841,6.508976141369,-8.796775018666));
#32962=CARTESIAN_POINT('Ctrl Pts',(9.370415806732,6.515429682801,-8.734796114743));
#32963=CARTESIAN_POINT('Ctrl Pts',(9.454569368652,6.523533628542,-8.671929757642));
#32964=CARTESIAN_POINT('Ctrl Pts',(9.496358160883,6.528943855231,-8.632590750232));
#32965=CARTESIAN_POINT('Ctrl Pts',(9.501653316682,6.529654845007,-8.627456542266));
#32966=CARTESIAN_POINT('Ctrl Pts',(8.962706207688,6.543754453392,-8.557068318775));
#32967=CARTESIAN_POINT('Ctrl Pts',(8.967310172969,6.543567160675,-8.557205973457));
#32968=CARTESIAN_POINT('Ctrl Pts',(8.999444136385,6.542344118915,-8.55768560415));
#32969=CARTESIAN_POINT('Ctrl Pts',(9.059544841125,6.541148131598,-8.552341420912));
#32970=CARTESIAN_POINT('Ctrl Pts',(9.141415387249,6.542164979948,-8.529893434732));
#32971=CARTESIAN_POINT('Ctrl Pts',(9.2211546288,6.546048644919,-8.491323096556));
#32972=CARTESIAN_POINT('Ctrl Pts',(9.273432037729,6.550980270515,-8.45210592626));
#32973=CARTESIAN_POINT('Ctrl Pts',(9.299440276694,6.554291915423,-8.427516736843));
#32974=CARTESIAN_POINT('Ctrl Pts',(9.302736736018,6.554727402792,-8.424306776346));
#32975=CARTESIAN_POINT('',(9.631273226501,6.057526622699,-8.740237221487));
#32976=CARTESIAN_POINT('Ctrl Pts',(8.95892745169395,6.04683151392516,-8.99999999999995));
#32977=CARTESIAN_POINT('Ctrl Pts',(9.00313304379479,6.04604972402664,-8.99999898867999));
#32978=CARTESIAN_POINT('Ctrl Pts',(9.04760587323135,6.0455202798527,-8.99704958523495));
#32979=CARTESIAN_POINT('Ctrl Pts',(9.0917825090689,6.04525525204683,-8.99113201402888));
#32980=CARTESIAN_POINT('Ctrl Pts',(9.10585477641443,6.04517082863913,-8.98924699851176));
#32981=CARTESIAN_POINT('Ctrl Pts',(9.1198968933399,6.04511317331886,-8.98706118387352));
#32982=CARTESIAN_POINT('Ctrl Pts',(9.13389048489755,6.04508249896408,-8.98457500125824));
#32983=CARTESIAN_POINT('Ctrl Pts',(9.1628521082268,6.04501901425359,-8.97942951132918));
#32984=CARTESIAN_POINT('Ctrl Pts',(9.19160465322972,6.04507401878512,-8.97300230786102));
#32985=CARTESIAN_POINT('Ctrl Pts',(9.22017512254227,6.04524499188232,-8.96526941126628));
#32986=CARTESIAN_POINT('Ctrl Pts',(9.24874559185483,6.04541596497953,-8.95753651467154));
#32987=CARTESIAN_POINT('Ctrl Pts',(9.27713482025089,6.04570290954913,-8.94849779093512));
#32988=CARTESIAN_POINT('Ctrl Pts',(9.30534741011489,6.04611300830617,-8.93807953003303));
#32989=CARTESIAN_POINT('Ctrl Pts',(9.33355999997888,6.04652310706321,-8.92766126913094));
#32990=CARTESIAN_POINT('Ctrl Pts',(9.36158834110619,6.0470562702359,-8.91586640524687));
#32991=CARTESIAN_POINT('Ctrl Pts',(9.38941945465935,6.04772000825609,-8.9025928143899));
#32992=CARTESIAN_POINT('Ctrl Pts',(9.41506316740826,6.04833157944233,-8.89036246829066));
#32993=CARTESIAN_POINT('Ctrl Pts',(9.44053971294124,6.04905411615378,-8.87687607922135));
#32994=CARTESIAN_POINT('Ctrl Pts',(9.46580248313527,6.04990050739418,-8.86202001340548));
#32995=CARTESIAN_POINT('Ctrl Pts',(9.46795738965685,6.04997270430647,-8.86075279556414));
#32996=CARTESIAN_POINT('Ctrl Pts',(9.47011071559531,6.05004580639459,-8.85947559313687));
#32997=CARTESIAN_POINT('Ctrl Pts',(9.4722624174361,6.050119823895,-8.85818832518149));
#32998=CARTESIAN_POINT('Ctrl Pts',(9.50110713898193,6.05111206833537,-8.84093180523811));
#32999=CARTESIAN_POINT('Ctrl Pts',(9.52965700600334,6.05226429513786,-8.82186747223183));
#33000=CARTESIAN_POINT('Ctrl Pts',(9.55761457757172,6.05358096894265,-8.8009715755454));
#33001=CARTESIAN_POINT('Ctrl Pts',(9.58272679945829,6.05476363978576,-8.78220233470397));
#33002=CARTESIAN_POINT('Ctrl Pts',(9.60736070239246,6.05607893807379,-8.76195568320717));
#33003=CARTESIAN_POINT('Ctrl Pts',(9.63127322650134,6.057526622699,-8.74023722148736));
#33004=CARTESIAN_POINT('Origin',(9.295100333699,6.057526622722,-8.370118610573));
#33005=CARTESIAN_POINT('Origin',(8.958927440522,17.50736,-8.));
#33006=CARTESIAN_POINT('',(9.63127321029653,1.54247337967211,-8.74023723620533));
#33007=CARTESIAN_POINT('',(9.631273226501,6.057526622699,-8.740237221487));
#33008=CARTESIAN_POINT('Ctrl Pts',(9.63127321025096,1.54247337828569,-8.74023723624765));
#33009=CARTESIAN_POINT('Ctrl Pts',(9.6057200390174,1.54402189862992,-8.76344677737955));
#33010=CARTESIAN_POINT('Ctrl Pts',(9.5788416935493,1.54544836517941,-8.78543940428296));
#33011=CARTESIAN_POINT('Ctrl Pts',(9.55081894029273,1.54673721047252,-8.80601765024047));
#33012=CARTESIAN_POINT('Ctrl Pts',(9.53152029367347,1.54762480954714,-8.82018943033437));
#33013=CARTESIAN_POINT('Ctrl Pts',(9.51167976745598,1.54844713801948,-8.8336910486412));
#33014=CARTESIAN_POINT('Ctrl Pts',(9.49136629635905,1.54919911118225,-8.8464684665095));
#33015=CARTESIAN_POINT('Ctrl Pts',(9.46506696218071,1.55017267170307,-8.86301106431817));
#33016=CARTESIAN_POINT('Ctrl Pts',(9.43797899027672,1.55102830390587,-8.87834410170704));
#33017=CARTESIAN_POINT('Ctrl Pts',(9.41005849198976,1.55176304374565,-8.89245771574993));
#33018=CARTESIAN_POINT('Ctrl Pts',(9.38509876020795,1.55241986975004,-8.9050746833041));
#33019=CARTESIAN_POINT('Ctrl Pts',(9.35947295571484,1.55298008346687,-8.91671676781031));
#33020=CARTESIAN_POINT('Ctrl Pts',(9.33313997277414,1.5534415673395,-8.92734296821911));
#33021=CARTESIAN_POINT('Ctrl Pts',(9.30524515786841,1.55393042221925,-8.93859941775323));
#33022=CARTESIAN_POINT('Ctrl Pts',(9.27656418794365,1.55430848844038,-8.94871368108735));
#33023=CARTESIAN_POINT('Ctrl Pts',(9.2470373763062,1.55456292647825,-8.95759733964878));
#33024=CARTESIAN_POINT('Ctrl Pts',(9.21751056466876,1.55481736451613,-8.96648099821022));
#33025=CARTESIAN_POINT('Ctrl Pts',(9.18713704206229,1.55494817437075,-8.97413435291267));
#33026=CARTESIAN_POINT('Ctrl Pts',(9.15586562026909,1.5549425165175,-8.9804159083562));
#33027=CARTESIAN_POINT('Ctrl Pts',(9.12334173955173,1.55493663206027,-8.98694904782506));
#33028=CARTESIAN_POINT('Ctrl Pts',(9.08984768872008,1.5547831295879,-8.99199043374914));
#33029=CARTESIAN_POINT('Ctrl Pts',(9.05558312753583,1.55446759872465,-8.9953178779505));
#33030=CARTESIAN_POINT('Ctrl Pts',(9.02395754758573,1.55417636935538,-8.99838904970879));
#33031=CARTESIAN_POINT('Ctrl Pts',(8.99167619777338,1.55374710862609,-9.00000000000432));
#33032=CARTESIAN_POINT('Ctrl Pts',(8.95892744039,1.553168485875,-9.));
#33033=CARTESIAN_POINT('Ctrl Pts',(9.6539425342,1.568966285828,-8.717909048124));
#33034=CARTESIAN_POINT('Ctrl Pts',(9.646944923898,1.569906069969,-8.72464832123));
#33035=CARTESIAN_POINT('Ctrl Pts',(9.597148177396,1.576355760916,-8.771213723106));
#33036=CARTESIAN_POINT('Ctrl Pts',(9.494950476551,1.58651869939,-8.848842890954));
#33037=CARTESIAN_POINT('Ctrl Pts',(9.333640806294,1.595561978493,-8.931284233888));
#33038=CARTESIAN_POINT('Ctrl Pts',(9.152534187008,1.598909442216,-8.985523427163));
#33039=CARTESIAN_POINT('Ctrl Pts',(9.013894746136,1.59647733588,-8.999282347838));
#33040=CARTESIAN_POINT('Ctrl Pts',(8.937785978218,1.593573411533,-8.998158240137));
#33041=CARTESIAN_POINT('Ctrl Pts',(8.927957313071,1.593172004412,-8.997866979416));
#33042=CARTESIAN_POINT('Ctrl Pts',(9.645773859302,1.285243398955,-8.747934853163));
#33043=CARTESIAN_POINT('Ctrl Pts',(9.638958599346,1.286161413433,-8.754518076087));
#33044=CARTESIAN_POINT('Ctrl Pts',(9.590459936523,1.29246171878,-8.800004804342));
#33045=CARTESIAN_POINT('Ctrl Pts',(9.490931861646,1.302389666159,-8.875830399956));
#33046=CARTESIAN_POINT('Ctrl Pts',(9.333848365003,1.311227380035,-8.956348467272));
#33047=CARTESIAN_POINT('Ctrl Pts',(9.157494856417,1.314507075387,-9.0093185165));
#33048=CARTESIAN_POINT('Ctrl Pts',(9.022494227322,1.312143653767,-9.022753948681));
#33049=CARTESIAN_POINT('Ctrl Pts',(8.948380876688,1.309315289639,-9.021654826406));
#33050=CARTESIAN_POINT('Ctrl Pts',(8.938809856917,1.308924276241,-9.021370203034));
#33051=CARTESIAN_POINT('Ctrl Pts',(9.501656950695,1.070344855274,-8.627454082903));
#33052=CARTESIAN_POINT('Ctrl Pts',(9.496360026356,1.071055961909,-8.632589318456));
#33053=CARTESIAN_POINT('Ctrl Pts',(9.458669824932,1.075935204229,-8.668067974497));
#33054=CARTESIAN_POINT('Ctrl Pts',(9.381370324166,1.083610835663,-8.727171256311));
#33055=CARTESIAN_POINT('Ctrl Pts',(9.259475956808,1.090423267748,-8.789877060081));
#33056=CARTESIAN_POINT('Ctrl Pts',(9.122699106024,1.092933570735,-8.831108527563));
#33057=CARTESIAN_POINT('Ctrl Pts',(9.017996952515,1.091092054531,-8.8415656694));
#33058=CARTESIAN_POINT('Ctrl Pts',(8.960498394176,1.08889895505,-8.840709420371));
#33059=CARTESIAN_POINT('Ctrl Pts',(8.953072652207,1.088595839625,-8.840487779265));
#33060=CARTESIAN_POINT('Ctrl Pts',(9.302738927017,1.045272401126,-8.424305184978));
#33061=CARTESIAN_POINT('Ctrl Pts',(9.299441402642,1.045707964206,-8.427515806291));
#33062=CARTESIAN_POINT('Ctrl Pts',(9.275984179159,1.048694616249,-8.449692181949));
#33063=CARTESIAN_POINT('Ctrl Pts',(9.227956079129,1.053368806096,-8.486570150069));
#33064=CARTESIAN_POINT('Ctrl Pts',(9.152400046375,1.057476604153,-8.525604156071));
#33065=CARTESIAN_POINT('Ctrl Pts',(9.067739188484,1.058949108328,-8.551237183059));
#33066=CARTESIAN_POINT('Ctrl Pts',(9.002935177616,1.057788851816,-8.557738202339));
#33067=CARTESIAN_POINT('Ctrl Pts',(8.967315586458,1.056433026425,-8.557205961066));
#33068=CARTESIAN_POINT('Ctrl Pts',(8.962714824892,1.056245820989,-8.557068184064));
#33069=CARTESIAN_POINT('Origin',(9.295100309023,1.542473380275,-8.370118632984));
#33070=CARTESIAN_POINT('Ctrl Pts',(9.485442651867,1.647108267952,8.860081856811));
#33071=CARTESIAN_POINT('Ctrl Pts',(9.534636055674,1.64096510107,8.816948883762));
#33072=CARTESIAN_POINT('Ctrl Pts',(9.870608039504,1.598500395072,8.517369852702));
#33073=CARTESIAN_POINT('Ctrl Pts',(10.43190063343,1.521624710073,7.955944056789));
#33074=CARTESIAN_POINT('Ctrl Pts',(11.09326750931,1.42128421097,7.158960123002));
#33075=CARTESIAN_POINT('Ctrl Pts',(11.62445570885,1.33442407676,6.398723949699));
#33076=CARTESIAN_POINT('Ctrl Pts',(12.05012035755,1.260803969321,5.681200837573));
#33077=CARTESIAN_POINT('Ctrl Pts',(12.3950828246,1.198551710967,4.999467721285));
#33078=CARTESIAN_POINT('Ctrl Pts',(12.68374840675,1.144689166094,4.328719065733));
#33079=CARTESIAN_POINT('Ctrl Pts',(12.93020205058,1.097406293304,3.643458045457));
#33080=CARTESIAN_POINT('Ctrl Pts',(13.13571146032,1.057052001434,2.936359424241));
#33081=CARTESIAN_POINT('Ctrl Pts',(13.29688798186,1.024817639632,2.215855271431));
#33082=CARTESIAN_POINT('Ctrl Pts',(13.41249169134,1.00138297161,1.48878756032));
#33083=CARTESIAN_POINT('Ctrl Pts',(13.48260841803,0.9870409655564,0.7555736754422));
#33084=CARTESIAN_POINT('Ctrl Pts',(13.50680269221,0.982069625917,0.01877529667324));
#33085=CARTESIAN_POINT('Ctrl Pts',(13.48500661443,0.9865486686153,-0.7154601880356));
#33086=CARTESIAN_POINT('Ctrl Pts',(13.41819019154,1.000220349609,-1.441614172335));
#33087=CARTESIAN_POINT('Ctrl Pts',(13.30787595815,1.022599136136,-2.155736540013));
#33088=CARTESIAN_POINT('Ctrl Pts',(13.15767129232,1.052680207326,-2.845996704197));
#33089=CARTESIAN_POINT('Ctrl Pts',(12.97703907332,1.088248262002,-3.489954094899));
#33090=CARTESIAN_POINT('Ctrl Pts',(12.77682071924,1.12690535597,-4.077973333215));
#33091=CARTESIAN_POINT('Ctrl Pts',(12.55943682104,1.167989222857,-4.624788445562));
#33092=CARTESIAN_POINT('Ctrl Pts',(12.31876846793,1.2123926264,-5.153155013548));
#33093=CARTESIAN_POINT('Ctrl Pts',(12.05079729047,1.260473276706,-5.671685873951));
#33094=CARTESIAN_POINT('Ctrl Pts',(11.75644670744,1.311635180831,-6.177986581914));
#33095=CARTESIAN_POINT('Ctrl Pts',(11.4341748887,1.365674385277,-6.673870492724));
#33096=CARTESIAN_POINT('Ctrl Pts',(11.07534695527,1.423420589966,-7.169262308066));
#33097=CARTESIAN_POINT('Ctrl Pts',(10.66577646073,1.486219448941,-7.675934257889));
#33098=CARTESIAN_POINT('Ctrl Pts',(10.18588708925,1.555563635995,-8.204530961181));
#33099=CARTESIAN_POINT('Ctrl Pts',(9.78023156014,1.609923272329,-8.597955355053));
#33100=CARTESIAN_POINT('Ctrl Pts',(9.534645036012,1.640963964657,-8.816940683287));
#33101=CARTESIAN_POINT('Ctrl Pts',(9.485454699128,1.647106839676,-8.860071905716));
#33102=CARTESIAN_POINT('Ctrl Pts',(9.501283507643,1.340755486448,8.919478683582));
#33103=CARTESIAN_POINT('Ctrl Pts',(9.550507790226,1.334558254542,8.876058628521));
#33104=CARTESIAN_POINT('Ctrl Pts',(9.886690580984,1.291720690537,8.574485288614));
#33105=CARTESIAN_POINT('Ctrl Pts',(10.44833443549,1.214179980504,8.009317354798));
#33106=CARTESIAN_POINT('Ctrl Pts',(11.11011430115,1.112986469181,7.207011291774));
#33107=CARTESIAN_POINT('Ctrl Pts',(11.64163405682,1.025396523771,6.441690810591));
#33108=CARTESIAN_POINT('Ctrl Pts',(12.06756458097,0.9511628997746,5.719363221124));
#33109=CARTESIAN_POINT('Ctrl Pts',(12.41274280116,0.8883949022656,5.033060755404));
#33110=CARTESIAN_POINT('Ctrl Pts',(12.70158922282,0.8340880943174,4.357812662756));
#33111=CARTESIAN_POINT('Ctrl Pts',(12.94819754771,0.7864166089429,3.667951535326));
#33112=CARTESIAN_POINT('Ctrl Pts',(13.15383619157,0.74573159891,2.956103202327));
#33113=CARTESIAN_POINT('Ctrl Pts',(13.31511425316,0.7132336445999,2.230756755417));
#33114=CARTESIAN_POINT('Ctrl Pts',(13.43079090278,0.6896076458371,1.498800686597));
#33115=CARTESIAN_POINT('Ctrl Pts',(13.50095191817,0.6751486666702,0.7606557814507));
#33116=CARTESIAN_POINT('Ctrl Pts',(13.52516148339,0.6701368018972,0.01890158512833));
#33117=CARTESIAN_POINT('Ctrl Pts',(13.50335163006,0.6746523562059,-0.7202724951362));
#33118=CARTESIAN_POINT('Ctrl Pts',(13.43649300123,0.6884355387342,-1.451310075406));
#33119=CARTESIAN_POINT('Ctrl Pts',(13.32610915903,0.7109970198194,-2.170233874786));
#33120=CARTESIAN_POINT('Ctrl Pts',(13.17580985142,0.7413240355844,-2.86513326537));
#33121=CARTESIAN_POINT('Ctrl Pts',(12.99506401229,0.7771834854259,-3.513416598512));
#33122=CARTESIAN_POINT('Ctrl Pts',(12.79471993203,0.8161580465605,-4.105383881712));
#33123=CARTESIAN_POINT('Ctrl Pts',(12.57719973951,0.8575802200963,-4.655868321512));
#33124=CARTESIAN_POINT('Ctrl Pts',(12.33638070567,0.9023504074507,-5.187778254645));
#33125=CARTESIAN_POINT('Ctrl Pts',(12.068241961,0.9508297021305,-5.709784168435));
#33126=CARTESIAN_POINT('Ctrl Pts',(11.77370749238,1.002417669683,-6.219475482681));
#33127=CARTESIAN_POINT('Ctrl Pts',(11.45123446739,1.056909230048,-6.718677630099));
#33128=CARTESIAN_POINT('Ctrl Pts',(11.09218254538,1.115141808556,-7.217381559891));
#33129=CARTESIAN_POINT('Ctrl Pts',(10.68235630247,1.178473627838,-7.727437814332));
#33130=CARTESIAN_POINT('Ctrl Pts',(10.20216697086,1.248412121368,-8.25956136877));
#33131=CARTESIAN_POINT('Ctrl Pts',(9.796257394007,1.303243865608,-8.655607251179));
#33132=CARTESIAN_POINT('Ctrl Pts',(9.55051677653,1.334557108182,-8.876050373624));
#33133=CARTESIAN_POINT('Ctrl Pts',(9.501295562957,1.340754045595,-8.919468666609));
#33134=CARTESIAN_POINT('Ctrl Pts',(9.359979883938,1.092901517146,8.792071381238));
#33135=CARTESIAN_POINT('Ctrl Pts',(9.40827342587,1.086922770804,8.749258499761));
#33136=CARTESIAN_POINT('Ctrl Pts',(9.73810212497,1.045593549208,8.451901782226));
#33137=CARTESIAN_POINT('Ctrl Pts',(10.28915836763,0.9707608749562,7.89463319151));
#33138=CARTESIAN_POINT('Ctrl Pts',(10.93848999477,0.8730705639218,7.10356490815));
#33139=CARTESIAN_POINT('Ctrl Pts',(11.46001606517,0.7884977051436,6.349006483595));
#33140=CARTESIAN_POINT('Ctrl Pts',(11.87793263586,0.7168140964409,5.636885495828));
#33141=CARTESIAN_POINT('Ctrl Pts',(12.21660767664,0.6561993181206,4.960329573556));
#33142=CARTESIAN_POINT('Ctrl Pts',(12.50000327728,0.6037544207696,4.294718569006));
#33143=CARTESIAN_POINT('Ctrl Pts',(12.74194924295,0.5577172247791,3.614751118391));
#33144=CARTESIAN_POINT('Ctrl Pts',(12.94369254322,0.5184273359704,2.913159732911));
#33145=CARTESIAN_POINT('Ctrl Pts',(13.10191000897,0.487044227227,2.19830818232));
#33146=CARTESIAN_POINT('Ctrl Pts',(13.21538811471,0.4642290789812,1.476977936882));
#33147=CARTESIAN_POINT('Ctrl Pts',(13.28421419066,0.4502665148141,0.7495738144426));
#33148=CARTESIAN_POINT('Ctrl Pts',(13.30796285691,0.4454267556509,0.0186261527622));
#33149=CARTESIAN_POINT('Ctrl Pts',(13.28656822283,0.4497872467096,-0.7097786655537));
#33150=CARTESIAN_POINT('Ctrl Pts',(13.22098175535,0.4630972089924,-1.430177833726));
#33151=CARTESIAN_POINT('Ctrl Pts',(13.11269604486,0.4848843526421,-2.138662949869));
#33152=CARTESIAN_POINT('Ctrl Pts',(12.96524940725,0.5141709553425,-2.823504541799));
#33153=CARTESIAN_POINT('Ctrl Pts',(12.7879282788,0.5488006889822,-3.462440733503));
#33154=CARTESIAN_POINT('Ctrl Pts',(12.59137380672,0.5864390447853,-4.045907115348));
#33155=CARTESIAN_POINT('Ctrl Pts',(12.37796176471,0.6264411523485,-4.588517372372));
#33156=CARTESIAN_POINT('Ctrl Pts',(12.14168451331,0.6696761533601,-5.112848598301));
#33157=CARTESIAN_POINT('Ctrl Pts',(11.87859653892,0.716492108312,-5.627445918905));
#33158=CARTESIAN_POINT('Ctrl Pts',(11.58960470579,0.7663082323814,-6.129930166316));
#33159=CARTESIAN_POINT('Ctrl Pts',(11.27319639095,0.8189252214204,-6.622097308292));
#33160=CARTESIAN_POINT('Ctrl Pts',(10.92089587887,0.8751498914803,-7.113793976026));
#33161=CARTESIAN_POINT('Ctrl Pts',(10.51877834181,0.9362907877084,-7.616701069514));
#33162=CARTESIAN_POINT('Ctrl Pts',(10.04763033621,1.003798345438,-8.141379735601));
#33163=CARTESIAN_POINT('Ctrl Pts',(9.64937820522,1.056710983639,-8.531889495748));
#33164=CARTESIAN_POINT('Ctrl Pts',(9.408282232358,1.086921664791,-8.749250354908));
#33165=CARTESIAN_POINT('Ctrl Pts',(9.359991696511,1.092900125163,-8.792061502863));
#33166=CARTESIAN_POINT('Ctrl Pts',(9.152731006036,1.063514585851,8.560090305693));
#33167=CARTESIAN_POINT('Ctrl Pts',(9.1997329002,1.057885862191,8.518386975545));
#33168=CARTESIAN_POINT('Ctrl Pts',(9.520743623748,1.018972679307,8.228736347825));
#33169=CARTESIAN_POINT('Ctrl Pts',(10.05710676667,0.9484732995852,7.685910240827));
#33170=CARTESIAN_POINT('Ctrl Pts',(10.68916318457,0.8563813896063,6.915386634592));
#33171=CARTESIAN_POINT('Ctrl Pts',(11.19682038478,0.7766252477241,6.180490657665));
#33172=CARTESIAN_POINT('Ctrl Pts',(11.60361548453,0.709009372612,5.486999875077));
#33173=CARTESIAN_POINT('Ctrl Pts',(11.93326565123,0.6518270557176,4.828215841246));
#33174=CARTESIAN_POINT('Ctrl Pts',(12.20909680221,0.6023485409416,4.180158546027));
#33175=CARTESIAN_POINT('Ctrl Pts',(12.44457251662,0.5589137443474,3.51819304649));
#33176=CARTESIAN_POINT('Ctrl Pts',(12.64091000179,0.5218443864833,2.835245298414));
#33177=CARTESIAN_POINT('Ctrl Pts',(12.7948800848,0.4922350253254,2.139452289843));
#33178=CARTESIAN_POINT('Ctrl Pts',(12.90530713191,0.4707095752198,1.43740400211));
#33179=CARTESIAN_POINT('Ctrl Pts',(12.97228062783,0.4575364213677,0.7294802223117));
#33180=CARTESIAN_POINT('Ctrl Pts',(12.99538967536,0.4529703193238,0.01812676726228));
#33181=CARTESIAN_POINT('Ctrl Pts',(12.97457126737,0.4570842521421,-0.6907515555187));
#33182=CARTESIAN_POINT('Ctrl Pts',(12.91075025878,0.4696416949965,-1.39185647522));
#33183=CARTESIAN_POINT('Ctrl Pts',(12.80537625858,0.4901972368263,-2.081400057238));
#33184=CARTESIAN_POINT('Ctrl Pts',(12.66188845186,0.5178285651575,-2.747978261569));
#33185=CARTESIAN_POINT('Ctrl Pts',(12.4893200114,0.5505011463086,-3.369926996511));
#33186=CARTESIAN_POINT('Ctrl Pts',(12.29802461869,0.5860120288538,-3.937930124791));
#33187=CARTESIAN_POINT('Ctrl Pts',(12.0903137174,0.6237522271604,-4.466204790387));
#33188=CARTESIAN_POINT('Ctrl Pts',(11.86033938522,0.6645409012191,-4.976726634499));
#33189=CARTESIAN_POINT('Ctrl Pts',(11.60426068474,0.7087050737737,-5.477813319251));
#33190=CARTESIAN_POINT('Ctrl Pts',(11.32296071804,0.7556950186386,-5.967144362846));
#33191=CARTESIAN_POINT('Ctrl Pts',(11.0149687857,0.8053203822034,-6.446463742772));
#33192=CARTESIAN_POINT('Ctrl Pts',(10.6720376329,0.8583387921827,-6.925356351434));
#33193=CARTESIAN_POINT('Ctrl Pts',(10.28061795534,0.915978932676,-7.415194981312));
#33194=CARTESIAN_POINT('Ctrl Pts',(9.822017170651,0.9795992704055,-7.926262048838));
#33195=CARTESIAN_POINT('Ctrl Pts',(9.434391762418,1.029440205011,-8.306651162358));
#33196=CARTESIAN_POINT('Ctrl Pts',(9.199741457146,1.057884820781,-8.518379034178));
#33197=CARTESIAN_POINT('Ctrl Pts',(9.152742481741,1.063513272641,-8.560080680939));
#33198=CARTESIAN_POINT('',(9.631273226511,1.5424733773,8.740237221479));
#33199=CARTESIAN_POINT('Ctrl Pts',(9.63127322651082,1.5424733773,8.7402372214788));
#33200=CARTESIAN_POINT('Ctrl Pts',(9.76016736551745,1.52748192728802,8.62316346505574));
#33201=CARTESIAN_POINT('Ctrl Pts',(9.88367797190008,1.51265196794207,8.50577017900236));
#33202=CARTESIAN_POINT('Ctrl Pts',(10.0019313763767,1.49808103045733,8.38863411644834));
#33203=CARTESIAN_POINT('Ctrl Pts',(10.1221460058904,1.48326843492024,8.26955535990054));
#33204=CARTESIAN_POINT('Ctrl Pts',(10.2369277857404,1.46872349768402,8.15074250929634));
#33205=CARTESIAN_POINT('Ctrl Pts',(10.3464427733501,1.45452769271862,8.03276472333058));
#33206=CARTESIAN_POINT('Ctrl Pts',(10.380527813305,1.45010944285166,7.9960457532955));
#33207=CARTESIAN_POINT('Ctrl Pts',(10.4141028979157,1.44572486363172,7.95940740548168));
#33208=CARTESIAN_POINT('Ctrl Pts',(10.4471736310341,1.44137601424082,7.92286611309366));
#33209=CARTESIAN_POINT('Ctrl Pts',(10.536440168792,1.42963733499938,7.82423163030186));
#33210=CARTESIAN_POINT('Ctrl Pts',(10.6220293312436,1.41816178692121,7.72631349155243));
#33211=CARTESIAN_POINT('Ctrl Pts',(10.704297540876,1.40695201812211,7.62913681450109));
#33212=CARTESIAN_POINT('Ctrl Pts',(10.789095425202,1.39539755884562,7.52897204056718));
#33213=CARTESIAN_POINT('Ctrl Pts',(10.8703651110396,1.38412536211667,7.42959483382496));
#33214=CARTESIAN_POINT('Ctrl Pts',(10.9484674400921,1.37313074153775,7.33098567275051));
#33215=CARTESIAN_POINT('Ctrl Pts',(11.0015800711469,1.36565397056971,7.26392759581079));
#33216=CARTESIAN_POINT('Ctrl Pts',(11.053227327317,1.35830540981071,7.19722372438596));
#33217=CARTESIAN_POINT('Ctrl Pts',(11.1035148709274,1.35108206939083,7.1308567988699));
#33218=CARTESIAN_POINT('Ctrl Pts',(11.2015036679035,1.33700688521846,7.00153620129411));
#33219=CARTESIAN_POINT('Ctrl Pts',(11.2943246180977,1.32340992308326,6.87350257018018));
#33220=CARTESIAN_POINT('Ctrl Pts',(11.3823679190261,1.31031122879814,6.74706040500975));
#33221=CARTESIAN_POINT('Ctrl Pts',(11.4704112199545,1.29721253451303,6.62061823983932));
#33222=CARTESIAN_POINT('Ctrl Pts',(11.5536769978988,1.28461192973242,6.4957671084551));
#33223=CARTESIAN_POINT('Ctrl Pts',(11.6325422446539,1.27251585364215,6.37275783163964));
#33224=CARTESIAN_POINT('Ctrl Pts',(11.7130560730598,1.26016692385639,6.24717719614634));
#33225=CARTESIAN_POINT('Ctrl Pts',(11.788983030893,1.24834526068386,6.12351749166098));
#33226=CARTESIAN_POINT('Ctrl Pts',(11.8607187737643,1.23704304155025,6.0019887645426));
#33227=CARTESIAN_POINT('Ctrl Pts',(11.9295168292409,1.22620366542002,5.88543682299102));
#33228=CARTESIAN_POINT('Ctrl Pts',(11.9944598344691,1.21584188353946,5.77084425224909));
#33229=CARTESIAN_POINT('Ctrl Pts',(12.0558789256988,1.20594334387555,5.65835573107204));
#33230=CARTESIAN_POINT('Ctrl Pts',(12.1038310837798,1.19821518754449,5.57053177858779));
#33231=CARTESIAN_POINT('Ctrl Pts',(12.1496367114629,1.19077219983256,5.48399330909393));
#33232=CARTESIAN_POINT('Ctrl Pts',(12.1936278131294,1.18357376049498,5.39842189093468));
#33233=CARTESIAN_POINT('Ctrl Pts',(12.2386454394624,1.17620734683392,5.31085367869266));
#33234=CARTESIAN_POINT('Ctrl Pts',(12.2817628927706,1.16909695753592,5.22429795088912));
#33235=CARTESIAN_POINT('Ctrl Pts',(12.3232908005036,1.16220259249432,5.13838260493158));
#33236=CARTESIAN_POINT('Ctrl Pts',(12.3473569046407,1.15820719479413,5.08859325180347));
#33237=CARTESIAN_POINT('Ctrl Pts',(12.3708883419127,1.15428441754086,5.03901841395892));
#33238=CARTESIAN_POINT('Ctrl Pts',(12.3939388048181,1.15042713724629,4.98958152163347));
#33239=CARTESIAN_POINT('Ctrl Pts',(12.4317412300487,1.14410125344399,4.90850573441675));
#33240=CARTESIAN_POINT('Ctrl Pts',(12.4682510143418,1.13795307997892,4.82780619813583));
#33241=CARTESIAN_POINT('Ctrl Pts',(12.5037313437523,1.13194537250749,4.74700117092273));
#33242=CARTESIAN_POINT('Ctrl Pts',(12.5392814814001,1.12592584475489,4.66603715824885));
#33243=CARTESIAN_POINT('Ctrl Pts',(12.5737981464946,1.12004727777973,4.58496704665721));
#33244=CARTESIAN_POINT('Ctrl Pts',(12.6074992630549,1.11427866384779,4.50328422139707));
#33245=CARTESIAN_POINT('Ctrl Pts',(12.6306462071191,1.11031660568355,4.4471819915516));
#33246=CARTESIAN_POINT('Ctrl Pts',(12.653407468017,1.10640654850001,4.39079027065877));
#33247=CARTESIAN_POINT('Ctrl Pts',(12.6758406044922,1.1025404436147,4.33393955596147));
#33248=CARTESIAN_POINT('Ctrl Pts',(12.7274812603864,1.09364074328731,4.20307028593055));
#33249=CARTESIAN_POINT('Ctrl Pts',(12.7773728839536,1.08496340147549,4.06976945161404));
#33250=CARTESIAN_POINT('Ctrl Pts',(12.8252096589171,1.07658322740027,3.93441410555896));
#33251=CARTESIAN_POINT('Ctrl Pts',(12.8586060667958,1.07073275542085,3.83991813778412));
#33252=CARTESIAN_POINT('Ctrl Pts',(12.8910018140696,1.06502704983544,3.74442145063781));
#33253=CARTESIAN_POINT('Ctrl Pts',(12.9223056969685,1.0594901363143,3.64806012546232));
#33254=CARTESIAN_POINT('Ctrl Pts',(12.9568881477048,1.05337332199786,3.54160653337837));
#33255=CARTESIAN_POINT('Ctrl Pts',(12.9901360722762,1.04746035389728,3.43409399001926));
#33256=CARTESIAN_POINT('Ctrl Pts',(13.0218729325533,1.04178927772019,3.32598947361619));
#33257=CARTESIAN_POINT('Ctrl Pts',(13.0535488749454,1.03612908699186,3.21809246036381));
#33258=CARTESIAN_POINT('Ctrl Pts',(13.0837194710999,1.03070992177902,3.10960598071963));
#33259=CARTESIAN_POINT('Ctrl Pts',(13.1122581627635,1.02556110406422,3.00100968818389));
#33260=CARTESIAN_POINT('Ctrl Pts',(13.1180829828847,1.02451021717076,2.97884490651453));
#33261=CARTESIAN_POINT('Ctrl Pts',(13.1238399864087,1.02347056232403,2.95667559452744));
#33262=CARTESIAN_POINT('Ctrl Pts',(13.1295283518426,1.02244234182423,2.93450589513787));
#33263=CARTESIAN_POINT('Ctrl Pts',(13.1668836820405,1.0156900477369,2.78891812467845));
#33264=CARTESIAN_POINT('Ctrl Pts',(13.2012838387308,1.00943843149588,2.64331335810838));
#33265=CARTESIAN_POINT('Ctrl Pts',(13.2328430798278,1.00367908012121,2.49748776573468));
#33266=CARTESIAN_POINT('Ctrl Pts',(13.2532264254349,0.999959255262895,2.40330256531842));
#33267=CARTESIAN_POINT('Ctrl Pts',(13.2724236824129,0.996444944216602,2.30902485890701));
#33268=CARTESIAN_POINT('Ctrl Pts',(13.2904547716062,0.993135801902423,2.21459634085511));
#33269=CARTESIAN_POINT('Ctrl Pts',(13.3214594197414,0.98744569677451,2.05222550763766));
#33270=CARTESIAN_POINT('Ctrl Pts',(13.3490176029642,0.982361156275227,1.88941172405413));
#33271=CARTESIAN_POINT('Ctrl Pts',(13.3731643781013,0.977892034139776,1.72600340806214));
#33272=CARTESIAN_POINT('Ctrl Pts',(13.3848027163602,0.975737992664778,1.6472433564596));
#33273=CARTESIAN_POINT('Ctrl Pts',(13.3956478126217,0.97372706051493,1.56834503918377));
#33274=CARTESIAN_POINT('Ctrl Pts',(13.4056993955901,0.971861166161085,1.48929083180983));
#33275=CARTESIAN_POINT('Ctrl Pts',(13.4366056150463,0.96612398620019,1.2462180054005));
#33276=CARTESIAN_POINT('Ctrl Pts',(13.4600071666758,0.961754442251598,1.00167097719576));
#33277=CARTESIAN_POINT('Ctrl Pts',(13.4757625271622,0.958810186936582,0.75615674000873));
#33278=CARTESIAN_POINT('Ctrl Pts',(13.4870314438372,0.956704327927927,0.580554316707783));
#33279=CARTESIAN_POINT('Ctrl Pts',(13.4943847641842,0.955326771075483,0.404456792494881));
#33280=CARTESIAN_POINT('Ctrl Pts',(13.4977916921877,0.954688412324058,0.228331189878502));
#33281=CARTESIAN_POINT('Ctrl Pts',(13.499148077322,0.95443426538586,0.158211084932178));
#33282=CARTESIAN_POINT('Ctrl Pts',(13.4998795101869,0.954297167785211,0.0880865669065382));
#33283=CARTESIAN_POINT('Ctrl Pts',(13.4999862992676,0.954277342264801,0.0179871712228238));
#33284=CARTESIAN_POINT('Ctrl Pts',(13.5002265334807,0.95423274249614,-0.13970941207456));
#33285=CARTESIAN_POINT('Ctrl Pts',(13.4973018794775,0.954781650237799,-0.29727994041566));
#33286=CARTESIAN_POINT('Ctrl Pts',(13.4912574586599,0.955912892086901,-0.454274314967719));
#33287=CARTESIAN_POINT('Ctrl Pts',(13.4878662083785,0.956547580563249,-0.542356735591353));
#33288=CARTESIAN_POINT('Ctrl Pts',(13.4834938311073,0.957365388509113,-0.630257845020122));
#33289=CARTESIAN_POINT('Ctrl Pts',(13.4781552909154,0.95836291423459,-0.717898947514517));
#33290=CARTESIAN_POINT('Ctrl Pts',(13.4661608904116,0.960604111759422,-0.914807174507933));
#33291=CARTESIAN_POINT('Ctrl Pts',(13.4492956345586,0.963755902347615,-1.11040352667427));
#33292=CARTESIAN_POINT('Ctrl Pts',(13.4276955991877,0.967773971019727,-1.30468906634728));
#33293=CARTESIAN_POINT('Ctrl Pts',(13.4225463984485,0.968731832514913,-1.35100451108217));
#33294=CARTESIAN_POINT('Ctrl Pts',(13.4171278995042,0.969738972562947,-1.39724550214024));
#33295=CARTESIAN_POINT('Ctrl Pts',(13.4114415260978,0.970794881126638,-1.44341211566292));
#33296=CARTESIAN_POINT('Ctrl Pts',(13.3924576987589,0.974320007674985,-1.59753829720194));
#33297=CARTESIAN_POINT('Ctrl Pts',(13.3704926452548,0.978389043240586,-1.75083401852059));
#33298=CARTESIAN_POINT('Ctrl Pts',(13.3455542466026,0.98299168568862,-1.90350363273298));
#33299=CARTESIAN_POINT('Ctrl Pts',(13.3316872845961,0.985550978642689,-1.98839536011907));
#33300=CARTESIAN_POINT('Ctrl Pts',(13.3169000816878,0.988275444713513,-2.07309342852308));
#33301=CARTESIAN_POINT('Ctrl Pts',(13.3011872234493,0.991164664440456,-2.15763205493448));
#33302=CARTESIAN_POINT('Ctrl Pts',(13.2817749696322,0.994734114748057,-2.2620742416032));
#33303=CARTESIAN_POINT('Ctrl Pts',(13.2609449552185,0.998551087536764,-2.3662727735945));
#33304=CARTESIAN_POINT('Ctrl Pts',(13.2388164250053,1.00259155889224,-2.46972511079396));
#33305=CARTESIAN_POINT('Ctrl Pts',(13.2165454097734,1.00665804673552,-2.57384357484662));
#33306=CARTESIAN_POINT('Ctrl Pts',(13.1929591758184,1.01095087186728,-2.67720597429563));
#33307=CARTESIAN_POINT('Ctrl Pts',(13.168229649725,1.01543629733027,-2.77931309282663));
#33308=CARTESIAN_POINT('Ctrl Pts',(13.1618737206253,1.01658913164328,-2.8055564427198));
#33309=CARTESIAN_POINT('Ctrl Pts',(13.1554425213489,1.01775464375683,-2.83171694779066));
#33310=CARTESIAN_POINT('Ctrl Pts',(13.1489394909979,1.01893216973745,-2.85778629807699));
#33311=CARTESIAN_POINT('Ctrl Pts',(13.1263239080982,1.02302725079878,-2.94844765451032));
#33312=CARTESIAN_POINT('Ctrl Pts',(13.1028347601488,1.02726732550112,-3.03800882211687));
#33313=CARTESIAN_POINT('Ctrl Pts',(13.0787022721279,1.03160637240792,-3.12591046701909));
#33314=CARTESIAN_POINT('Ctrl Pts',(13.0539550821271,1.0360559433818,-3.21605113987043));
#33315=CARTESIAN_POINT('Ctrl Pts',(13.0285314995321,1.04060952686829,-3.30444647936617));
#33316=CARTESIAN_POINT('Ctrl Pts',(13.0027308146993,1.0452092509767,-3.39051297959414));
#33317=CARTESIAN_POINT('Ctrl Pts',(12.9903401839258,1.04741824207352,-3.43184592223512));
#33318=CARTESIAN_POINT('Ctrl Pts',(12.9778633112975,1.04963776091173,-3.47264205963787));
#33319=CARTESIAN_POINT('Ctrl Pts',(12.9653371636099,1.0518608243978,-3.51283847920185));
#33320=CARTESIAN_POINT('Ctrl Pts',(12.9397525056021,1.05640143180874,-3.59493967051231));
#33321=CARTESIAN_POINT('Ctrl Pts',(12.9139675330497,1.06096428172172,-3.67453971736313));
#33322=CARTESIAN_POINT('Ctrl Pts',(12.8879510802549,1.06555104034565,-3.7521646067085));
#33323=CARTESIAN_POINT('Ctrl Pts',(12.8611841832938,1.07027010394901,-3.83202858475043));
#33324=CARTESIAN_POINT('Ctrl Pts',(12.8341721013302,1.07501454269927,-3.90980195282997));
#33325=CARTESIAN_POINT('Ctrl Pts',(12.8068280574077,1.07979620072513,-3.98604480334464));
#33326=CARTESIAN_POINT('Ctrl Pts',(12.7942204177638,1.08200090100504,-4.02119843268463));
#33327=CARTESIAN_POINT('Ctrl Pts',(12.7815414973675,1.08421364481377,-4.05602650238246));
#33328=CARTESIAN_POINT('Ctrl Pts',(12.768779288753,1.0864362255717,-4.09058291631843));
#33329=CARTESIAN_POINT('Ctrl Pts',(12.7416044788988,1.09116880841115,-4.1641645357952));
#33330=CARTESIAN_POINT('Ctrl Pts',(12.714056646962,1.09594489502114,-4.23651208758985));
#33331=CARTESIAN_POINT('Ctrl Pts',(12.6859506057501,1.10079561217221,-4.30823009812429));
#33332=CARTESIAN_POINT('Ctrl Pts',(12.6576888991591,1.10567319503226,-4.38034531903806));
#33333=CARTESIAN_POINT('Ctrl Pts',(12.6288626839948,1.11062629594105,-4.45182414645006));
#33334=CARTESIAN_POINT('Ctrl Pts',(12.5992351970053,1.1156943322581,-4.52326269754378));
#33335=CARTESIAN_POINT('Ctrl Pts',(12.5853084146409,1.11807662809128,-4.55684330982678));
#33336=CARTESIAN_POINT('Ctrl Pts',(12.5712039002858,1.12048442557025,-4.59041474515251));
#33337=CARTESIAN_POINT('Ctrl Pts',(12.5568934393279,1.12292235830783,-4.62403736370218));
#33338=CARTESIAN_POINT('Ctrl Pts',(12.5157966851936,1.12992360883407,-4.72059473470175));
#33339=CARTESIAN_POINT('Ctrl Pts',(12.4729962079317,1.13716536282956,-4.81757125875771));
#33340=CARTESIAN_POINT('Ctrl Pts',(12.4286427289522,1.14461307353984,-4.91446457153812));
#33341=CARTESIAN_POINT('Ctrl Pts',(12.392020208736,1.15076262352617,-4.99446905794523));
#33342=CARTESIAN_POINT('Ctrl Pts',(12.3543397615075,1.15705242076176,-5.07441703357359));
#33343=CARTESIAN_POINT('Ctrl Pts',(12.3157108673077,1.1634592045548,-5.15403561069008));
#33344=CARTESIAN_POINT('Ctrl Pts',(12.263417077726,1.1721323755194,-5.26181910293787));
#33345=CARTESIAN_POINT('Ctrl Pts',(12.2093834549275,1.18102122084978,-5.36900096619964));
#33346=CARTESIAN_POINT('Ctrl Pts',(12.1538263915905,1.19007320817802,-5.47515194145451));
#33347=CARTESIAN_POINT('Ctrl Pts',(12.1186412076037,1.19580597770291,-5.54237906561095));
#33348=CARTESIAN_POINT('Ctrl Pts',(12.0828459295794,1.20160405362024,-5.60919316153846));
#33349=CARTESIAN_POINT('Ctrl Pts',(12.0465049645459,1.20745299121237,-5.67549034442851));
#33350=CARTESIAN_POINT('Ctrl Pts',(11.9921789271359,1.21619655655648,-5.77459787320605));
#33351=CARTESIAN_POINT('Ctrl Pts',(11.9366389356514,1.2250554615878,-5.87255244596524));
#33352=CARTESIAN_POINT('Ctrl Pts',(11.8796989992141,1.23404685830823,-5.96971786588508));
#33353=CARTESIAN_POINT('Ctrl Pts',(11.8384064553275,1.24056737214985,-6.04018171985728));
#33354=CARTESIAN_POINT('Ctrl Pts',(11.7963766993591,1.24715769405327,-6.11023007401325));
#33355=CARTESIAN_POINT('Ctrl Pts',(11.7535240951848,1.25382589389963,-6.17999300576206));
#33356=CARTESIAN_POINT('Ctrl Pts',(11.6791717591893,1.26539569799939,-6.30103668656892));
#33357=CARTESIAN_POINT('Ctrl Pts',(11.6023431512998,1.27719852979548,-6.42122091795169));
#33358=CARTESIAN_POINT('Ctrl Pts',(11.522831796062,1.28923292277853,-6.54072032768313));
#33359=CARTESIAN_POINT('Ctrl Pts',(11.4933258998355,1.29369876981941,-6.58506540483728));
#33360=CARTESIAN_POINT('Ctrl Pts',(11.4634501712187,1.29819651733763,-6.6293158522582));
#33361=CARTESIAN_POINT('Ctrl Pts',(11.4331926690046,1.30272611517905,-6.67347939649423));
#33362=CARTESIAN_POINT('Ctrl Pts',(11.3801106222787,1.31067258486998,-6.75095741507395));
#33363=CARTESIAN_POINT('Ctrl Pts',(11.3258574716049,1.3187173628309,-6.82816947322432));
#33364=CARTESIAN_POINT('Ctrl Pts',(11.270099910585,1.32689750593474,-6.90550130181125));
#33365=CARTESIAN_POINT('Ctrl Pts',(11.2151048678493,1.33496578064673,-6.98177557098961));
#33366=CARTESIAN_POINT('Ctrl Pts',(11.1586462082761,1.34316582874487,-7.05816654327559));
#33367=CARTESIAN_POINT('Ctrl Pts',(11.1003648662286,1.35153426861603,-7.13501209334715));
#33368=CARTESIAN_POINT('Ctrl Pts',(11.0932894453453,1.35255020668719,-7.14434123009419));
#33369=CARTESIAN_POINT('Ctrl Pts',(11.0861871138464,1.35356862693456,-7.15367702482475));
#33370=CARTESIAN_POINT('Ctrl Pts',(11.0790571897794,1.35458959500383,-7.16302004684974));
#33371=CARTESIAN_POINT('Ctrl Pts',(11.0163547803249,1.36356825414787,-7.24518501621748));
#33372=CARTESIAN_POINT('Ctrl Pts',(10.9515226474709,1.37274293502362,-7.32791024198651));
#33373=CARTESIAN_POINT('Ctrl Pts',(10.8841959067605,1.38214071339441,-7.41140804188175));
#33374=CARTESIAN_POINT('Ctrl Pts',(10.8168691660501,1.3915384917652,-7.494905841777));
#33375=CARTESIAN_POINT('Ctrl Pts',(10.7470478932044,1.40115948398462,-7.5791766228846));
#33376=CARTESIAN_POINT('Ctrl Pts',(10.6743311014899,1.41102779561278,-7.66439154289842));
#33377=CARTESIAN_POINT('Ctrl Pts',(10.609071748101,1.41988406691836,-7.74086728458169));
#33378=CARTESIAN_POINT('Ctrl Pts',(10.5414820399865,1.42893856155155,-7.81810198386333));
#33379=CARTESIAN_POINT('Ctrl Pts',(10.4711762902307,1.43821456689777,-7.89626316965109));
#33380=CARTESIAN_POINT('Ctrl Pts',(10.402894830669,1.44722349129075,-7.97217388627369));
#33381=CARTESIAN_POINT('Ctrl Pts',(10.3320514165358,1.45644144668458,-8.04895869510814));
#33382=CARTESIAN_POINT('Ctrl Pts',(10.2582624312653,1.46588546680312,-8.12673235594464));
#33383=CARTESIAN_POINT('Ctrl Pts',(10.2387105952778,1.46838784479006,-8.14734000971909));
#33384=CARTESIAN_POINT('Ctrl Pts',(10.2189517878589,1.4709060662173,-8.16801686462112));
#33385=CARTESIAN_POINT('Ctrl Pts',(10.1989785098382,1.47344038183622,-8.18876455273126));
#33386=CARTESIAN_POINT('Ctrl Pts',(10.0991791609495,1.48610345338535,-8.29243335272441));
#33387=CARTESIAN_POINT('Ctrl Pts',(9.99402608080279,1.49916870374078,-8.39786818195577));
#33388=CARTESIAN_POINT('Ctrl Pts',(9.88340877548464,1.51255465483016,-8.50440623974693));
#33389=CARTESIAN_POINT('Ctrl Pts',(9.80230993319642,1.52236853642087,-8.58251439038075));
#33390=CARTESIAN_POINT('Ctrl Pts',(9.71827471455824,1.53235440715854,-8.66121489978216));
#33391=CARTESIAN_POINT('Ctrl Pts',(9.63127322649984,1.542473377301,-8.74023722148882));
#33392=CARTESIAN_POINT('Origin',(9.295100333713,1.542473377277,8.37011861056));
#33393=CARTESIAN_POINT('Origin',(1.692653696601,0.,0.));
#33394=CARTESIAN_POINT('',(9.63127320811535,6.05752662000828,8.74023723818668));
#33395=CARTESIAN_POINT('Ctrl Pts',(9.63127322650206,6.057526622699,-8.74023722148816));
#33396=CARTESIAN_POINT('Ctrl Pts',(9.76588086213937,6.0731825242371,-8.61797523041577));
#33397=CARTESIAN_POINT('Ctrl Pts',(9.89461857444399,6.08865437321686,-8.49536863500099));
#33398=CARTESIAN_POINT('Ctrl Pts',(10.0176281064609,6.10384611849948,-8.37306561562682));
#33399=CARTESIAN_POINT('Ctrl Pts',(10.1431176997746,6.11934415272484,-8.24829677933693));
#33400=CARTESIAN_POINT('Ctrl Pts',(10.2626461575767,6.13455067475198,-8.12384421773691));
#33401=CARTESIAN_POINT('Ctrl Pts',(10.37640803786,6.14936370590824,-8.00036482099906));
#33402=CARTESIAN_POINT('Ctrl Pts',(10.400201994996,6.15246193729742,-7.97453838893019));
#33403=CARTESIAN_POINT('Ctrl Pts',(10.4237438262894,6.15554295497639,-7.94875441217995));
#33404=CARTESIAN_POINT('Ctrl Pts',(10.447035525501,6.15860582586468,-7.92301871272803));
#33405=CARTESIAN_POINT('Ctrl Pts',(10.5370129321437,6.1704379029023,-7.82359996814539));
#33406=CARTESIAN_POINT('Ctrl Pts',(10.6232564765674,6.18199917010837,-7.72490907933849));
#33407=CARTESIAN_POINT('Ctrl Pts',(10.7061287125036,6.19329278823122,-7.62697153961611));
#33408=CARTESIAN_POINT('Ctrl Pts',(10.7912441069049,6.20489209830034,-7.52638305873346));
#33409=CARTESIAN_POINT('Ctrl Pts',(10.872803393278,6.21620907391581,-7.42658905138719));
#33410=CARTESIAN_POINT('Ctrl Pts',(10.951172069922,6.22724713949817,-7.32756878229688));
#33411=CARTESIAN_POINT('Ctrl Pts',(11.0032593022312,6.23458351814911,-7.2617556030995));
#33412=CARTESIAN_POINT('Ctrl Pts',(11.0539365063572,6.24179668801535,-7.19628323082759));
#33413=CARTESIAN_POINT('Ctrl Pts',(11.103304087683,6.24888765453051,-7.13113496894025));
#33414=CARTESIAN_POINT('Ctrl Pts',(11.2012859035996,6.26296137977892,-7.0018326042689));
#33415=CARTESIAN_POINT('Ctrl Pts',(11.2941025393094,6.27655372243322,-6.87381566679909));
#33416=CARTESIAN_POINT('Ctrl Pts',(11.3821420721327,6.28965154729957,-6.7473877722308));
#33417=CARTESIAN_POINT('Ctrl Pts',(11.470181604956,6.30274937216593,-6.6209598776625));
#33418=CARTESIAN_POINT('Ctrl Pts',(11.5534442861599,6.31535267924435,-6.49612068475505));
#33419=CARTESIAN_POINT('Ctrl Pts',(11.6323087423303,6.32744833334101,-6.37312202145236));
#33420=CARTESIAN_POINT('Ctrl Pts',(11.7139317330224,6.3399670713085,-6.24582108973488));
#33421=CARTESIAN_POINT('Ctrl Pts',(11.7908429946487,6.35194202164803,-6.12049296792028));
#33422=CARTESIAN_POINT('Ctrl Pts',(11.8634519252431,6.36338559571308,-5.99735692790288));
#33423=CARTESIAN_POINT('Ctrl Pts',(11.9311530660119,6.37405567461845,-5.88254391095459));
#33424=CARTESIAN_POINT('Ctrl Pts',(11.9951137821112,6.38426378322768,-5.769635897331));
#33425=CARTESIAN_POINT('Ctrl Pts',(12.0556513233948,6.39401998244428,-5.65877256262166));
#33426=CARTESIAN_POINT('Ctrl Pts',(12.1038652840376,6.40179011970257,-5.57047759154957));
#33427=CARTESIAN_POINT('Ctrl Pts',(12.1499093874645,6.40927360994193,-5.48348278526444));
#33428=CARTESIAN_POINT('Ctrl Pts',(12.1941193727415,6.41650884040827,-5.39746657064736));
#33429=CARTESIAN_POINT('Ctrl Pts',(12.239347841141,6.4239107517742,-5.30946876607293));
#33430=CARTESIAN_POINT('Ctrl Pts',(12.2826567466982,6.43105283309077,-5.22249493248192));
#33431=CARTESIAN_POINT('Ctrl Pts',(12.3243602954384,6.4379761862191,-5.13616992754827));
#33432=CARTESIAN_POINT('Ctrl Pts',(12.3479705506366,6.44189580790898,-5.08729745846498));
#33433=CARTESIAN_POINT('Ctrl Pts',(12.371065438676,6.44574532280715,-5.03863241735876));
#33434=CARTESIAN_POINT('Ctrl Pts',(12.3936956904151,6.44953218929337,-4.99010290224972));
#33435=CARTESIAN_POINT('Ctrl Pts',(12.4316423719943,6.45588205311251,-4.908728020597));
#33436=CARTESIAN_POINT('Ctrl Pts',(12.4682836359117,6.46205576845061,-4.82773956322418));
#33437=CARTESIAN_POINT('Ctrl Pts',(12.5038861066545,6.46808556494792,-4.74664939765116));
#33438=CARTESIAN_POINT('Ctrl Pts',(12.5395883311841,6.47413225620062,-4.6653320273106));
#33439=CARTESIAN_POINT('Ctrl Pts',(12.574245978718,6.48003422099657,-4.58391218210168));
#33440=CARTESIAN_POINT('Ctrl Pts',(12.6080804843132,6.48582396064637,-4.50187569469749));
#33441=CARTESIAN_POINT('Ctrl Pts',(12.6309096503538,6.48973047340522,-4.44652319111007));
#33442=CARTESIAN_POINT('Ctrl Pts',(12.6533631014863,6.49358589443462,-4.39088950817029));
#33443=CARTESIAN_POINT('Ctrl Pts',(12.6754964142268,6.4974002074343,-4.33481171082529));
#33444=CARTESIAN_POINT('Ctrl Pts',(12.7269620283516,6.50626946091183,-4.20441648653281));
#33445=CARTESIAN_POINT('Ctrl Pts',(12.7766868579223,6.5149164508941,-4.07162023955325));
#33446=CARTESIAN_POINT('Ctrl Pts',(12.8243735059259,6.52326975856373,-3.93678051396021));
#33447=CARTESIAN_POINT('Ctrl Pts',(12.8578991816006,6.52914247756301,-3.84198263871521));
#33448=CARTESIAN_POINT('Ctrl Pts',(12.8904183033638,6.53487003912974,-3.74617535806888));
#33449=CARTESIAN_POINT('Ctrl Pts',(12.9218408197293,6.5404276259437,-3.64949082505811));
#33450=CARTESIAN_POINT('Ctrl Pts',(12.9562541218577,6.54651418221784,-3.5436038869485));
#33451=CARTESIAN_POINT('Ctrl Pts',(12.989350143959,6.5523968676152,-3.4366610057836));
#33452=CARTESIAN_POINT('Ctrl Pts',(13.0209525658403,6.5580429985623,-3.32912472845405));
#33453=CARTESIAN_POINT('Ctrl Pts',(13.0525173160842,6.56368239904426,-3.22171663964358));
#33454=CARTESIAN_POINT('Ctrl Pts',(13.0825919425141,6.56908580870885,-3.11371679794506));
#33455=CARTESIAN_POINT('Ctrl Pts',(13.1110505414873,6.57422066072457,-3.00560147409868));
#33456=CARTESIAN_POINT('Ctrl Pts',(13.1171211402712,6.57531599315578,-2.98253903331994));
#33457=CARTESIAN_POINT('Ctrl Pts',(13.1231183881254,6.57639910552087,-2.95947138618505));
#33458=CARTESIAN_POINT('Ctrl Pts',(13.1290413604535,6.57746968171617,-2.93640323022847));
#33459=CARTESIAN_POINT('Ctrl Pts',(13.1676212352864,6.58444298723336,-2.786146480723));
#33460=CARTESIAN_POINT('Ctrl Pts',(13.2030547578354,6.59088442080034,-2.63586799647866));
#33461=CARTESIAN_POINT('Ctrl Pts',(13.2354636382202,6.59679996185767,-2.48535015240714));
#33462=CARTESIAN_POINT('Ctrl Pts',(13.2547085157596,6.60031269854823,-2.39597040703327));
#33463=CARTESIAN_POINT('Ctrl Pts',(13.2728859159242,6.60363999702594,-2.30650590690212));
#33464=CARTESIAN_POINT('Ctrl Pts',(13.2900130167678,6.60678310931848,-2.21690855187006));
#33465=CARTESIAN_POINT('Ctrl Pts',(13.3222777813736,6.61270423859626,-2.04812122494202));
#33466=CARTESIAN_POINT('Ctrl Pts',(13.3508170882143,6.61797171624897,-1.87886546720217));
#33467=CARTESIAN_POINT('Ctrl Pts',(13.3756691945126,6.62257209353774,-1.70896916413712));
#33468=CARTESIAN_POINT('Ctrl Pts',(13.386225408693,6.62452615599781,-1.63680378136887));
#33469=CARTESIAN_POINT('Ctrl Pts',(13.3961157384593,6.62635985874055,-1.5645227116085));
#33470=CARTESIAN_POINT('Ctrl Pts',(13.4053402988285,6.62807217110335,-1.49211235716791));
#33471=CARTESIAN_POINT('Ctrl Pts',(13.4362819019681,6.63381571740367,-1.2492289718761));
#33472=CARTESIAN_POINT('Ctrl Pts',(13.4597283165912,6.63819349065334,-1.00489014817131));
#33473=CARTESIAN_POINT('Ctrl Pts',(13.4755417506912,6.64114854912334,-0.759589252947098));
#33474=CARTESIAN_POINT('Ctrl Pts',(13.4865389940783,6.64320360541361,-0.588997992957664));
#33475=CARTESIAN_POINT('Ctrl Pts',(13.4938417996689,6.64457059089948,-0.417941196048216));
#33476=CARTESIAN_POINT('Ctrl Pts',(13.4974195660371,6.64524136211976,-0.24683900869035));
#33477=CARTESIAN_POINT('Ctrl Pts',(13.4989864318914,6.64553512320223,-0.171905615231797));
#33478=CARTESIAN_POINT('Ctrl Pts',(13.4998395222726,6.64569535313262,-0.0969635614458784));
#33479=CARTESIAN_POINT('Ctrl Pts',(13.4999794142971,6.64572136789133,-0.0220482345393076));
#33480=CARTESIAN_POINT('Ctrl Pts',(13.5002684457918,6.64577511709272,0.132734634566845));
#33481=CARTESIAN_POINT('Ctrl Pts',(13.4975093177643,6.64525593039062,0.287404480942835));
#33482=CARTESIAN_POINT('Ctrl Pts',(13.4917413597792,6.64417678722204,0.441539403733856));
#33483=CARTESIAN_POINT('Ctrl Pts',(13.4883430531217,6.64354098865631,0.532351045500931));
#33484=CARTESIAN_POINT('Ctrl Pts',(13.4839013085648,6.6427108174116,0.622977047436292));
#33485=CARTESIAN_POINT('Ctrl Pts',(13.4784325941184,6.64168892795466,0.713331975483202));
#33486=CARTESIAN_POINT('Ctrl Pts',(13.4653273546151,6.63924006977958,0.929858726693208));
#33487=CARTESIAN_POINT('Ctrl Pts',(13.4463315506767,6.63569022305755,1.14482941200399));
#33488=CARTESIAN_POINT('Ctrl Pts',(13.4216193971161,6.6310961576815,1.35823058592934));
#33489=CARTESIAN_POINT('Ctrl Pts',(13.4185164456516,6.63051930945774,1.38502604442876));
#33490=CARTESIAN_POINT('Ctrl Pts',(13.4153233038083,6.62992599780766,1.41179677541527));
#33491=CARTESIAN_POINT('Ctrl Pts',(13.4120402606657,6.62931633511701,1.43854276628595));
#33492=CARTESIAN_POINT('Ctrl Pts',(13.3926244347943,6.6257108069141,1.59671781271477));
#33493=CARTESIAN_POINT('Ctrl Pts',(13.3700688387817,6.6215333999691,1.75402610638057));
#33494=CARTESIAN_POINT('Ctrl Pts',(13.3443776216534,6.61679181905033,1.91069524068469));
#33495=CARTESIAN_POINT('Ctrl Pts',(13.3311274780926,6.61434636745629,1.99149672668338));
#33496=CARTESIAN_POINT('Ctrl Pts',(13.3170424290057,6.61175084898136,2.07212813769992));
#33497=CARTESIAN_POINT('Ctrl Pts',(13.3021176699024,6.60900632060681,2.15262002709032));
#33498=CARTESIAN_POINT('Ctrl Pts',(13.282699452721,6.60543548588387,2.2573459378208));
#33499=CARTESIAN_POINT('Ctrl Pts',(13.2618549081864,6.60161240813343,2.36183523166039));
#33500=CARTESIAN_POINT('Ctrl Pts',(13.2397008743149,6.59756647754478,2.46558881488019));
#33501=CARTESIAN_POINT('Ctrl Pts',(13.2174151238934,6.59349649192299,2.56995926381932));
#33502=CARTESIAN_POINT('Ctrl Pts',(13.1938043422287,6.58920099564749,2.67358500413981));
#33503=CARTESIAN_POINT('Ctrl Pts',(13.1690386693525,6.58470990624757,2.77597094466383));
#33504=CARTESIAN_POINT('Ctrl Pts',(13.1628121938078,6.58358077648569,2.80171236335964));
#33505=CARTESIAN_POINT('Ctrl Pts',(13.1565129652826,6.58243928332459,2.82737548734641));
#33506=CARTESIAN_POINT('Ctrl Pts',(13.1501441803073,6.58128590221134,2.85295260111209));
#33507=CARTESIAN_POINT('Ctrl Pts',(13.1276352530914,6.57720955615299,2.94334871189015));
#33508=CARTESIAN_POINT('Ctrl Pts',(13.1042526433213,6.57298471795363,3.03267264726758));
#33509=CARTESIAN_POINT('Ctrl Pts',(13.0802238691335,6.56866270647682,3.12036412844092));
#33510=CARTESIAN_POINT('Ctrl Pts',(13.0555891306266,6.56423170131094,3.21026703780761));
#33511=CARTESIAN_POINT('Ctrl Pts',(13.0302753666322,6.55969855998359,3.29845393225428));
#33512=CARTESIAN_POINT('Ctrl Pts',(13.0045795814911,6.55511858261199,3.38434033500869));
#33513=CARTESIAN_POINT('Ctrl Pts',(12.99200037201,6.55287648358838,3.42638548155284));
#33514=CARTESIAN_POINT('Ctrl Pts',(12.9793303739806,6.5506231601651,3.46787961563997));
#33515=CARTESIAN_POINT('Ctrl Pts',(12.9666085639724,6.54836510018653,3.50875595858229));
#33516=CARTESIAN_POINT('Ctrl Pts',(12.940792431796,6.5437828611159,3.5917055602194));
#33517=CARTESIAN_POINT('Ctrl Pts',(12.9147681836767,6.53918111699148,3.67211234175013));
#33518=CARTESIAN_POINT('Ctrl Pts',(12.8885057287866,6.53455169676247,3.75050983225192));
#33519=CARTESIAN_POINT('Ctrl Pts',(12.8615210754612,6.52979497083945,3.83106319680337));
#33520=CARTESIAN_POINT('Ctrl Pts',(12.8342847721211,6.52500902573734,3.90949538777508));
#33521=CARTESIAN_POINT('Ctrl Pts',(12.8067104903906,6.52018499760443,3.98637282662223));
#33522=CARTESIAN_POINT('Ctrl Pts',(12.7945330216198,6.51805459027371,4.02032376031806));
#33523=CARTESIAN_POINT('Ctrl Pts',(12.7822889612338,6.51591675553747,4.05397129591668));
#33524=CARTESIAN_POINT('Ctrl Pts',(12.7699677834507,6.51377072994513,4.08736337382604));
#33525=CARTESIAN_POINT('Ctrl Pts',(12.7427108058986,6.50902328027543,4.16123351303019));
#33526=CARTESIAN_POINT('Ctrl Pts',(12.7150811577462,6.50423574575775,4.23385109131939));
#33527=CARTESIAN_POINT('Ctrl Pts',(12.6868914513244,6.49937095059352,4.30582894702377));
#33528=CARTESIAN_POINT('Ctrl Pts',(12.6585644801614,6.494482467178,4.37815728604268));
#33529=CARTESIAN_POINT('Ctrl Pts',(12.6296718796146,6.48951596887022,4.44983980209247));
#33530=CARTESIAN_POINT('Ctrl Pts',(12.5999743835185,6.48443373416024,4.52148008523258));
#33531=CARTESIAN_POINT('Ctrl Pts',(12.5861748224671,6.48207216778673,4.5547692372113));
#33532=CARTESIAN_POINT('Ctrl Pts',(12.5722007878739,6.47968561172406,4.58804900037526));
#33533=CARTESIAN_POINT('Ctrl Pts',(12.5580247409487,6.47727028132517,4.62137845204915));
#33534=CARTESIAN_POINT('Ctrl Pts',(12.5168376484799,6.47025277940755,4.71821385441987));
#33535=CARTESIAN_POINT('Ctrl Pts',(12.4739402348053,6.46299238320348,4.81546529168791));
#33536=CARTESIAN_POINT('Ctrl Pts',(12.4294801907888,6.45552630928657,4.91263509352366));
#33537=CARTESIAN_POINT('Ctrl Pts',(12.3929332080852,6.44938905773091,4.9925104770408));
#33538=CARTESIAN_POINT('Ctrl Pts',(12.355331219531,6.44311282674947,5.07233092004027));
#33539=CARTESIAN_POINT('Ctrl Pts',(12.3167808262493,6.43671828828554,5.15182971976806));
#33540=CARTESIAN_POINT('Ctrl Pts',(12.2651233822605,6.42814962051294,5.25835794022213));
#33541=CARTESIAN_POINT('Ctrl Pts',(12.211761199467,6.41936852050751,5.36431060995521));
#33542=CARTESIAN_POINT('Ctrl Pts',(12.1569061803181,6.41042804776098,5.46926381567329));
#33543=CARTESIAN_POINT('Ctrl Pts',(12.1210244044939,6.40457990398431,5.53791582706711));
#33544=CARTESIAN_POINT('Ctrl Pts',(12.0845048538408,6.3986635688782,5.606140646506));
#33545=CARTESIAN_POINT('Ctrl Pts',(12.0474174600384,6.3926938927608,5.67382535260096));
#33546=CARTESIAN_POINT('Ctrl Pts',(11.9926822297006,6.3838835784241,5.77371746144518));
#33547=CARTESIAN_POINT('Ctrl Pts',(11.9367157922521,6.37495708110681,5.8724355292054));
#33548=CARTESIAN_POINT('Ctrl Pts',(11.8793286684131,6.36589527473159,5.97035005230608));
#33549=CARTESIAN_POINT('Ctrl Pts',(11.8383864053749,6.35943022063242,6.04020617841705));
#33550=CARTESIAN_POINT('Ctrl Pts',(11.796720037908,6.35289629470045,6.10965282806653));
#33551=CARTESIAN_POINT('Ctrl Pts',(11.7542467422086,6.34628655152287,6.17881640065429));
#33552=CARTESIAN_POINT('Ctrl Pts',(11.6787939476812,6.33454450076735,6.30168383406892));
#33553=CARTESIAN_POINT('Ctrl Pts',(11.6007955847598,6.32256318084416,6.42365766571776));
#33554=CARTESIAN_POINT('Ctrl Pts',(11.5200360405655,6.31034401507871,6.54492039630344));
#33555=CARTESIAN_POINT('Ctrl Pts',(11.4916148586905,6.30604380343135,6.58759560150689));
#33556=CARTESIAN_POINT('Ctrl Pts',(11.462851342409,6.3017141345399,6.63018243833174));
#33557=CARTESIAN_POINT('Ctrl Pts',(11.4337349306691,6.29735507044112,6.67268784821382));
#33558=CARTESIAN_POINT('Ctrl Pts',(11.3778091956261,6.28898234010605,6.75433067948669));
#33559=CARTESIAN_POINT('Ctrl Pts',(11.3205862334272,6.28050116110226,6.8356750631076));
#33560=CARTESIAN_POINT('Ctrl Pts',(11.2616761282475,6.27186760351598,6.91716968355268));
#33561=CARTESIAN_POINT('Ctrl Pts',(11.2063472398295,6.26375889036932,6.99371014715426));
#33562=CARTESIAN_POINT('Ctrl Pts',(11.1495296754629,6.25551576207198,7.07038306740363));
#33563=CARTESIAN_POINT('Ctrl Pts',(11.0908602382651,6.24710182319922,7.14752688198067));
#33564=CARTESIAN_POINT('Ctrl Pts',(11.0870628011956,6.24655722272405,7.15252009130992));
#33565=CARTESIAN_POINT('Ctrl Pts',(11.0832575922087,6.24601190664599,7.15751526131866));
#33566=CARTESIAN_POINT('Ctrl Pts',(11.0794445071668,6.24546586509583,7.16251247866907));
#33567=CARTESIAN_POINT('Ctrl Pts',(11.0167202277328,6.23648362043076,7.24471543350426));
#33568=CARTESIAN_POINT('Ctrl Pts',(10.9518690113909,6.22730506726939,7.32747369271627));
#33569=CARTESIAN_POINT('Ctrl Pts',(10.8845241565944,6.21790432002736,7.41100156356173));
#33570=CARTESIAN_POINT('Ctrl Pts',(10.8171793017979,6.20850357278533,7.49452943440719));
#33571=CARTESIAN_POINT('Ctrl Pts',(10.7473408580157,6.19888063146263,7.57882731379565));
#33572=CARTESIAN_POINT('Ctrl Pts',(10.6746067396372,6.18900961047489,7.66406851881595));
#33573=CARTESIAN_POINT('Ctrl Pts',(10.6092476574337,6.18013948340723,7.74066650405669));
#33574=CARTESIAN_POINT('Ctrl Pts',(10.5415523622487,6.17106903523843,7.81802449638722));
#33575=CARTESIAN_POINT('Ctrl Pts',(10.4711322854565,6.1617777234388,7.8963118222002));
#33576=CARTESIAN_POINT('Ctrl Pts',(10.4026106648622,6.15273689629178,7.97248859849848));
#33577=CARTESIAN_POINT('Ctrl Pts',(10.3315091069494,6.14348695352644,8.04954548082737));
#33578=CARTESIAN_POINT('Ctrl Pts',(10.2574401066208,6.13400896964473,8.12759869082826));
#33579=CARTESIAN_POINT('Ctrl Pts',(10.2382091260077,6.13154814361128,8.14786411579227));
#33580=CARTESIAN_POINT('Ctrl Pts',(10.2187779530672,6.12907194512913,8.16819648124987));
#33581=CARTESIAN_POINT('Ctrl Pts',(10.199139479305,6.12658004295878,8.18859733758286));
#33582=CARTESIAN_POINT('Ctrl Pts',(10.0955471544311,6.11343533821694,8.29621120628442));
#33583=CARTESIAN_POINT('Ctrl Pts',(9.98618552590945,6.09985367380175,8.40572955822586));
#33584=CARTESIAN_POINT('Ctrl Pts',(9.87093205162319,6.0859343295064,8.51640709901712));
#33585=CARTESIAN_POINT('Ctrl Pts',(9.79369900175001,6.07660677197443,8.59057374848871));
#33586=CARTESIAN_POINT('Ctrl Pts',(9.71382101063564,6.06712757802916,8.66526037192818));
#33587=CARTESIAN_POINT('Ctrl Pts',(9.63127322650993,6.0575266227,8.74023722148102));
#33588=CARTESIAN_POINT('',(9.631273226509,6.0575266227,8.74023722148));
#33589=CARTESIAN_POINT('',(13.3,5.241201401137,2.164009824691));
#33590=CARTESIAN_POINT('',(13.3,5.241201401137,-2.164009824691));
#33591=CARTESIAN_POINT('Ctrl Pts',(13.300000000001,5.24120140113708,2.16400982469131));
#33592=CARTESIAN_POINT('Ctrl Pts',(13.3180935597627,5.38692580429823,2.06695933461524));
#33593=CARTESIAN_POINT('Ctrl Pts',(13.3374024258682,5.52055417312555,1.95640108904449));
#33594=CARTESIAN_POINT('Ctrl Pts',(13.3922809876029,5.86870480663107,1.60825045553898));
#33595=CARTESIAN_POINT('Ctrl Pts',(13.4307628143448,6.06863168929127,1.3166037527462));
#33596=CARTESIAN_POINT('Ctrl Pts',(13.4849916924495,6.33430849895895,0.676325134116298));
#33597=CARTESIAN_POINT('Ctrl Pts',(13.500000000001,6.4,0.327606623932291));
#33598=CARTESIAN_POINT('Ctrl Pts',(13.500000000001,6.4,-0.327606623932292));
#33599=CARTESIAN_POINT('Ctrl Pts',(13.4849916924495,6.33430849895895,-0.676325134116299));
#33600=CARTESIAN_POINT('Ctrl Pts',(13.4307628143448,6.06863168929127,-1.31660375274621));
#33601=CARTESIAN_POINT('Ctrl Pts',(13.3922809876029,5.86870480663107,-1.60825045553898));
#33602=CARTESIAN_POINT('Ctrl Pts',(13.3374024258682,5.52055417312555,-1.95640108904449));
#33603=CARTESIAN_POINT('Ctrl Pts',(13.3180935597627,5.38692580429823,-2.06695933461524));
#33604=CARTESIAN_POINT('Ctrl Pts',(13.300000000001,5.24120140113708,-2.16400982469131));
#33605=CARTESIAN_POINT('',(13.3,2.358798598863,-2.164009824691));
#33606=CARTESIAN_POINT('Ctrl Pts',(13.3000000000008,5.24120140113749,-2.16400982469205));
#33607=CARTESIAN_POINT('Ctrl Pts',(13.2864350300733,5.10747808862643,-2.23676980098582));
#33608=CARTESIAN_POINT('Ctrl Pts',(13.2739820406732,4.96621350744257,-2.29979178340204));
#33609=CARTESIAN_POINT('Ctrl Pts',(13.2394248960124,4.48771447089005,-2.46983579880371));
#33610=CARTESIAN_POINT('Ctrl Pts',(13.2265218318602,4.13149059985939,-2.52652183186019));
#33611=CARTESIAN_POINT('Ctrl Pts',(13.2265218318602,3.46850940014061,-2.52652183186019));
#33612=CARTESIAN_POINT('Ctrl Pts',(13.2394248960124,3.11228552910995,-2.46983579880371));
#33613=CARTESIAN_POINT('Ctrl Pts',(13.2739820406732,2.63378649255743,-2.29979178340204));
#33614=CARTESIAN_POINT('Ctrl Pts',(13.2864350300733,2.49252191137357,-2.23676980098582));
#33615=CARTESIAN_POINT('Ctrl Pts',(13.3000000000008,2.35879859886251,-2.16400982469205));
#33616=CARTESIAN_POINT('',(13.3,2.358798598863,2.164009824691));
#33617=CARTESIAN_POINT('Ctrl Pts',(13.300000000001,2.35879859886292,-2.16400982469131));
#33618=CARTESIAN_POINT('Ctrl Pts',(13.3180935597627,2.21307419570177,-2.06695933461524));
#33619=CARTESIAN_POINT('Ctrl Pts',(13.3374024258682,2.07944582687445,-1.95640108904449));
#33620=CARTESIAN_POINT('Ctrl Pts',(13.3922809876029,1.73129519336893,-1.60825045553898));
#33621=CARTESIAN_POINT('Ctrl Pts',(13.4307628143448,1.53136831070873,-1.3166037527462));
#33622=CARTESIAN_POINT('Ctrl Pts',(13.4849916924495,1.26569150104105,-0.676325134116298));
#33623=CARTESIAN_POINT('Ctrl Pts',(13.500000000001,1.2,-0.327606623932291));
#33624=CARTESIAN_POINT('Ctrl Pts',(13.500000000001,1.2,0.327606623932291));
#33625=CARTESIAN_POINT('Ctrl Pts',(13.4849916924495,1.26569150104105,0.676325134116298));
#33626=CARTESIAN_POINT('Ctrl Pts',(13.4307628143448,1.53136831070873,1.3166037527462));
#33627=CARTESIAN_POINT('Ctrl Pts',(13.3922809876029,1.73129519336893,1.60825045553898));
#33628=CARTESIAN_POINT('Ctrl Pts',(13.3374024258682,2.07944582687445,1.95640108904449));
#33629=CARTESIAN_POINT('Ctrl Pts',(13.3180935597627,2.21307419570177,2.06695933461524));
#33630=CARTESIAN_POINT('Ctrl Pts',(13.300000000001,2.35879859886292,2.16400982469131));
#33631=CARTESIAN_POINT('Ctrl Pts',(13.3000000000008,2.35879859886251,2.16400982469205));
#33632=CARTESIAN_POINT('Ctrl Pts',(13.2864350300733,2.49252191137357,2.23676980098582));
#33633=CARTESIAN_POINT('Ctrl Pts',(13.2739820406732,2.63378649255743,2.29979178340204));
#33634=CARTESIAN_POINT('Ctrl Pts',(13.2394248960124,3.11228552910995,2.46983579880371));
#33635=CARTESIAN_POINT('Ctrl Pts',(13.2265218318602,3.46850940014061,2.52652183186019));
#33636=CARTESIAN_POINT('Ctrl Pts',(13.2265218318602,3.8,2.52652183186019));
#33637=CARTESIAN_POINT('Ctrl Pts',(13.2265218318602,4.13149059985939,2.52652183186019));
#33638=CARTESIAN_POINT('Ctrl Pts',(13.2394248960124,4.48771447089005,2.46983579880371));
#33639=CARTESIAN_POINT('Ctrl Pts',(13.2739820406732,4.96621350744257,2.29979178340204));
#33640=CARTESIAN_POINT('Ctrl Pts',(13.2864350300733,5.10747808862643,2.23676980098582));
#33641=CARTESIAN_POINT('Ctrl Pts',(13.3000000000008,5.24120140113749,2.16400982469205));
#33642=CARTESIAN_POINT('Origin',(13.875,3.8,0.));
#33643=CARTESIAN_POINT('',(13.3000000000008,6.40000000000084,3.18408167778415E-16));
#33644=CARTESIAN_POINT('Origin',(13.3,3.8,0.));
#33645=CARTESIAN_POINT('Origin',(13.3,3.8,0.));
#33646=CARTESIAN_POINT('Origin',(13.875,3.8,0.));
#33647=CARTESIAN_POINT('Origin',(13.3,3.8,0.));
#33648=CARTESIAN_POINT('Origin',(12.625,3.8,0.));
#33649=CARTESIAN_POINT('',(11.95,2.55,0.));
#33650=CARTESIAN_POINT('',(11.95,5.05,1.53080849893419E-16));
#33651=CARTESIAN_POINT('Origin',(11.95,3.8,0.));
#33652=CARTESIAN_POINT('',(12.625,5.725,2.35744508835865E-16));
#33653=CARTESIAN_POINT('Origin',(11.95,3.8,0.));
#33654=CARTESIAN_POINT('Origin',(13.875,3.8,0.));
#33655=CARTESIAN_POINT('',(6.,2.55,0.));
#33656=CARTESIAN_POINT('',(13.875,2.55,1.53080849893419E-16));
#33657=CARTESIAN_POINT('Origin',(6.,3.8,0.));
#33658=CARTESIAN_POINT('Origin',(6.,0.,0.));
#33659=CARTESIAN_POINT('',(6.,3.8,-2.5));
#33660=CARTESIAN_POINT('Origin',(6.,3.8,0.));
#33661=CARTESIAN_POINT('Origin',(-1.,3.8,0.));
#33662=CARTESIAN_POINT('',(-1.,3.8,-2.5));
#33663=CARTESIAN_POINT('',(-1.,3.8,-2.5));
#33664=CARTESIAN_POINT('Origin',(-1.,3.8,0.));
#33665=CARTESIAN_POINT('Origin',(-1.,0.,0.));
#33666=CARTESIAN_POINT('Ctrl Pts',(9.485442650021,5.952891693689,-8.860081849749));
#33667=CARTESIAN_POINT('Ctrl Pts',(9.534636054532,5.959034860707,-8.816948875496));
#33668=CARTESIAN_POINT('Ctrl Pts',(9.870556912557,6.001493104786,-8.517415431551));
#33669=CARTESIAN_POINT('Ctrl Pts',(10.43177183646,6.078357198741,-7.956077122609));
#33670=CARTESIAN_POINT('Ctrl Pts',(11.09306532507,6.178684101018,-7.159219782959));
#33671=CARTESIAN_POINT('Ctrl Pts',(11.62422729818,6.265537517347,-6.399074799972));
#33672=CARTESIAN_POINT('Ctrl Pts',(12.04988106646,6.339153757363,-5.681632943686));
#33673=CARTESIAN_POINT('Ctrl Pts',(12.39479790134,6.401396123129,-5.00006532987));
#33674=CARTESIAN_POINT('Ctrl Pts',(12.68337078438,6.455239570641,-4.329650458296));
#33675=CARTESIAN_POINT('Ctrl Pts',(12.92973905293,6.502503926928,-3.644849379563));
#33676=CARTESIAN_POINT('Ctrl Pts',(13.13522025712,6.54285063425,-2.938234819852));
#33677=CARTESIAN_POINT('Ctrl Pts',(13.29643076178,6.575090237291,-2.218196523314));
#33678=CARTESIAN_POINT('Ctrl Pts',(13.41211690496,6.598540633102,-1.491642412231));
#33679=CARTESIAN_POINT('Ctrl Pts',(13.48237446627,6.612910993203,-0.7590144441822));
#33680=CARTESIAN_POINT('Ctrl Pts',(13.50678376795,6.61792644257,-0.02280129264716));
#33681=CARTESIAN_POINT('Ctrl Pts',(13.48527073568,6.613505521845,0.7109530505647));
#33682=CARTESIAN_POINT('Ctrl Pts',(13.41877759765,6.599899443318,1.436789723415));
#33683=CARTESIAN_POINT('Ctrl Pts',(13.30878668262,6.57758461397,2.150825299771));
#33684=CARTESIAN_POINT('Ctrl Pts',(13.15883216383,6.547550459594,2.841355547203));
#33685=CARTESIAN_POINT('Ctrl Pts',(12.97830256373,6.511998053041,3.485919540467));
#33686=CARTESIAN_POINT('Ctrl Pts',(12.77805158862,6.4733296184,4.07466488761));
#33687=CARTESIAN_POINT('Ctrl Pts',(12.56058971477,6.432225904256,4.62210341788));
#33688=CARTESIAN_POINT('Ctrl Pts',(12.31982924549,6.387800142595,5.150989661439));
#33689=CARTESIAN_POINT('Ctrl Pts',(12.05172287785,6.33968980881,5.670016802825));
#33690=CARTESIAN_POINT('Ctrl Pts',(11.75719282679,6.28849176907,6.176788355475));
#33691=CARTESIAN_POINT('Ctrl Pts',(11.43474145404,6.234418256753,6.673056312275));
#33692=CARTESIAN_POINT('Ctrl Pts',(11.07576023228,6.176643934304,7.168730439045));
#33693=CARTESIAN_POINT('Ctrl Pts',(10.66606024847,6.113822407882,7.675609305722));
#33694=CARTESIAN_POINT('Ctrl Pts',(10.1860426261,6.04445748388,8.20437686418));
#33695=CARTESIAN_POINT('Ctrl Pts',(9.780289236406,5.990083979416,8.597903917999));
#33696=CARTESIAN_POINT('Ctrl Pts',(9.534645032455,5.959035996825,8.816940677232));
#33697=CARTESIAN_POINT('Ctrl Pts',(9.485454696088,5.952893121937,8.860071898555));
#33698=CARTESIAN_POINT('Ctrl Pts',(9.501283522908,6.25924448941,-8.919478697923));
#33699=CARTESIAN_POINT('Ctrl Pts',(9.550507806299,6.265441721484,-8.876058641547));
#33700=CARTESIAN_POINT('Ctrl Pts',(9.886639439875,6.308272767042,-8.574531191516));
#33701=CARTESIAN_POINT('Ctrl Pts',(10.44820557707,6.385801787616,-8.009451327147));
#33702=CARTESIAN_POINT('Ctrl Pts',(11.10991201118,6.486981590413,-7.207272704089));
#33703=CARTESIAN_POINT('Ctrl Pts',(11.64140552514,6.574564764989,-6.442044024142));
#33704=CARTESIAN_POINT('Ctrl Pts',(12.06732516279,6.648794492034,-5.719798235741));
#33705=CARTESIAN_POINT('Ctrl Pts',(12.41245772277,6.711552517154,-5.033662382996));
#33706=CARTESIAN_POINT('Ctrl Pts',(12.70121138752,6.76584007241,-4.358750315406));
#33707=CARTESIAN_POINT('Ctrl Pts',(12.94773428354,6.813492891526,-3.669352220712));
#33708=CARTESIAN_POINT('Ctrl Pts',(13.15334470394,6.854170257082,-2.957991205558));
#33709=CARTESIAN_POINT('Ctrl Pts',(13.31465676988,6.88667349715,-2.233113750652));
#33710=CARTESIAN_POINT('Ctrl Pts',(13.43041590509,6.910315353154,-1.50167473912));
#33711=CARTESIAN_POINT('Ctrl Pts',(13.50071784403,6.924802918115,-0.7641196938934));
#33712=CARTESIAN_POINT('Ctrl Pts',(13.52514257268,6.929859252279,-0.02295466127787));
#33713=CARTESIAN_POINT('Ctrl Pts',(13.50361594369,6.925402293752,0.7157350447915));
#33714=CARTESIAN_POINT('Ctrl Pts',(13.43708080358,6.911685249168,1.446453187537));
#33715=CARTESIAN_POINT('Ctrl Pts',(13.32702048293,6.889188248829,2.165289624432));
#33716=CARTESIAN_POINT('Ctrl Pts',(13.17697147856,6.858908536401,2.860460929475));
#33717=CARTESIAN_POINT('Ctrl Pts',(12.99632832114,6.823064867231,3.50935495712));
#33718=CARTESIAN_POINT('Ctrl Pts',(12.79595159765,6.784078877253,4.10205323945));
#33719=CARTESIAN_POINT('Ctrl Pts',(12.57835337903,6.742636698209,4.653165293559));
#33720=CARTESIAN_POINT('Ctrl Pts',(12.33744216991,6.697843973672,5.185598399135));
#33721=CARTESIAN_POINT('Ctrl Pts',(12.06916814928,6.649334755299,5.708103930231));
#33722=CARTESIAN_POINT('Ctrl Pts',(11.77445409949,6.597710356767,6.218269250769));
#33723=CARTESIAN_POINT('Ctrl Pts',(11.45180140757,6.543184206245,6.717858020621));
#33724=CARTESIAN_POINT('Ctrl Pts',(11.09259610083,6.484923277324,7.216846154425));
#33725=CARTESIAN_POINT('Ctrl Pts',(10.68264028709,6.421568601756,7.727110711857));
#33726=CARTESIAN_POINT('Ctrl Pts',(10.20232262365,6.351609196432,8.259406264638));
#33727=CARTESIAN_POINT('Ctrl Pts',(9.796315124191,6.296763464549,8.655555492532));
#33728=CARTESIAN_POINT('Ctrl Pts',(9.550516790186,6.265442867547,8.876050388876));
#33729=CARTESIAN_POINT('Ctrl Pts',(9.501295577027,6.259245930234,8.91946868085));
#33730=CARTESIAN_POINT('Ctrl Pts',(9.35997989658,6.507098481045,-8.792071395616));
#33731=CARTESIAN_POINT('Ctrl Pts',(9.408273439289,6.513077227545,-8.749258512838));
#33732=CARTESIAN_POINT('Ctrl Pts',(9.738051948008,6.554400160203,-8.451947043545));
#33733=CARTESIAN_POINT('Ctrl Pts',(10.28903193377,6.629221549912,-7.894765291821));
#33734=CARTESIAN_POINT('Ctrl Pts',(10.93829150539,6.726898620283,-7.10382265491));
#33735=CARTESIAN_POINT('Ctrl Pts',(11.45979182787,6.811464936495,-6.3493547208));
#33736=CARTESIAN_POINT('Ctrl Pts',(11.87769772134,6.883144779298,-5.637314350587));
#33737=CARTESIAN_POINT('Ctrl Pts',(12.21632796884,6.943749925877,-4.960922641443));
#33738=CARTESIAN_POINT('Ctrl Pts',(12.4996325731,6.9961762299,-4.295642816956));
#33739=CARTESIAN_POINT('Ctrl Pts',(12.74149474047,7.042195399749,-3.616131678469));
#33740=CARTESIAN_POINT('Ctrl Pts',(12.94321036984,7.08147790737,-2.915020481202));
#33741=CARTESIAN_POINT('Ctrl Pts',(13.10146121022,7.112866122033,-2.200631020283));
#33742=CARTESIAN_POINT('Ctrl Pts',(13.21502024463,7.135696584537,-1.479810217005));
#33743=CARTESIAN_POINT('Ctrl Pts',(13.28398456809,7.149686753743,-0.7529872864468));
#33744=CARTESIAN_POINT('Ctrl Pts',(13.30794430238,7.15456945535,-0.02262016733114));
#33745=CARTESIAN_POINT('Ctrl Pts',(13.28682750111,7.150265547977,0.7053073001723));
#33746=CARTESIAN_POINT('Ctrl Pts',(13.22155837359,7.137019453742,1.425391562183));
#33747=CARTESIAN_POINT('Ctrl Pts',(13.1135900535,7.115294579917,2.133790387283));
#33748=CARTESIAN_POINT('Ctrl Pts',(12.96638900092,7.086053660963,2.818899704123));
#33749=CARTESIAN_POINT('Ctrl Pts',(12.78916864978,7.051439169748,3.458437528109));
#33750=CARTESIAN_POINT('Ctrl Pts',(12.59258219107,7.013789778161,4.042624198806));
#33751=CARTESIAN_POINT('Ctrl Pts',(12.37909362994,6.973768350244,4.585852924676));
#33752=CARTESIAN_POINT('Ctrl Pts',(12.1427259698,6.930511582039,5.110699731971));
#33753=CARTESIAN_POINT('Ctrl Pts',(11.87950528854,6.883666724966,5.625789474164));
#33754=CARTESIAN_POINT('Ctrl Pts',(11.59033726588,6.833815414448,6.128740954401));
#33755=CARTESIAN_POINT('Ctrl Pts',(11.2737526677,6.781165017737,6.621289226868));
#33756=CARTESIAN_POINT('Ctrl Pts',(10.92130165418,6.724912967278,7.113266081009));
#33757=CARTESIAN_POINT('Ctrl Pts',(10.51905697905,6.663749998167,7.616378545751));
#33758=CARTESIAN_POINT('Ctrl Pts',(10.04778305149,6.596222248822,8.141226799633));
#33759=CARTESIAN_POINT('Ctrl Pts',(9.649434841825,6.543296109889,8.531838461027));
#33760=CARTESIAN_POINT('Ctrl Pts',(9.408282243416,6.513078333271,8.749250370185));
#33761=CARTESIAN_POINT('Ctrl Pts',(9.359991707996,6.507099872998,8.792061517141));
#33762=CARTESIAN_POINT('Ctrl Pts',(9.152731006141,6.53648541412,-8.560090306046));
#33763=CARTESIAN_POINT('Ctrl Pts',(9.199732900989,6.542114137906,-8.518386974692));
#33764=CARTESIAN_POINT('Ctrl Pts',(9.520694775513,6.581021399357,-8.228780423059));
#33765=CARTESIAN_POINT('Ctrl Pts',(10.05698368769,6.651510141599,-7.686038905367));
#33766=CARTESIAN_POINT('Ctrl Pts',(10.68896995904,6.743589556577,-6.915637669631));
#33767=CARTESIAN_POINT('Ctrl Pts',(11.19660209605,6.823339518226,-6.180829796028));
#33768=CARTESIAN_POINT('Ctrl Pts',(11.60338680859,6.890951834637,-5.487417482014));
#33769=CARTESIAN_POINT('Ctrl Pts',(11.93299338477,6.948125061152,-4.828793299445));
#33770=CARTESIAN_POINT('Ctrl Pts',(12.2087359823,6.997586031203,-4.18105837969));
#33771=CARTESIAN_POINT('Ctrl Pts',(12.44413016099,7.0410038186,-3.519536996875));
#33772=CARTESIAN_POINT('Ctrl Pts',(12.64044074188,7.078066211933,-2.837056522375));
#33773=CARTESIAN_POINT('Ctrl Pts',(12.79444332545,7.107680390949,-2.141713117333));
#33774=CARTESIAN_POINT('Ctrl Pts',(12.9049491405,7.129220290391,-1.440160498536));
#33775=CARTESIAN_POINT('Ctrl Pts',(12.97205717013,7.142419489043,-0.7328022253019));
#33776=CARTESIAN_POINT('Ctrl Pts',(12.99537160226,7.147026105496,-0.0220136976379));
#33777=CARTESIAN_POINT('Ctrl Pts',(12.97482354493,7.142965556986,0.686400021429));
#33778=CARTESIAN_POINT('Ctrl Pts',(12.91131134333,7.130468371904,1.38719829978));
#33779=CARTESIAN_POINT('Ctrl Pts',(12.80624622508,7.109971581401,2.076657613881));
#33780=CARTESIAN_POINT('Ctrl Pts',(12.66299745577,7.08238335636,2.743496037382));
#33781=CARTESIAN_POINT('Ctrl Pts',(12.49052714993,7.049725155911,3.366030037639));
#33782=CARTESIAN_POINT('Ctrl Pts',(12.299200682,7.01420385811,3.934734056953));
#33783=CARTESIAN_POINT('Ctrl Pts',(12.09141535314,6.97644542572,4.463610607139));
#33784=CARTESIAN_POINT('Ctrl Pts',(11.861353064,6.935636206461,4.974634253413));
#33785=CARTESIAN_POINT('Ctrl Pts',(11.60514522221,6.891444755714,5.476200276634));
#33786=CARTESIAN_POINT('Ctrl Pts',(11.32367377305,6.844421605485,5.965986216616));
#33787=CARTESIAN_POINT('Ctrl Pts',(11.0155102533,6.794764718208,6.445676711681));
#33788=CARTESIAN_POINT('Ctrl Pts',(10.67243260075,6.741720474333,6.924842172373));
#33789=CARTESIAN_POINT('Ctrl Pts',(10.28088916162,6.684059510856,7.414880816488));
#33790=CARTESIAN_POINT('Ctrl Pts',(9.822165799765,6.620420131763,7.926113063764));
#33791=CARTESIAN_POINT('Ctrl Pts',(9.434446872203,6.570566475392,8.306601436968));
#33792=CARTESIAN_POINT('Ctrl Pts',(9.199741455652,6.542115179046,8.518379035476));
#33793=CARTESIAN_POINT('Ctrl Pts',(9.15274248074,6.536486727296,8.560080681194));
#33794=CARTESIAN_POINT('Origin',(9.295100305717,6.057526619323,8.370118635987));
#33795=CARTESIAN_POINT('Ctrl Pts',(9.653942535497,6.031033711932,8.717909060576));
#33796=CARTESIAN_POINT('Ctrl Pts',(9.646944916628,6.030093928364,8.724648332143));
#33797=CARTESIAN_POINT('Ctrl Pts',(9.59719467314,6.023650265556,8.771170219865));
#33798=CARTESIAN_POINT('Ctrl Pts',(9.495042840547,6.013489241721,8.848779982819));
#33799=CARTESIAN_POINT('Ctrl Pts',(9.33375118979,6.004441014892,8.931245876486));
#33800=CARTESIAN_POINT('Ctrl Pts',(9.152585363009,6.001089741996,8.98551789411));
#33801=CARTESIAN_POINT('Ctrl Pts',(9.013899860845,6.003522469926,8.999282418285));
#33802=CARTESIAN_POINT('Ctrl Pts',(8.937785978944,6.00642658824,8.998158241186));
#33803=CARTESIAN_POINT('Ctrl Pts',(8.927957310455,6.006827995205,8.997866981941));
#33804=CARTESIAN_POINT('Ctrl Pts',(9.645773860495,6.31475659886,8.747934865266));
#33805=CARTESIAN_POINT('Ctrl Pts',(9.638958592229,6.313838584937,8.754518086709));
#33806=CARTESIAN_POINT('Ctrl Pts',(9.590505220355,6.307544168074,8.799962308943));
#33807=CARTESIAN_POINT('Ctrl Pts',(9.491021810395,6.297618091538,8.875768956116));
#33808=CARTESIAN_POINT('Ctrl Pts',(9.333955851884,6.288775548995,8.956311007241));
#33809=CARTESIAN_POINT('Ctrl Pts',(9.157544689065,6.285492132199,9.009313113419));
#33810=CARTESIAN_POINT('Ctrl Pts',(9.022499207939,6.287856157087,9.02275401755));
#33811=CARTESIAN_POINT('Ctrl Pts',(8.948380877393,6.290684710128,9.021654827436));
#33812=CARTESIAN_POINT('Ctrl Pts',(8.938809854365,6.291075723373,9.021370205509));
#33813=CARTESIAN_POINT('Ctrl Pts',(9.501656951024,6.529655143128,8.627454091879));
#33814=CARTESIAN_POINT('Ctrl Pts',(9.496360020516,6.528944036884,8.63258932645));
#33815=CARTESIAN_POINT('Ctrl Pts',(9.458705017816,6.524069354645,8.668034829828));
#33816=CARTESIAN_POINT('Ctrl Pts',(9.38144016242,6.516395155231,8.727123383244));
#33817=CARTESIAN_POINT('Ctrl Pts',(9.259559325096,6.509578980089,8.789847902424));
#33818=CARTESIAN_POINT('Ctrl Pts',(9.12273775328,6.507065811343,8.831104321855));
#33819=CARTESIAN_POINT('Ctrl Pts',(9.018000816625,6.508907798825,8.841565722931));
#33820=CARTESIAN_POINT('Ctrl Pts',(8.96049839471,6.511101044754,8.840709421231));
#33821=CARTESIAN_POINT('Ctrl Pts',(8.953072650201,6.511404160057,8.840487781273));
#33822=CARTESIAN_POINT('Ctrl Pts',(9.302738926203,6.554727598069,8.424305189807));
#33823=CARTESIAN_POINT('Ctrl Pts',(9.299441398479,6.554292035165,8.427515810797));
#33824=CARTESIAN_POINT('Ctrl Pts',(9.276006083907,6.551308174027,8.449671465829));
#33825=CARTESIAN_POINT('Ctrl Pts',(9.227999435144,6.546634829437,8.486540313026));
#33826=CARTESIAN_POINT('Ctrl Pts',(9.152451654413,6.542524729215,8.525586031012));
#33827=CARTESIAN_POINT('Ctrl Pts',(9.067763106405,6.541050501118,8.55123456792));
#33828=CARTESIAN_POINT('Ctrl Pts',(9.002937571468,6.542211057571,8.557738235401));
#33829=CARTESIAN_POINT('Ctrl Pts',(8.967315586768,6.543566973447,8.557205961694));
#33830=CARTESIAN_POINT('Ctrl Pts',(8.962714823604,6.5437541788,8.557068185445));
#33831=CARTESIAN_POINT('Ctrl Pts',(9.63127320806298,6.05752662158217,8.74023723823402));
#33832=CARTESIAN_POINT('Ctrl Pts',(9.59861968550863,6.05554784605247,8.76989447988101));
#33833=CARTESIAN_POINT('Ctrl Pts',(9.56377963052759,6.05376690177339,8.79757308911125));
#33834=CARTESIAN_POINT('Ctrl Pts',(9.52714118362392,6.05221803617318,8.8228771921826));
#33835=CARTESIAN_POINT('Ctrl Pts',(9.51544884961683,6.05172375064909,8.8309524259838));
#33836=CARTESIAN_POINT('Ctrl Pts',(9.50357367483786,6.05125305271542,8.83878608429263));
#33837=CARTESIAN_POINT('Ctrl Pts',(9.49152905935388,6.05080691142483,8.84636606478418));
#33838=CARTESIAN_POINT('Ctrl Pts',(9.46663316979638,6.04988474962462,8.86203367637514));
#33839=CARTESIAN_POINT('Ctrl Pts',(9.44101708626723,6.04907020633919,8.87662025026625));
#33840=CARTESIAN_POINT('Ctrl Pts',(9.41465075551265,6.04836152478895,8.89011896197565));
#33841=CARTESIAN_POINT('Ctrl Pts',(9.38828952944122,6.0476529804438,8.90361506025176));
#33842=CARTESIAN_POINT('Ctrl Pts',(9.36117771796724,6.04705018167203,8.91602418308567));
#33843=CARTESIAN_POINT('Ctrl Pts',(9.3332677890998,6.04656067319867,8.9272913800025));
#33844=CARTESIAN_POINT('Ctrl Pts',(9.30535515794258,6.04607111733021,8.9385596678297));
#33845=CARTESIAN_POINT('Ctrl Pts',(9.27665152939504,6.04569542348672,8.94868311708087));
#33846=CARTESIAN_POINT('Ctrl Pts',(9.24710436032083,6.04544064223698,8.95757570678599));
#33847=CARTESIAN_POINT('Ctrl Pts',(9.21968152314074,6.04520417881436,8.96582895226545));
#33848=CARTESIAN_POINT('Ctrl Pts',(9.19153146044287,6.04507191208051,8.97302179223174));
#33849=CARTESIAN_POINT('Ctrl Pts',(9.16261456287849,6.0450584487924,8.97903646990965));
#33850=CARTESIAN_POINT('Ctrl Pts',(9.16037449240832,6.04505740584807,8.97950240170001));
#33851=CARTESIAN_POINT('Ctrl Pts',(9.15812982412392,6.04505708043623,8.9799612379583));
#33852=CARTESIAN_POINT('Ctrl Pts',(9.15588054189446,6.045057481699,8.98041291090022));
#33853=CARTESIAN_POINT('Ctrl Pts',(9.12236154441565,6.04506346135141,8.98714377997617));
#33854=CARTESIAN_POINT('Ctrl Pts',(9.08782147666207,6.04522615909127,8.99228271987963));
#33855=CARTESIAN_POINT('Ctrl Pts',(9.05247524549954,6.04556133675228,8.99560506194131));
#33856=CARTESIAN_POINT('Ctrl Pts',(9.02184037719226,6.04585183797877,8.99848456304182));
#33857=CARTESIAN_POINT('Ctrl Pts',(8.99060061916653,6.04627189451713,8.9999993959498));
#33858=CARTESIAN_POINT('Ctrl Pts',(8.958927440406,6.046831514125,8.99999999999996));
#33859=CARTESIAN_POINT('Origin',(8.958927440522,17.50736,8.));
#33860=CARTESIAN_POINT('Ctrl Pts',(8.95892745008802,1.55316848604618,8.99999999999974));
#33861=CARTESIAN_POINT('Ctrl Pts',(9.00275855065562,1.553943645885,8.99999899837848));
#33862=CARTESIAN_POINT('Ctrl Pts',(9.04683010695701,1.55447030043154,8.99709917174271));
#33863=CARTESIAN_POINT('Ctrl Pts',(9.0905895416497,1.55473749600761,8.99129104676408));
#33864=CARTESIAN_POINT('Ctrl Pts',(9.10512924205577,1.55482627557374,8.98936121385597));
#33865=CARTESIAN_POINT('Ctrl Pts',(9.11963440887108,1.5548864802363,8.9871107249482));
#33866=CARTESIAN_POINT('Ctrl Pts',(9.13408467274677,1.55491791715508,8.98454047352005));
#33867=CARTESIAN_POINT('Ctrl Pts',(9.16305493722674,1.55498094270669,8.97938756667391));
#33868=CARTESIAN_POINT('Ctrl Pts',(9.1918032220189,1.55492530956165,8.97295449863129));
#33869=CARTESIAN_POINT('Ctrl Pts',(9.22036197221234,1.55475387971182,8.96521883852068));
#33870=CARTESIAN_POINT('Ctrl Pts',(9.24892072240577,1.55458244986199,8.95748317841007));
#33871=CARTESIAN_POINT('Ctrl Pts',(9.27729079577433,1.55429521929521,8.94844478328275));
#33872=CARTESIAN_POINT('Ctrl Pts',(9.3054821343589,1.55388503037883,8.93802976721407));
#33873=CARTESIAN_POINT('Ctrl Pts',(9.33223490527492,1.55349577287412,8.92814621599014));
#33874=CARTESIAN_POINT('Ctrl Pts',(9.35881934236324,1.55299579736816,8.91702531744028));
#33875=CARTESIAN_POINT('Ctrl Pts',(9.38522933679278,1.55237888045198,8.90457933423687));
#33876=CARTESIAN_POINT('Ctrl Pts',(9.41074299990903,1.5517829011377,8.89255575644138));
#33877=CARTESIAN_POINT('Ctrl Pts',(9.43609438980752,1.55107773409733,8.87929518309596));
#33878=CARTESIAN_POINT('Ctrl Pts',(9.46124299424961,1.55025083931054,8.86468504225787));
#33879=CARTESIAN_POINT('Ctrl Pts',(9.46492613223733,1.55012973646334,8.86254531459026));
#33880=CARTESIAN_POINT('Ctrl Pts',(9.46860484909312,1.55000601088045,8.86037658442236));
#33881=CARTESIAN_POINT('Ctrl Pts',(9.47227894057115,1.54987961105733,8.85817844146731));
#33882=CARTESIAN_POINT('Ctrl Pts',(9.50104973858653,1.54888980887034,8.84096538965656));
#33883=CARTESIAN_POINT('Ctrl Pts',(9.52953374654615,1.54774065894391,8.82194974148639));
#33884=CARTESIAN_POINT('Ctrl Pts',(9.55743303390829,1.54642756706802,8.80110722892218));
#33885=CARTESIAN_POINT('Ctrl Pts',(9.5826050168278,1.5452428369406,8.78230218335038));
#33886=CARTESIAN_POINT('Ctrl Pts',(9.60730057475277,1.54392470007601,8.76201029506294));
#33887=CARTESIAN_POINT('Ctrl Pts',(9.63127322651056,1.5424733773,8.74023722147852));
#33888=CARTESIAN_POINT('Ctrl Pts',(8.9279389474,1.593171467102,8.997867580782));
#33889=CARTESIAN_POINT('Ctrl Pts',(8.937774434699,1.593573040994,8.99815844767));
#33890=CARTESIAN_POINT('Ctrl Pts',(9.006501123144,1.596194951904,8.999171711777));
#33891=CARTESIAN_POINT('Ctrl Pts',(9.135111717268,1.598711309997,8.987844921877));
#33892=CARTESIAN_POINT('Ctrl Pts',(9.310266674501,1.596356340012,8.940309843117));
#33893=CARTESIAN_POINT('Ctrl Pts',(9.480507438288,1.587786189889,8.858829792006));
#33894=CARTESIAN_POINT('Ctrl Pts',(9.591735407857,1.577057308712,8.776278000932));
#33895=CARTESIAN_POINT('Ctrl Pts',(9.646942416699,1.569906309379,8.724650180619));
#33896=CARTESIAN_POINT('Ctrl Pts',(9.653937650666,1.568966676907,8.717912247757));
#33897=CARTESIAN_POINT('Ctrl Pts',(8.93879197217,1.308923750487,9.021370782115));
#33898=CARTESIAN_POINT('Ctrl Pts',(8.948369635441,1.309314926618,9.021655024549));
#33899=CARTESIAN_POINT('Ctrl Pts',(9.015294451232,1.311868617701,9.022645787154));
#33900=CARTESIAN_POINT('Ctrl Pts',(9.140529817566,1.314314972079,9.011585510257));
#33901=CARTESIAN_POINT('Ctrl Pts',(9.311087401957,1.312004268657,8.965163068201));
#33902=CARTESIAN_POINT('Ctrl Pts',(9.47686644203,1.303627875584,8.885584897535));
#33903=CARTESIAN_POINT('Ctrl Pts',(9.585188255283,1.293147013991,8.804951761537));
#33904=CARTESIAN_POINT('Ctrl Pts',(9.638956159986,1.286161646375,8.754519895411));
#33905=CARTESIAN_POINT('Ctrl Pts',(9.645769108012,1.285243780476,8.747937983081));
#33906=CARTESIAN_POINT('Ctrl Pts',(8.953058771447,1.088595421228,8.840488165336));
#33907=CARTESIAN_POINT('Ctrl Pts',(8.960489669369,1.088898666868,8.840709537911));
#33908=CARTESIAN_POINT('Ctrl Pts',(9.012411237366,1.090878811164,8.841481514187));
#33909=CARTESIAN_POINT('Ctrl Pts',(9.10954285353,1.092783101822,8.832872893528));
#33910=CARTESIAN_POINT('Ctrl Pts',(9.241820527383,1.091020419799,8.796738876884));
#33911=CARTESIAN_POINT('Ctrl Pts',(9.370449136028,1.084567200145,8.734771759971));
#33912=CARTESIAN_POINT('Ctrl Pts',(9.454572911059,1.076465913557,8.671926426951));
#33913=CARTESIAN_POINT('Ctrl Pts',(9.496358150974,1.071056145855,8.632590758479));
#33914=CARTESIAN_POINT('Ctrl Pts',(9.501653299641,1.070345156809,8.62745655615));
#33915=CARTESIAN_POINT('Ctrl Pts',(8.962706216611,1.05624554634,8.557068315928));
#33916=CARTESIAN_POINT('Ctrl Pts',(8.967310175283,1.0564328393,8.557205973027));
#33917=CARTESIAN_POINT('Ctrl Pts',(8.999474917003,1.057657053701,8.557686068968));
#33918=CARTESIAN_POINT('Ctrl Pts',(9.059598485478,1.058852437488,8.552333807117));
#33919=CARTESIAN_POINT('Ctrl Pts',(9.141467770911,1.057832960287,8.529870957179));
#33920=CARTESIAN_POINT('Ctrl Pts',(9.2211753306,1.053949459686,8.491307907635));
#33921=CARTESIAN_POINT('Ctrl Pts',(9.273434242506,1.049019449244,8.452103844583));
#33922=CARTESIAN_POINT('Ctrl Pts',(9.299440270493,1.045708085229,8.427516741922));
#33923=CARTESIAN_POINT('Ctrl Pts',(9.302736725367,1.0452725983,8.424306784914));
#33924=CARTESIAN_POINT('Ctrl Pts',(0.001363716877125,7.004096037298,1.995067420053));
#33925=CARTESIAN_POINT('Ctrl Pts',(-0.0002547629821602,7.033536439795,1.947200740707));
#33926=CARTESIAN_POINT('Ctrl Pts',(-0.004372367677244,7.10872651687,1.819803089527));
#33927=CARTESIAN_POINT('Ctrl Pts',(-0.01069751864402,7.22832969105,1.590379225774));
#33928=CARTESIAN_POINT('Ctrl Pts',(-0.01714467798322,7.357904932227,1.288569665529));
#33929=CARTESIAN_POINT('Ctrl Pts',(-0.02256867464758,7.474904436555,0.9310228511914));
#33930=CARTESIAN_POINT('Ctrl Pts',(-0.02637651263401,7.564389025907,0.5171914444451));
#33931=CARTESIAN_POINT('Ctrl Pts',(-0.02742725699744,7.593855284484,0.2127089892188));
#33932=CARTESIAN_POINT('Ctrl Pts',(-0.02749825835039,7.599065112105,0.05030904096556));
#33933=CARTESIAN_POINT('Ctrl Pts',(-0.02750035356636,7.599263124611,0.04357390005572));
#33934=CARTESIAN_POINT('Ctrl Pts',(-0.02360189154764,7.332522732615,2.008012314209));
#33935=CARTESIAN_POINT('Ctrl Pts',(-0.007100235964038,7.363321141605,1.961090142431));
#33936=CARTESIAN_POINT('Ctrl Pts',(0.03503481007398,7.438156938294,1.831220908937));
#33937=CARTESIAN_POINT('Ctrl Pts',(0.1002819388273,7.542515456862,1.58377920092));
#33938=CARTESIAN_POINT('Ctrl Pts',(0.1674804264521,7.633451595482,1.250318159269));
#33939=CARTESIAN_POINT('Ctrl Pts',(0.2248447651456,7.687511126466,0.8568392396603));
#33940=CARTESIAN_POINT('Ctrl Pts',(0.2662490974893,7.689939339522,0.4123496126132));
#33941=CARTESIAN_POINT('Ctrl Pts',(0.2789069387192,7.649350136403,0.0983060253891));
#33942=CARTESIAN_POINT('Ctrl Pts',(0.2806593262459,7.61693316005,-0.06530116546358));
#33943=CARTESIAN_POINT('Ctrl Pts',(0.2807233254674,7.615570360117,-0.07207992811569));
#33944=CARTESIAN_POINT('Ctrl Pts',(0.2095583867952,7.565232260888,2.019596510591));
#33945=CARTESIAN_POINT('Ctrl Pts',(0.2389857802897,7.583483482567,1.964918501646));
#33946=CARTESIAN_POINT('Ctrl Pts',(0.3101581568233,7.623781352774,1.8140793846));
#33947=CARTESIAN_POINT('Ctrl Pts',(0.4068616564539,7.663606955409,1.532524925837));
#33948=CARTESIAN_POINT('Ctrl Pts',(0.4886889080965,7.670258563261,1.166376398115));
#33949=CARTESIAN_POINT('Ctrl Pts',(0.5374668975788,7.630189595634,0.7523865517109));
#33950=CARTESIAN_POINT('Ctrl Pts',(0.5443422263585,7.535897759144,0.306016547344));
#33951=CARTESIAN_POINT('Ctrl Pts',(0.5164520353948,7.437358052934,0.005351407090497));
#33952=CARTESIAN_POINT('Ctrl Pts',(0.4928891039185,7.378812409657,-0.1483861234052));
#33953=CARTESIAN_POINT('Ctrl Pts',(0.4918968454424,7.376374277029,-0.1547511527335));
#33954=CARTESIAN_POINT('Ctrl Pts',(0.5381945238366,7.539889032304,2.021739002091));
#33955=CARTESIAN_POINT('Ctrl Pts',(0.5663364060878,7.540440651784,1.956015197361));
#33956=CARTESIAN_POINT('Ctrl Pts',(0.6290746726959,7.536110224441,1.780336254062));
#33957=CARTESIAN_POINT('Ctrl Pts',(0.6951750183964,7.507132098316,1.472370815215));
#33958=CARTESIAN_POINT('Ctrl Pts',(0.7224092873361,7.442649702456,1.095301225047));
#33959=CARTESIAN_POINT('Ctrl Pts',(0.6972159851596,7.342926709167,0.690529825709));
#33960=CARTESIAN_POINT('Ctrl Pts',(0.6139081869805,7.209721985333,0.2723690173976));
#33961=CARTESIAN_POINT('Ctrl Pts',(0.5194992042506,7.105762363827,-0.001310753365661));
#33962=CARTESIAN_POINT('Ctrl Pts',(0.461141932074,7.050813259361,-0.1409866863127));
#33963=CARTESIAN_POINT('Ctrl Pts',(0.4587078974377,7.048535413961,-0.1467692430359));
#33964=CARTESIAN_POINT('Ctrl Pts',(0.0865688256819392,7.3235406542984,1.99263811287353));
#33965=CARTESIAN_POINT('Ctrl Pts',(0.0896802537077462,7.32912623877558,
1.96759743689578));
#33966=CARTESIAN_POINT('Ctrl Pts',(0.0923915043624595,7.3347911606353,1.94236105944537));
#33967=CARTESIAN_POINT('Ctrl Pts',(0.0947293636910101,7.34039900203038,
1.91744867197809));
#33968=CARTESIAN_POINT('Ctrl Pts',(0.0949482417161692,7.34092402645549,
1.91511629290624));
#33969=CARTESIAN_POINT('Ctrl Pts',(0.0951638771415863,7.34144856040776,
1.91278677211149));
#33970=CARTESIAN_POINT('Ctrl Pts',(0.0953763099453126,7.3419724980081,1.91046054583049));
#33971=CARTESIAN_POINT('Ctrl Pts',(0.0969299050857642,7.34580423630613,
1.89344804219467));
#33972=CARTESIAN_POINT('Ctrl Pts',(0.0983102863785579,7.34959839588947,
1.87660634057612));
#33973=CARTESIAN_POINT('Ctrl Pts',(0.0995681453181531,7.35344107264442,
1.85954655396089));
#33974=CARTESIAN_POINT('Ctrl Pts',(0.0997992999342739,7.35414723487152,
1.85641150574363));
#33975=CARTESIAN_POINT('Ctrl Pts',(0.100026202607223,7.35485500173232,1.85326901614998));
#33976=CARTESIAN_POINT('Ctrl Pts',(0.100249016916711,7.35556486233215,1.85011657530178));
#33977=CARTESIAN_POINT('Ctrl Pts',(0.100750378724828,7.35716214302145,1.84302316443752));
#33978=CARTESIAN_POINT('Ctrl Pts',(0.101231115787448,7.35877004683759,1.83587940956835));
#33979=CARTESIAN_POINT('Ctrl Pts',(0.101692526905404,7.36039395275203,1.82865566109089));
#33980=CARTESIAN_POINT('Ctrl Pts',(0.103474856351766,7.36666674336496,1.80075191295082));
#33981=CARTESIAN_POINT('Ctrl Pts',(0.104977614729166,7.37319161572645,1.77167311737816));
#33982=CARTESIAN_POINT('Ctrl Pts',(0.10616646031735,7.37984389128196,1.74175841581746));
#33983=CARTESIAN_POINT('Ctrl Pts',(0.107355305905534,7.38649616683747,1.71184371425676));
#33984=CARTESIAN_POINT('Ctrl Pts',(0.108232329401721,7.39327388476653,1.68109269976559));
#33985=CARTESIAN_POINT('Ctrl Pts',(0.108791895149357,7.4001768310032,1.64928217769217));
#33986=CARTESIAN_POINT('Ctrl Pts',(0.109166261829539,7.40479511415763,1.62799996091283));
#33987=CARTESIAN_POINT('Ctrl Pts',(0.109398357722325,7.40947001886123,1.60624309301958));
#33988=CARTESIAN_POINT('Ctrl Pts',(0.109487433858617,7.41418919456437,1.58401272756834));
#33989=CARTESIAN_POINT('Ctrl Pts',(0.109531499792492,7.41652376915564,1.57301537345363));
#33990=CARTESIAN_POINT('Ctrl Pts',(0.109540579661707,7.41886914803633,1.561902154465));
#33991=CARTESIAN_POINT('Ctrl Pts',(0.109514929847241,7.4212239270889,1.55067260771111));
#33992=CARTESIAN_POINT('Ctrl Pts',(0.109437430765813,7.42833872371927,1.51674333467875));
#33993=CARTESIAN_POINT('Ctrl Pts',(0.109042119817046,7.43553816021822,1.48175438125156));
#33994=CARTESIAN_POINT('Ctrl Pts',(0.108313731955709,7.44279124618812,1.44554679740932));
#33995=CARTESIAN_POINT('Ctrl Pts',(0.107585344094372,7.45004433215802,1.40933921356709));
#33996=CARTESIAN_POINT('Ctrl Pts',(0.106523548757051,7.4573515698644,1.37191311297681));
#33997=CARTESIAN_POINT('Ctrl Pts',(0.105117873628984,7.46467568199902,1.33311770345657));
#33998=CARTESIAN_POINT('Ctrl Pts',(0.104377954802098,7.46853094581526,1.31269658813082));
#33999=CARTESIAN_POINT('Ctrl Pts',(0.103543023712786,7.47239091384454,1.29189575125132));
#34000=CARTESIAN_POINT('Ctrl Pts',(0.102611872470959,7.47624431142032,1.27071260516852));
#34001=CARTESIAN_POINT('Ctrl Pts',(0.101774051099112,7.47971148055266,1.2516526590353));
#34002=CARTESIAN_POINT('Ctrl Pts',(0.100858336039839,7.48317330483615,1.23228319638487));
#34003=CARTESIAN_POINT('Ctrl Pts',(0.0998645221405797,7.48662201250552,
1.21260136918125));
#34004=CARTESIAN_POINT('Ctrl Pts',(0.097766187543305,7.49390359975632,1.17104523981968));
#34005=CARTESIAN_POINT('Ctrl Pts',(0.0953185572951622,7.50112665999997,
1.12809788131681));
#34006=CARTESIAN_POINT('Ctrl Pts',(0.0925150010827101,7.50821076792826,
1.08370319344878));
#34007=CARTESIAN_POINT('Ctrl Pts',(0.089711444870258,7.51529487585655,1.03930850558076));
#34008=CARTESIAN_POINT('Ctrl Pts',(0.0865511551028964,7.52224148615219,
0.993466772008885));
#34009=CARTESIAN_POINT('Ctrl Pts',(0.0830270933744481,7.52899459767804,
0.945862005357544));
#34010=CARTESIAN_POINT('Ctrl Pts',(0.0821381954945036,7.530697980587,0.933854333695601));
#34011=CARTESIAN_POINT('Ctrl Pts',(0.081226180044907,7.53238887179564,0.921734422666414));
#34012=CARTESIAN_POINT('Ctrl Pts',(0.0802903601283761,7.53406600471985,
0.909495233375608));
#34013=CARTESIAN_POINT('Ctrl Pts',(0.0775160945255589,7.5390379144867,0.873211797581972));
#34014=CARTESIAN_POINT('Ctrl Pts',(0.0745326823159648,7.54389003125133,
0.835880050581168));
#34015=CARTESIAN_POINT('Ctrl Pts',(0.0713215509276857,7.54858645422804,
0.797314112004502));
#34016=CARTESIAN_POINT('Ctrl Pts',(0.0672743784190882,7.55450562465796,
0.748707254326407));
#34017=CARTESIAN_POINT('Ctrl Pts',(0.0628650243611779,7.56017951647996,
0.698140410147152));
#34018=CARTESIAN_POINT('Ctrl Pts',(0.0580773486278632,7.56549672991315,
0.645280546452683));
#34019=CARTESIAN_POINT('Ctrl Pts',(0.0577849862459548,7.56582142884245,
0.642052626159432));
#34020=CARTESIAN_POINT('Ctrl Pts',(0.057491216650073,7.56614478165179,0.638816155811791));
#34021=CARTESIAN_POINT('Ctrl Pts',(0.0571960377183247,7.5664667564898,0.635571059829908));
#34022=CARTESIAN_POINT('Ctrl Pts',(0.0532958632914503,7.5707209829749,0.592693879245485));
#34023=CARTESIAN_POINT('Ctrl Pts',(0.0491499956495321,7.57473650573253,
0.548310744947044));
#34024=CARTESIAN_POINT('Ctrl Pts',(0.0447657824929133,7.57841830892359,
0.502354796048155));
#34025=CARTESIAN_POINT('Ctrl Pts',(0.0433844758662343,7.57957831163429,
0.487875742571131));
#34026=CARTESIAN_POINT('Ctrl Pts',(0.0419795965094829,7.58070504176636,
0.473240574471837));
#34027=CARTESIAN_POINT('Ctrl Pts',(0.0405516110274916,7.58179564957126,
0.458447294243215));
#34028=CARTESIAN_POINT('Ctrl Pts',(0.0352357117822026,7.58585560765916,
0.403376995424063));
#34029=CARTESIAN_POINT('Ctrl Pts',(0.0295974679152405,7.58941730052929,
0.346115563689829));
#34030=CARTESIAN_POINT('Ctrl Pts',(0.0236363315001921,7.59231304495109,
0.28649801517568));
#34031=CARTESIAN_POINT('Ctrl Pts',(0.0229136519574967,7.59266410137872,
0.279270470006933));
#34032=CARTESIAN_POINT('Ctrl Pts',(0.0221862695618803,7.59300533008682,
0.272008321185318));
#34033=CARTESIAN_POINT('Ctrl Pts',(0.0214542211065908,7.59333639705194,
0.264711295552353));
#34034=CARTESIAN_POINT('Ctrl Pts',(0.0156433037850095,7.59596436894136,
0.206788336573017));
#34035=CARTESIAN_POINT('Ctrl Pts',(0.00953650453228541,7.59795273247266,
0.146666268293311));
#34036=CARTESIAN_POINT('Ctrl Pts',(0.00317281194423555,7.59911587089843,
0.0844485241839117));
#34037=CARTESIAN_POINT('Ctrl Pts',(0.00212199046213768,7.59930793719131,
0.0741746554868914));
#34038=CARTESIAN_POINT('Ctrl Pts',(0.00106426940600786,7.5994774832001,
0.0638436870231593));
#34039=CARTESIAN_POINT('Ctrl Pts',(-4.55832343463506E-8,7.59962364606423,
0.0534561336397867));
#34040=CARTESIAN_POINT('Origin',(-1.165507426858E-9,7.09967345946,0.04642263385286));
#34041=CARTESIAN_POINT('Ctrl Pts',(0.09332729536784,7.333647414405,2.027339375446));
#34042=CARTESIAN_POINT('Ctrl Pts',(0.0956460765109,7.337274567028,2.020940474449));
#34043=CARTESIAN_POINT('Ctrl Pts',(0.1067234777855,7.354783699243,1.98987166704));
#34044=CARTESIAN_POINT('Ctrl Pts',(0.1252614819808,7.385575923908,1.933661042191));
#34045=CARTESIAN_POINT('Ctrl Pts',(0.1483230597314,7.42617634589,1.855915420958));
#34046=CARTESIAN_POINT('Ctrl Pts',(0.1706856731413,7.467450488292,1.772637372698));
#34047=CARTESIAN_POINT('Ctrl Pts',(0.1930020158897,7.510044352663,1.681442257421));
#34048=CARTESIAN_POINT('Ctrl Pts',(0.2153249421398,7.553626038292,1.581617848906));
#34049=CARTESIAN_POINT('Ctrl Pts',(0.237760929357,7.597792410414,1.472368077024));
#34050=CARTESIAN_POINT('Ctrl Pts',(0.2604508155607,7.642090028244,1.352628361367));
#34051=CARTESIAN_POINT('Ctrl Pts',(0.2834723960102,7.685792567441,1.221593810851));
#34052=CARTESIAN_POINT('Ctrl Pts',(0.3069634986954,7.728092190564,1.078167578903));
#34053=CARTESIAN_POINT('Ctrl Pts',(0.3311487111769,7.768064414624,0.9208497005947));
#34054=CARTESIAN_POINT('Ctrl Pts',(0.3564829869057,7.804698725932,0.7467239997499));
#34055=CARTESIAN_POINT('Ctrl Pts',(0.383183258108,7.836191149907,0.5536747851937));
#34056=CARTESIAN_POINT('Ctrl Pts',(0.4118738384147,7.860119523589,0.3402017808901));
#34057=CARTESIAN_POINT('Ctrl Pts',(0.4323948723823,7.868947086026,0.183227181261));
#34058=CARTESIAN_POINT('Ctrl Pts',(0.4433244432103,7.871063970647,0.0981968847509));
#34059=CARTESIAN_POINT('Ctrl Pts',(0.4441525558925,7.871209365081,0.09174594482544));
#34060=CARTESIAN_POINT('Ctrl Pts',(0.00413371639593,7.185905309626,1.91818759396));
#34061=CARTESIAN_POINT('Ctrl Pts',(0.006375610685106,7.18924784677,1.912236954105));
#34062=CARTESIAN_POINT('Ctrl Pts',(0.01709859516906,7.205399755638,1.883314369697));
#34063=CARTESIAN_POINT('Ctrl Pts',(0.03514371433924,7.23393502954,1.830747145249));
#34064=CARTESIAN_POINT('Ctrl Pts',(0.05770123147572,7.271715716269,1.757747888332));
#34065=CARTESIAN_POINT('Ctrl Pts',(0.07967986153062,7.310277891777,1.67924388339));
#34066=CARTESIAN_POINT('Ctrl Pts',(0.1016848560021,7.350182806674,1.593045679998));
#34067=CARTESIAN_POINT('Ctrl Pts',(0.123750946579,7.391096468068,1.498504779354));
#34068=CARTESIAN_POINT('Ctrl Pts',(0.1459810956979,7.432635330052,1.394842391727));
#34069=CARTESIAN_POINT('Ctrl Pts',(0.1685009069597,7.474346978144,1.281076556188));
#34070=CARTESIAN_POINT('Ctrl Pts',(0.1913848392552,7.515534476051,1.156432362992));
#34071=CARTESIAN_POINT('Ctrl Pts',(0.2147620673246,7.555413295895,1.019885111452));
#34072=CARTESIAN_POINT('Ctrl Pts',(0.2388605698404,7.593100119069,0.8699663883089));
#34073=CARTESIAN_POINT('Ctrl Pts',(0.2641204729043,7.62760311364,0.7039575843834));
#34074=CARTESIAN_POINT('Ctrl Pts',(0.2907706259586,7.657204843238,0.5197608497961));
#34075=CARTESIAN_POINT('Ctrl Pts',(0.3194378379588,7.679569502558,0.3159115398518));
#34076=CARTESIAN_POINT('Ctrl Pts',(0.3399248718625,7.687650272031,0.1661433025018));
#34077=CARTESIAN_POINT('Ctrl Pts',(0.3508467599435,7.689487914492,0.08495485013407));
#34078=CARTESIAN_POINT('Ctrl Pts',(0.3516743579076,7.689612809971,0.07879497185148));
#34079=CARTESIAN_POINT('Ctrl Pts',(-0.1656119288838,7.120545824473,1.825386409491));
#34080=CARTESIAN_POINT('Ctrl Pts',(-0.1635163591258,7.123519766875,1.81996392764));
#34081=CARTESIAN_POINT('Ctrl Pts',(-0.1534678705812,7.137930212453,1.79353716736));
#34082=CARTESIAN_POINT('Ctrl Pts',(-0.1363607683355,7.163697474219,1.744942128327));
#34083=CARTESIAN_POINT('Ctrl Pts',(-0.1147625365556,7.198182465273,1.676772747774));
#34084=CARTESIAN_POINT('Ctrl Pts',(-0.09351467101442,7.233744731282,1.602739197824));
#34085=CARTESIAN_POINT('Ctrl Pts',(-0.07210220814429,7.270802639682,1.520912659697));
#34086=CARTESIAN_POINT('Ctrl Pts',(-0.05052490541031,7.308992126025,1.430734790665));
#34087=CARTESIAN_POINT('Ctrl Pts',(-0.0286864898805,7.347943299813,1.331405236481));
#34088=CARTESIAN_POINT('Ctrl Pts',(-0.006490350805654,7.387171471204,1.222048142703));
#34089=CARTESIAN_POINT('Ctrl Pts',(0.01613162121186,7.425990916832,1.101895162335));
#34090=CARTESIAN_POINT('Ctrl Pts',(0.03929213278287,7.463608317969,0.9700014892299));
#34091=CARTESIAN_POINT('Ctrl Pts',(0.06322561625506,7.499163150947,0.8248557918099));
#34092=CARTESIAN_POINT('Ctrl Pts',(0.0883439795788,7.531628832607,0.6639649220211));
#34093=CARTESIAN_POINT('Ctrl Pts',(0.1148987520299,7.559346495031,0.4851100355565));
#34094=CARTESIAN_POINT('Ctrl Pts',(0.1435214914534,7.579991317253,0.2867927966161));
#34095=CARTESIAN_POINT('Ctrl Pts',(0.163943819323,7.587052319387,0.1413866086485));
#34096=CARTESIAN_POINT('Ctrl Pts',(0.1748512775237,7.588418185354,0.0624210760095));
#34097=CARTESIAN_POINT('Ctrl Pts',(0.1756779116267,7.58850768362,0.05642892400282));
#34098=CARTESIAN_POINT('Ctrl Pts',(-0.3607780994109,7.158797009499,1.779076638338));
#34099=CARTESIAN_POINT('Ctrl Pts',(-0.3588507672437,7.161438093464,1.774090671374));
#34100=CARTESIAN_POINT('Ctrl Pts',(-0.3495777848353,7.174288444165,1.749698719792));
#34101=CARTESIAN_POINT('Ctrl Pts',(-0.3335491737094,7.197675652681,1.70411452853));
#34102=CARTESIAN_POINT('Ctrl Pts',(-0.3130538865687,7.229459393784,1.639289845029));
#34103=CARTESIAN_POINT('Ctrl Pts',(-0.2926462223267,7.262708145696,1.56797120654));
#34104=CARTESIAN_POINT('Ctrl Pts',(-0.2719150265568,7.297685667349,1.488471217684));
#34105=CARTESIAN_POINT('Ctrl Pts',(-0.2508997108556,7.333979610279,1.400318838748));
#34106=CARTESIAN_POINT('Ctrl Pts',(-0.2295116935927,7.371223370819,1.302660309974));
#34107=CARTESIAN_POINT('Ctrl Pts',(-0.2076876987406,7.408877164792,1.194714908186));
#34108=CARTESIAN_POINT('Ctrl Pts',(-0.1853669172732,7.4462446648,1.07569529903));
#34109=CARTESIAN_POINT('Ctrl Pts',(-0.1624555769196,7.482494516028,0.9447183706797));
#34110=CARTESIAN_POINT('Ctrl Pts',(-0.1387118251766,7.516763216746,0.8001693426502));
#34111=CARTESIAN_POINT('Ctrl Pts',(-0.1137561980987,7.547947286417,0.6397351948215));
#34112=CARTESIAN_POINT('Ctrl Pts',(-0.0873110901226,7.574399433416,0.4609765504098));
#34113=CARTESIAN_POINT('Ctrl Pts',(-0.05873948333615,7.593726880203,0.2623030025697));
#34114=CARTESIAN_POINT('Ctrl Pts',(-0.03839155165445,7.599826349973,0.1169978048482));
#34115=CARTESIAN_POINT('Ctrl Pts',(-0.02750058379875,7.600681132993,0.03791428735155));
#34116=CARTESIAN_POINT('Ctrl Pts',(-0.02667504964837,7.600731832416,0.03191205058198));
#34117=CARTESIAN_POINT('Ctrl Pts',(0.006092677290347,7.599378811355,0.0686831784786));
#34118=CARTESIAN_POINT('Ctrl Pts',(0.003734755645105,7.599467813605,0.06378738843317));
#34119=CARTESIAN_POINT('Ctrl Pts',(-0.0004662461470239,7.599626415391,0.05398924362921));
#34120=CARTESIAN_POINT('Ctrl Pts',(-0.005281917817338,7.599808258387,0.03903695947461));
#34121=CARTESIAN_POINT('Ctrl Pts',(-0.008492810869693,7.599929521181,0.02433820698079));
#34122=CARTESIAN_POINT('Ctrl Pts',(-0.01020745239528,7.599994282083,0.009761485286655));
#34123=CARTESIAN_POINT('Ctrl Pts',(-0.01046402051099,7.600003972854,-0.005086971198367));
#34124=CARTESIAN_POINT('Ctrl Pts',(-0.009120895515257,7.599953242924,-0.02060522202386));
#34125=CARTESIAN_POINT('Ctrl Pts',(-0.005888618218437,7.599831169114,-0.03701638653157));
#34126=CARTESIAN_POINT('Ctrl Pts',(-0.0007646346168158,7.599637680482,-0.05329605734118));
#34127=CARTESIAN_POINT('Ctrl Pts',(0.003740802961434,7.599467585381,-0.06380088841689));
#34128=CARTESIAN_POINT('Ctrl Pts',(0.006102566100798,7.599378439467,-0.06870005169305));
#34129=CARTESIAN_POINT('Ctrl Pts',(0.01191131196756,7.59942502026,0.0658677090234));
#34130=CARTESIAN_POINT('Ctrl Pts',(0.009633710571033,7.599510770099,0.06113683658055));
#34131=CARTESIAN_POINT('Ctrl Pts',(0.005585856903677,7.599663190864,0.05169022499271));
#34132=CARTESIAN_POINT('Ctrl Pts',(0.000963349003167,7.599837277401,0.03732842304098));
#34133=CARTESIAN_POINT('Ctrl Pts',(-0.002109362182591,7.599953011217,0.02325255344247));
#34134=CARTESIAN_POINT('Ctrl Pts',(-0.003746892804695,7.600014693386,0.009321455251517));
#34135=CARTESIAN_POINT('Ctrl Pts',(-0.003991703715731,7.600023915162,-0.004857311815456));
#34136=CARTESIAN_POINT('Ctrl Pts',(-0.002709569211279,7.599975619204,-0.01968209560348));
#34137=CARTESIAN_POINT('Ctrl Pts',(0.0003816499432407,7.599859185572,-0.03538922245973));
#34138=CARTESIAN_POINT('Ctrl Pts',(0.005298322938301,7.599674017825,-0.05102182560792));
#34139=CARTESIAN_POINT('Ctrl Pts',(0.009639551531228,7.599510550216,-0.0611499027721));
#34140=CARTESIAN_POINT('Ctrl Pts',(0.01192093360296,7.599424658936,-0.06588431051089));
#34141=CARTESIAN_POINT('Ctrl Pts',(0.01772876858228,7.599345883008,0.06305053973491));
#34142=CARTESIAN_POINT('Ctrl Pts',(0.01553153160734,7.599428378633,0.0584846866516));
#34143=CARTESIAN_POINT('Ctrl Pts',(0.01163691029,7.599574614956,0.04938982358297));
#34144=CARTESIAN_POINT('Ctrl Pts',(0.007207672391512,7.599740940741,0.03561886170935));
#34145=CARTESIAN_POINT('Ctrl Pts',(0.004273219066756,7.59985114252,0.02216624982538));
#34146=CARTESIAN_POINT('Ctrl Pts',(0.002712841755993,7.599909744253,0.00888116198926));
#34147=CARTESIAN_POINT('Ctrl Pts',(0.002479794515622,7.599918496774,-0.004627515069058));
#34148=CARTESIAN_POINT('Ctrl Pts',(0.0037009049865,7.599872636135,-0.01875841664829));
#34149=CARTESIAN_POINT('Ctrl Pts',(0.006650988422478,7.5997618458,-0.03376108270729));
#34150=CARTESIAN_POINT('Ctrl Pts',(0.01136023679858,7.599585003543,-0.0487462262884));
#34151=CARTESIAN_POINT('Ctrl Pts',(0.01553716609792,7.599428167097,-0.05849731878176));
#34152=CARTESIAN_POINT('Ctrl Pts',(0.0177381228957,7.599345532253,-0.06306686930571));
#34153=CARTESIAN_POINT('Ctrl Pts',(0.02354285942058,7.59914142936,0.0602327300384));
#34154=CARTESIAN_POINT('Ctrl Pts',(0.02142600081824,7.599220670193,0.05583193601436));
#34155=CARTESIAN_POINT('Ctrl Pts',(0.01768463845156,7.599360720975,0.04708890448941));
#34156=CARTESIAN_POINT('Ctrl Pts',(0.01344870410615,7.599519284634,0.03390891837772));
#34157=CARTESIAN_POINT('Ctrl Pts',(0.01065253264352,7.599623953398,0.02107970464507));
#34158=CARTESIAN_POINT('Ctrl Pts',(0.009169322037672,7.599679474151,0.00844077107666));
#34159=CARTESIAN_POINT('Ctrl Pts',(0.008948040510102,7.599687757336,-0.004397667376584));
#34160=CARTESIAN_POINT('Ctrl Pts',(0.01010811635383,7.599644332445,-0.01783453251719));
#34161=CARTESIAN_POINT('Ctrl Pts',(0.01291703957055,7.599539186405,-0.03213257955283));
#34162=CARTESIAN_POINT('Ctrl Pts',(0.01741882731943,7.599370671111,-0.04647011514499));
#34163=CARTESIAN_POINT('Ctrl Pts',(0.02143142880335,7.599220467005,-0.05584413397716));
#34164=CARTESIAN_POINT('Ctrl Pts',(0.02355194636561,7.599141089176,-0.06024878760501));
#34165=CARTESIAN_POINT('Origin',(-3.054477616688E-10,7.099673459428,-0.04642263614025));
#34166=CARTESIAN_POINT('Ctrl Pts',(-0.02750316139292,7.599262953893,-0.04358922770243));
#34167=CARTESIAN_POINT('Ctrl Pts',(-0.02750089427335,7.599065008369,-0.05032035313669));
#34168=CARTESIAN_POINT('Ctrl Pts',(-0.02742485534672,7.593772444205,-0.2152695514171));
#34169=CARTESIAN_POINT('Ctrl Pts',(-0.02635280173775,7.563632607212,-0.5234275620995));
#34170=CARTESIAN_POINT('Ctrl Pts',(-0.02245453925618,7.472273113365,-0.9410069594233));
#34171=CARTESIAN_POINT('Ctrl Pts',(-0.01694441566883,7.353683066177,-1.299793310531));
#34172=CARTESIAN_POINT('Ctrl Pts',(-0.0104233500914,7.222960376541,-1.601669677065));
#34173=CARTESIAN_POINT('Ctrl Pts',(-0.00415034249476,7.104640819788,-1.82694866898));
#34174=CARTESIAN_POINT('Ctrl Pts',(-0.000137982512947,7.031410069502,-1.950653360374));
#34175=CARTESIAN_POINT('Ctrl Pts',(0.00136439425857,7.004084473842,-1.995080420042));
#34176=CARTESIAN_POINT('Ctrl Pts',(0.2807219033003,7.615574941146,0.07206410546599));
#34177=CARTESIAN_POINT('Ctrl Pts',(0.2806561737659,7.616937054043,0.06529447791626));
#34178=CARTESIAN_POINT('Ctrl Pts',(0.2788362287103,7.649866050139,-0.1007651614224));
#34179=CARTESIAN_POINT('Ctrl Pts',(0.265938333337,7.690613712512,-0.4189036102997));
#34180=CARTESIAN_POINT('Ctrl Pts',(0.2235950281924,7.686867087972,-0.8676904200621));
#34181=CARTESIAN_POINT('Ctrl Pts',(0.1653583372218,7.630983300808,-1.262746140425));
#34182=CARTESIAN_POINT('Ctrl Pts',(0.09742648092697,7.538286908882,-1.596177405319));
#34183=CARTESIAN_POINT('Ctrl Pts',(0.03275103019119,7.434243995127,-1.838700874606));
#34184=CARTESIAN_POINT('Ctrl Pts',(-0.008292099066438,7.361100787874,-1.964475131896));
#34185=CARTESIAN_POINT('Ctrl Pts',(-0.02360837126205,7.33251617638,-2.008025395665));
#34186=CARTESIAN_POINT('Ctrl Pts',(0.4918992607783,7.376380576182,0.1547359142356));
#34187=CARTESIAN_POINT('Ctrl Pts',(0.4928878083094,7.378817517877,0.1483835574526));
#34188=CARTESIAN_POINT('Ctrl Pts',(0.5167500083095,7.438288421961,-0.007565532271832));
#34189=CARTESIAN_POINT('Ctrl Pts',(0.5448287089649,7.537827128944,-0.3123858450142));
#34190=CARTESIAN_POINT('Ctrl Pts',(0.536824011986,7.632025775638,-0.7634855185152));
#34191=CARTESIAN_POINT('Ctrl Pts',(0.4864905623783,7.670854401701,-1.179726783912));
#34192=CARTESIAN_POINT('Ctrl Pts',(0.403012509611,7.662572001204,-1.546392400176));
#34193=CARTESIAN_POINT('Ctrl Pts',(0.3064646604075,7.621844952183,-1.822739961704));
#34194=CARTESIAN_POINT('Ctrl Pts',(0.2368627668342,7.582171578457,-1.968863315844));
#34195=CARTESIAN_POINT('Ctrl Pts',(0.2095495364899,7.56523383601,-2.019612509741));
#34196=CARTESIAN_POINT('Ctrl Pts',(0.4587131901116,7.048540031596,0.1467549726054));
#34197=CARTESIAN_POINT('Ctrl Pts',(0.4611428327528,7.050816780058,0.140984574553));
#34198=CARTESIAN_POINT('Ctrl Pts',(0.5203496374819,7.106634506402,-0.0006860175177874));
#34199=CARTESIAN_POINT('Ctrl Pts',(0.615766516957,7.21185561697,-0.2781802504272));
#34200=CARTESIAN_POINT('Ctrl Pts',(0.6987262516412,7.34600605939,-0.7010848027864));
#34201=CARTESIAN_POINT('Ctrl Pts',(0.7224328581585,7.445482591648,-1.108648913658));
#34202=CARTESIAN_POINT('Ctrl Pts',(0.6931602429223,7.509115316905,-1.487044303164));
#34203=CARTESIAN_POINT('Ctrl Pts',(0.6260499982531,7.536574687926,-1.790200141908));
#34204=CARTESIAN_POINT('Ctrl Pts',(0.5643084424037,7.540405136517,-1.96075674842));
#34205=CARTESIAN_POINT('Ctrl Pts',(0.5381889316308,7.539895380596,-2.021758679482));
#34206=CARTESIAN_POINT('Ctrl Pts',(-9.09791454320777E-7,7.59962392227978,
-0.0534607251838897));
#34207=CARTESIAN_POINT('Ctrl Pts',(0.0065283531795287,7.59872753669475,
-0.117157269822079));
#34208=CARTESIAN_POINT('Ctrl Pts',(0.0127944512896137,7.59695439925381,
-0.178629296927244));
#34209=CARTESIAN_POINT('Ctrl Pts',(0.0187482387130406,7.59450601408332,
-0.237760296202854));
#34210=CARTESIAN_POINT('Ctrl Pts',(0.0205286496400157,7.59377385295613,
-0.255442734245402));
#34211=CARTESIAN_POINT('Ctrl Pts',(0.0222814724519866,7.59298124399135,
-0.272915929949871));
#34212=CARTESIAN_POINT('Ctrl Pts',(0.0240062157852462,7.59213345316372,
-0.290177057808215));
#34213=CARTESIAN_POINT('Ctrl Pts',(0.0299524098926225,7.58921062474841,
-0.34968621188274));
#34214=CARTESIAN_POINT('Ctrl Pts',(0.0355590332814241,7.58563490866102,
-0.406673539550654));
#34215=CARTESIAN_POINT('Ctrl Pts',(0.0408307692423231,7.58158039917757,
-0.461351966728956));
#34216=CARTESIAN_POINT('Ctrl Pts',(0.0422015720466334,7.58052611022773,
-0.475569928680623));
#34217=CARTESIAN_POINT('Ctrl Pts',(0.0435499057751943,7.57943924715598,
-0.489631862685936));
#34218=CARTESIAN_POINT('Ctrl Pts',(0.0448761834513,7.57832247795482,-0.503541692217891));
#34219=CARTESIAN_POINT('Ctrl Pts',(0.0450702352681292,7.57815907997537,
-0.50557688269202));
#34220=CARTESIAN_POINT('Ctrl Pts',(0.0452638122698697,7.57799504118337,
-0.507608814416376));
#34221=CARTESIAN_POINT('Ctrl Pts',(0.0454569139117579,7.57783036882969,
-0.509637503453062));
#34222=CARTESIAN_POINT('Ctrl Pts',(0.0504911583145555,7.57353728842532,
-0.562526315418047));
#34223=CARTESIAN_POINT('Ctrl Pts',(0.0552009765518408,7.56881802512354,
-0.613211073658562));
#34224=CARTESIAN_POINT('Ctrl Pts',(0.0595853187064746,7.56379768086552,
-0.661979072988505));
#34225=CARTESIAN_POINT('Ctrl Pts',(0.0606025057451536,7.56263293848711,
-0.67329346750224));
#34226=CARTESIAN_POINT('Ctrl Pts',(0.0616022346632844,7.56145177499226,
-0.684504695951582));
#34227=CARTESIAN_POINT('Ctrl Pts',(0.0625845886514869,7.56025538274919,
-0.695616355735607));
#34228=CARTESIAN_POINT('Ctrl Pts',(0.0673140541170907,7.5544954470591,-0.749112561630028));
#34229=CARTESIAN_POINT('Ctrl Pts',(0.0716395926981727,7.54838661205288,
-0.800300379710368));
#34230=CARTESIAN_POINT('Ctrl Pts',(0.075594696585323,7.54203220392621,-0.849588597925932));
#34231=CARTESIAN_POINT('Ctrl Pts',(0.0761378573316066,7.54115954288904,
-0.856357427810763));
#34232=CARTESIAN_POINT('Ctrl Pts',(0.0766740369073583,7.54028217083988,
-0.863090434326044));
#34233=CARTESIAN_POINT('Ctrl Pts',(0.0772033241581099,7.53940028223977,
-0.869788678684179));
#34234=CARTESIAN_POINT('Ctrl Pts',(0.0785440273151084,7.53716642750662,
-0.886755566408276));
#34235=CARTESIAN_POINT('Ctrl Pts',(0.0798407302385532,7.53490375412732,
-0.903499201470491));
#34236=CARTESIAN_POINT('Ctrl Pts',(0.0810937204904941,7.53261600119494,
-0.920028260064166));
#34237=CARTESIAN_POINT('Ctrl Pts',(0.0839373260662721,7.5274240477983,-0.957540222433014));
#34238=CARTESIAN_POINT('Ctrl Pts',(0.0865557106729754,7.52210382157748,
-0.993947062290873));
#34239=CARTESIAN_POINT('Ctrl Pts',(0.0889539161282571,7.51669797919463,
-1.02934740992906));
#34240=CARTESIAN_POINT('Ctrl Pts',(0.092408853249567,7.50891013704819,-1.08034636620825));
#34241=CARTESIAN_POINT('Ctrl Pts',(0.0954064872307011,7.5009451628879,-1.12925696355173));
#34242=CARTESIAN_POINT('Ctrl Pts',(0.0979571981160565,7.4929211943923,-1.1762068370932));
#34243=CARTESIAN_POINT('Ctrl Pts',(0.0999421648727422,7.48667693095503,
-1.21274329394743));
#34244=CARTESIAN_POINT('Ctrl Pts',(0.101656839723846,7.48039623554083,-1.24809198876685));
#34245=CARTESIAN_POINT('Ctrl Pts',(0.103114408059408,7.47412058325023,-1.28234280769482));
#34246=CARTESIAN_POINT('Ctrl Pts',(0.103529836038339,7.47233193191639,-1.29210478463738));
#34247=CARTESIAN_POINT('Ctrl Pts',(0.103924381198659,7.47054363202985,-1.30177759317101));
#34248=CARTESIAN_POINT('Ctrl Pts',(0.104298386010432,7.4687566434487,-1.31136316830816));
#34249=CARTESIAN_POINT('Ctrl Pts',(0.105984622059959,7.46069983650188,-1.35458063996335));
#34250=CARTESIAN_POINT('Ctrl Pts',(0.10725238266638,7.45267074068681,-1.39602675468791));
#34251=CARTESIAN_POINT('Ctrl Pts',(0.108116417619798,7.44468165502368,-1.43608914702523));
#34252=CARTESIAN_POINT('Ctrl Pts',(0.108980452573216,7.43669256936054,-1.47615153936256));
#34253=CARTESIAN_POINT('Ctrl Pts',(0.109440821161578,7.42874335524718,-1.51483017857665));
#34254=CARTESIAN_POINT('Ctrl Pts',(0.109518134026665,7.42097012443101,-1.55188588983467));
#34255=CARTESIAN_POINT('Ctrl Pts',(0.109549379528338,7.41782862273911,-1.56686171936613));
#34256=CARTESIAN_POINT('Ctrl Pts',(0.109517733599107,7.41471541142924,-1.58157153761866));
#34257=CARTESIAN_POINT('Ctrl Pts',(0.1094247017107,7.41162697964378,-1.59605530105345));
#34258=CARTESIAN_POINT('Ctrl Pts',(0.109287538484548,7.40707349508385,-1.61740969634247));
#34259=CARTESIAN_POINT('Ctrl Pts',(0.109017347905158,7.40257412495728,-1.63827290333177));
#34260=CARTESIAN_POINT('Ctrl Pts',(0.108614123231762,7.39811498650203,-1.65876475481342));
#34261=CARTESIAN_POINT('Ctrl Pts',(0.108197298559464,7.3935054498145,-1.67994775734813));
#34262=CARTESIAN_POINT('Ctrl Pts',(0.107636013113357,7.38893509013303,-1.70073180908713));
#34263=CARTESIAN_POINT('Ctrl Pts',(0.106916313695485,7.38432485973754,-1.72156283502745));
#34264=CARTESIAN_POINT('Ctrl Pts',(0.106467581648175,7.38145038454336,-1.73455096407919));
#34265=CARTESIAN_POINT('Ctrl Pts',(0.105956508353038,7.37856013433668,-1.74755699928645));
#34266=CARTESIAN_POINT('Ctrl Pts',(0.105370932926494,7.37563206590809,-1.76068425372961));
#34267=CARTESIAN_POINT('Ctrl Pts',(0.104614139175394,7.37184784992309,-1.77764982926665));
#34268=CARTESIAN_POINT('Ctrl Pts',(0.10373062228697,7.36799661236927,-1.79481376372923));
#34269=CARTESIAN_POINT('Ctrl Pts',(0.102682811222867,7.36401912913252,-1.81251182586846));
#34270=CARTESIAN_POINT('Ctrl Pts',(0.101740077804235,7.36044051987958,-1.82843507309811));
#34271=CARTESIAN_POINT('Ctrl Pts',(0.100664403176793,7.35675971869643,-1.84479084066697));
#34272=CARTESIAN_POINT('Ctrl Pts',(0.0993976726188921,7.35292665555006,
-1.86180605447627));
#34273=CARTESIAN_POINT('Ctrl Pts',(0.0992357132673436,7.35243657467393,
-1.86398155500227));
#34274=CARTESIAN_POINT('Ctrl Pts',(0.0990705841488978,7.35194399434768,
-1.86616780777751));
#34275=CARTESIAN_POINT('Ctrl Pts',(0.0989021290733927,7.35144880143277,
-1.86836524213778));
#34276=CARTESIAN_POINT('Ctrl Pts',(0.0971030163999783,7.3461601044533,-1.89183400373318));
#34277=CARTESIAN_POINT('Ctrl Pts',(0.0949363222751479,7.34058460186587,
-1.91658901567847));
#34278=CARTESIAN_POINT('Ctrl Pts',(0.0922869113983884,7.33481922105929,
-1.94227889863271));
#34279=CARTESIAN_POINT('Ctrl Pts',(0.0905915320651806,7.33112990750159,
-1.95871806139723));
#34280=CARTESIAN_POINT('Ctrl Pts',(0.0886979474294951,7.32736294710167,
-1.97553922387949));
#34281=CARTESIAN_POINT('Ctrl Pts',(0.0865694808503494,7.32354392192484,
-1.99264108439717));
#34282=CARTESIAN_POINT('Ctrl Pts',(0.4441505898026,7.871213650645,-0.09177744215336));
#34283=CARTESIAN_POINT('Ctrl Pts',(0.4433243095181,7.871068290275,-0.09821494507687));
#34284=CARTESIAN_POINT('Ctrl Pts',(0.431912656318,7.868855063663,-0.1870059243154));
#34285=CARTESIAN_POINT('Ctrl Pts',(0.4105084687883,7.85942783985,-0.3505980872272));
#34286=CARTESIAN_POINT('Ctrl Pts',(0.3806737777609,7.833726074243,-0.572222828126));
#34287=CARTESIAN_POINT('Ctrl Pts',(0.3530194781211,7.800140145157,-0.7712432567487));
#34288=CARTESIAN_POINT('Ctrl Pts',(0.3268098245238,7.761290681241,-0.9498918064517));
#34289=CARTESIAN_POINT('Ctrl Pts',(0.3017673989979,7.719035433425,-1.110873752664));
#34290=CARTESIAN_POINT('Ctrl Pts',(0.27750044695,7.674652834655,-1.256626058432));
#34291=CARTESIAN_POINT('Ctrl Pts',(0.2538473285845,7.629290513098,-1.388548718731));
#34292=CARTESIAN_POINT('Ctrl Pts',(0.2306285320351,7.583757910898,-1.508164313343));
#34293=CARTESIAN_POINT('Ctrl Pts',(0.2077459409351,7.538748776583,-1.616570111714));
#34294=CARTESIAN_POINT('Ctrl Pts',(0.1848495979167,7.494336451159,-1.715813080171));
#34295=CARTESIAN_POINT('Ctrl Pts',(0.1609461047851,7.449222130099,-1.810174952063));
#34296=CARTESIAN_POINT('Ctrl Pts',(0.1337042946379,7.399946526947,-1.90703230257));
#34297=CARTESIAN_POINT('Ctrl Pts',(0.1104061460154,7.3606094987,-1.979544729913));
#34298=CARTESIAN_POINT('Ctrl Pts',(0.09567837415138,7.337327167199,-2.020855911046));
#34299=CARTESIAN_POINT('Ctrl Pts',(0.09337813193118,7.333727280678,-2.027206328594));
#34300=CARTESIAN_POINT('Ctrl Pts',(0.3516735936866,7.689614433451,-0.07882304454856));
#34301=CARTESIAN_POINT('Ctrl Pts',(0.350847645443,7.689489554466,-0.08497125195246));
#34302=CARTESIAN_POINT('Ctrl Pts',(0.3394417549388,7.687568105211,-0.1697648837862));
#34303=CARTESIAN_POINT('Ctrl Pts',(0.3180756196168,7.678929865608,-0.3258309287609));
#34304=CARTESIAN_POINT('Ctrl Pts',(0.2882640593889,7.654890630862,-0.5374733705245));
#34305=CARTESIAN_POINT('Ctrl Pts',(0.2606668037202,7.623311287819,-0.72733912594));
#34306=CARTESIAN_POINT('Ctrl Pts',(0.2345362971087,7.586713311666,-0.8976506379897));
#34307=CARTESIAN_POINT('Ctrl Pts',(0.2095892877477,7.546871805083,-1.051034607769));
#34308=CARTESIAN_POINT('Ctrl Pts',(0.1854463195427,7.505030986202,-1.189768938416));
#34309=CARTESIAN_POINT('Ctrl Pts',(0.1619437477529,7.46228752288,-1.315220328419));
#34310=CARTESIAN_POINT('Ctrl Pts',(0.138910375472,7.419427010875,-1.428824558871));
#34311=CARTESIAN_POINT('Ctrl Pts',(0.1162527672911,7.377116859745,-1.53163170281));
#34312=CARTESIAN_POINT('Ctrl Pts',(0.09364048230928,7.335454123773,-1.625553474636));
#34313=CARTESIAN_POINT('Ctrl Pts',(0.0700942572526,7.293224081819,-1.714671038855));
#34314=CARTESIAN_POINT('Ctrl Pts',(0.04337896997814,7.247270768707,-1.805808681845));
#34315=CARTESIAN_POINT('Ctrl Pts',(0.02066764874285,7.210775637613,-1.87369224103));
#34316=CARTESIAN_POINT('Ctrl Pts',(0.006407516092696,7.189293884623,-1.912158009393));
#34317=CARTESIAN_POINT('Ctrl Pts',(0.004182600943529,7.185975364974,-1.918065761637));
#34318=CARTESIAN_POINT('Ctrl Pts',(0.1756764843762,7.588507551776,-0.05645169963136));
#34319=CARTESIAN_POINT('Ctrl Pts',(0.17485115759,7.588418024305,-0.06243513417407));
#34320=CARTESIAN_POINT('Ctrl Pts',(0.1634561005123,7.586989322095,-0.1449398854917));
#34321=CARTESIAN_POINT('Ctrl Pts',(0.1421623841087,7.579420771145,-0.2964239473798));
#34322=CARTESIAN_POINT('Ctrl Pts',(0.1123948451765,7.557190120433,-0.5023434273139));
#34323=CARTESIAN_POINT('Ctrl Pts',(0.08490615253084,7.527597874674,-0.6866379321841));
#34324=CARTESIAN_POINT('Ctrl Pts',(0.05892627421298,7.49314065782,-0.8516776174722));
#34325=CARTESIAN_POINT('Ctrl Pts',(0.03416085577375,7.455547930377,-1.000117458604));
#34326=CARTESIAN_POINT('Ctrl Pts',(0.01025384696161,7.416083886949,-1.134060645635));
#34327=CARTESIAN_POINT('Ctrl Pts',(-0.01296221266884,7.375817217032,-1.254905212899));
#34328=CARTESIAN_POINT('Ctrl Pts',(-0.03564269543798,7.335541213803,-1.36400630926));
#34329=CARTESIAN_POINT('Ctrl Pts',(-0.05787212820738,7.295916502886,-1.462390721413));
#34330=CARTESIAN_POINT('Ctrl Pts',(-0.07994380918605,7.257099508462,-1.551819675948));
#34331=CARTESIAN_POINT('Ctrl Pts',(-0.1028101008255,7.217967061454,-1.636246280066));
#34332=CARTESIAN_POINT('Ctrl Pts',(-0.1285233380393,7.175787023336,-1.721805374644));
#34333=CARTESIAN_POINT('Ctrl Pts',(-0.1501178409,7.142734270604,-1.784726132061));
#34334=CARTESIAN_POINT('Ctrl Pts',(-0.1634879877075,7.123558780129,-1.819892205208));
#34335=CARTESIAN_POINT('Ctrl Pts',(-0.1655695444196,7.12060357232,-1.825280786222));
#34336=CARTESIAN_POINT('Ctrl Pts',(-0.02667784573404,7.600731964282,-0.03192949709627));
#34337=CARTESIAN_POINT('Ctrl Pts',(-0.02750246349208,7.600681176477,-0.0379261987546));
#34338=CARTESIAN_POINT('Ctrl Pts',(-0.03888513505015,7.599786149475,-0.1205939522383));
#34339=CARTESIAN_POINT('Ctrl Pts',(-0.0600955870907,7.593220562632,-0.271928368777));
#34340=CARTESIAN_POINT('Ctrl Pts',(-0.0898125121055,7.572357130986,-0.4782430106894));
#34341=CARTESIAN_POINT('Ctrl Pts',(-0.1171763833487,7.544087095491,-0.6623591991885));
#34342=CARTESIAN_POINT('Ctrl Pts',(-0.1429830753057,7.510964602637,-0.8269045289223));
#34343=CARTESIAN_POINT('Ctrl Pts',(-0.1675397077981,7.474725301153,-0.974659914962));
#34344=CARTESIAN_POINT('Ctrl Pts',(-0.1911754199796,7.43670106516,-1.10759492696));
#34345=CARTESIAN_POINT('Ctrl Pts',(-0.2140620594393,7.39796467495,-1.227193389711));
#34346=CARTESIAN_POINT('Ctrl Pts',(-0.2363368040245,7.359346164853,-1.334762175216));
#34347=CARTESIAN_POINT('Ctrl Pts',(-0.2580739379069,7.321521134976,-1.43133625717));
#34348=CARTESIAN_POINT('Ctrl Pts',(-0.2795240541205,7.284721753007,-1.518560016082));
#34349=CARTESIAN_POINT('Ctrl Pts',(-0.3016085856319,7.247894134993,-1.60037260569));
#34350=CARTESIAN_POINT('Ctrl Pts',(-0.3261697059415,7.208712817874,-1.682306192782));
#34351=CARTESIAN_POINT('Ctrl Pts',(-0.3464801359011,7.178584859169,-1.741542105518));
#34352=CARTESIAN_POINT('Ctrl Pts',(-0.3588270127402,7.161472253843,-1.774025923849));
#34353=CARTESIAN_POINT('Ctrl Pts',(-0.3607437416807,7.158844301156,-1.778987451663));
#34354=CARTESIAN_POINT('Ctrl Pts',(-0.1093368573593,2.267338017643,-3.503111485524));
#34355=CARTESIAN_POINT('Ctrl Pts',(-0.1083830870411,2.261715711184,-3.504763464173));
#34356=CARTESIAN_POINT('Ctrl Pts',(-0.1024109572104,2.226653555098,-3.515107496462));
#34357=CARTESIAN_POINT('Ctrl Pts',(-0.09166803071108,2.165207556871,-3.533714790978));
#34358=CARTESIAN_POINT('Ctrl Pts',(-0.07707930366217,2.085794285077,-3.558983207447));
#34359=CARTESIAN_POINT('Ctrl Pts',(-0.06322441812029,2.014421046044,-3.582980573135));
#34360=CARTESIAN_POINT('Ctrl Pts',(-0.05003765588103,1.950448046759,-3.605820715331));
#34361=CARTESIAN_POINT('Ctrl Pts',(-0.03741167371015,1.893137336415,-3.627689557913));
#34362=CARTESIAN_POINT('Ctrl Pts',(-0.02742060432543,1.85109146855,-3.644994597799));
#34363=CARTESIAN_POINT('Ctrl Pts',(-0.0216547415189,1.828308833643,-3.654981365119));
#34364=CARTESIAN_POINT('Ctrl Pts',(-0.020047604698,1.822076746678,-3.657765007738));
#34365=CARTESIAN_POINT('Ctrl Pts',(-0.08914856077128,2.30389779074,-3.615858489728));
#34366=CARTESIAN_POINT('Ctrl Pts',(-0.08820964158498,2.298363302287,-3.617484745462));
#34367=CARTESIAN_POINT('Ctrl Pts',(-0.08233249861155,2.263860250828,-3.62766425569));
#34368=CARTESIAN_POINT('Ctrl Pts',(-0.07178380934417,2.203526797407,-3.645935121454));
#34369=CARTESIAN_POINT('Ctrl Pts',(-0.0575231657281,2.125905672972,-3.670635280746));
#34370=CARTESIAN_POINT('Ctrl Pts',(-0.04406846217497,2.056600282344,-3.6939395109));
#34371=CARTESIAN_POINT('Ctrl Pts',(-0.03135539063293,1.994934720186,-3.715959196734));
#34372=CARTESIAN_POINT('Ctrl Pts',(-0.01932659075308,1.940347123965,-3.736793689271));
#34373=CARTESIAN_POINT('Ctrl Pts',(-0.009956155822182,1.900928630607,-3.753023758685));
#34374=CARTESIAN_POINT('Ctrl Pts',(-0.004648641143993,1.87996086452,-3.762216643767));
#34375=CARTESIAN_POINT('Ctrl Pts',(-0.003177995106695,1.874260366703,-3.76476387742));
#34376=CARTESIAN_POINT('Ctrl Pts',(-0.04841933904592,2.342100691839,-3.722337292106));
#34377=CARTESIAN_POINT('Ctrl Pts',(-0.04749593845507,2.336657968252,-3.723936668845));
#34378=CARTESIAN_POINT('Ctrl Pts',(-0.04171805139089,2.302739149594,-3.733944262798));
#34379=CARTESIAN_POINT('Ctrl Pts',(-0.03137232907633,2.243568242753,-3.751863579488));
#34380=CARTESIAN_POINT('Ctrl Pts',(-0.0174545141457,2.167819811241,-3.775969942078));
#34381=CARTESIAN_POINT('Ctrl Pts',(-0.004417978201916,2.10067520558,-3.798549884687));
#34382=CARTESIAN_POINT('Ctrl Pts',(0.007800113273371,2.041420785091,-3.819712239893));
#34383=CARTESIAN_POINT('Ctrl Pts',(0.01920489134338,1.989678689559,-3.839465894962));
#34384=CARTESIAN_POINT('Ctrl Pts',(0.0279267982543,1.953005654392,-3.854572680865));
#34385=CARTESIAN_POINT('Ctrl Pts',(0.03275536498868,1.933934323872,-3.862936003777));
#34386=CARTESIAN_POINT('Ctrl Pts',(0.03408338585636,1.928789306735,-3.865236203394));
#34387=CARTESIAN_POINT('Ctrl Pts',(0.01154374246066,2.380720729223,-3.819130818924));
#34388=CARTESIAN_POINT('Ctrl Pts',(0.01245145500894,2.375370772478,-3.820703023177));
#34389=CARTESIAN_POINT('Ctrl Pts',(0.01812900239146,2.342042565842,-3.830536823706));
#34390=CARTESIAN_POINT('Ctrl Pts',(0.02826954156393,2.284046899391,-3.848100752769));
#34391=CARTESIAN_POINT('Ctrl Pts',(0.04184078447309,2.210191608676,-3.87160683501));
#34392=CARTESIAN_POINT('Ctrl Pts',(0.05445458684907,2.145231381526,-3.893454581602));
#34393=CARTESIAN_POINT('Ctrl Pts',(0.06617229358387,2.088414429887,-3.913750245015));
#34394=CARTESIAN_POINT('Ctrl Pts',(0.07694623617531,2.039548904977,-3.932411260981));
#34395=CARTESIAN_POINT('Ctrl Pts',(0.08501253379338,2.005651305572,-3.946382498285));
#34396=CARTESIAN_POINT('Ctrl Pts',(0.08935692296802,1.988497117739,-3.953907201063));
#34397=CARTESIAN_POINT('Ctrl Pts',(0.09054076134808,1.983913646559,-3.955957669285));
#34398=CARTESIAN_POINT('Ctrl Pts',(-1.96632830365993E-8,2.35518147812891,
-3.79999996594227));
#34399=CARTESIAN_POINT('Ctrl Pts',(-0.00357935201635383,2.31983212279541,
-3.79380037680371));
#34400=CARTESIAN_POINT('Ctrl Pts',(-0.00668325372236177,2.2859060985581,
-3.78742526700976));
#34401=CARTESIAN_POINT('Ctrl Pts',(-0.00933017063364458,2.25352492902307,
-3.7809687846852));
#34402=CARTESIAN_POINT('Ctrl Pts',(-0.0117790651800547,2.22356627443035,
-3.77499532768463));
#34403=CARTESIAN_POINT('Ctrl Pts',(-0.0138399798130133,2.19492932956879,
-3.76895400168668));
#34404=CARTESIAN_POINT('Ctrl Pts',(-0.0155599555445709,2.16735773225228,
-3.76283182924018));
#34405=CARTESIAN_POINT('Ctrl Pts',(-0.0156990395242569,2.16512818481697,
-3.76233676637821));
#34406=CARTESIAN_POINT('Ctrl Pts',(-0.0158358799969592,2.16290558066701,
-3.76184117210061));
#34407=CARTESIAN_POINT('Ctrl Pts',(-0.0159704944353338,2.16068977328618,
-3.76134503811409));
#34408=CARTESIAN_POINT('Ctrl Pts',(-0.0177698122251964,2.13107228434972,
-3.75471348566788));
#34409=CARTESIAN_POINT('Ctrl Pts',(-0.0191729161038338,2.10267382287069,
-3.74798548303885));
#34410=CARTESIAN_POINT('Ctrl Pts',(-0.0202111003075097,2.07533858847079,
-3.74115901064695));
#34411=CARTESIAN_POINT('Ctrl Pts',(-0.0211069940837041,2.05174983968905,
-3.73526815418081));
#34412=CARTESIAN_POINT('Ctrl Pts',(-0.0217311225486786,2.02895149477714,
-3.7293043052384));
#34413=CARTESIAN_POINT('Ctrl Pts',(-0.0220993771361064,2.00682851987961,
-3.72324124653658));
#34414=CARTESIAN_POINT('Ctrl Pts',(-0.0221578652114335,2.00331483595973,
-3.7222782805718));
#34415=CARTESIAN_POINT('Ctrl Pts',(-0.0222098601880988,1.99981809119264,
-3.72131282557032));
#34416=CARTESIAN_POINT('Ctrl Pts',(-0.0222553839599064,1.99633772653508,
-3.72034478903747));
#34417=CARTESIAN_POINT('Ctrl Pts',(-0.0225419057442877,1.97443268105259,
-3.71425206992115));
#34418=CARTESIAN_POINT('Ctrl Pts',(-0.022573946896536,1.95318010085027,
-3.70805690800793));
#34419=CARTESIAN_POINT('Ctrl Pts',(-0.0223572182489124,1.93246260055955,
-3.70170259035036));
#34420=CARTESIAN_POINT('Ctrl Pts',(-0.0223227123773963,1.92916411920508,
-3.70069090467305));
#34421=CARTESIAN_POINT('Ctrl Pts',(-0.0222818493864799,1.92587910948092,
-3.69967520097663));
#34422=CARTESIAN_POINT('Ctrl Pts',(-0.022234595528982,1.92260700285591,
-3.69865526715785));
#34423=CARTESIAN_POINT('Ctrl Pts',(-0.022234582589023,1.92260610682482,
-3.69865498785998));
#34424=CARTESIAN_POINT('Ctrl Pts',(-0.0222345696485847,1.92260521079469,
-3.69865470856179));
#34425=CARTESIAN_POINT('Ctrl Pts',(-0.022234556707667,1.92260431476553,
-3.69865442926329));
#34426=CARTESIAN_POINT('Ctrl Pts',(-0.0219659729272414,1.9040075734149,
-3.69285769595474));
#34427=CARTESIAN_POINT('Ctrl Pts',(-0.0214906543542213,1.88582902904627,
-3.68692322599305));
#34428=CARTESIAN_POINT('Ctrl Pts',(-0.0208084100576887,1.86814906504177,
-3.68086191629441));
#34429=CARTESIAN_POINT('Ctrl Pts',(-0.0206166125285239,1.8631787436642,
-3.67915791637882));
#34430=CARTESIAN_POINT('Ctrl Pts',(-0.0204084646838708,1.85824749485259,
-3.67744394818951));
#34431=CARTESIAN_POINT('Ctrl Pts',(-0.0201840086718301,1.85335644493182,
-3.67572031916525));
#34432=CARTESIAN_POINT('Ctrl Pts',(0.01313183742357,2.35893980927,-3.823805869142));
#34433=CARTESIAN_POINT('Ctrl Pts',(0.01303186504026,2.353957576536,-3.82385436109));
#34434=CARTESIAN_POINT('Ctrl Pts',(0.01123027883039,2.264631434664,-3.82471367541));
#34435=CARTESIAN_POINT('Ctrl Pts',(0.00760883944032,2.10029230713,-3.825952350518));
#34436=CARTESIAN_POINT('Ctrl Pts',(0.002704317644358,1.905594454076,-3.826393794893));
#34437=CARTESIAN_POINT('Ctrl Pts',(-0.0002703855987072,1.795386308729,-3.826069286647));
#34438=CARTESIAN_POINT('Ctrl Pts',(-0.001263515685753,1.759172878611,-3.825885856397));
#34439=CARTESIAN_POINT('Ctrl Pts',(-0.1220155422729,2.480509211462,-3.559282264932));
#34440=CARTESIAN_POINT('Ctrl Pts',(-0.1210052566975,2.475681572059,-3.558834796486));
#34441=CARTESIAN_POINT('Ctrl Pts',(-0.1028036746325,2.389157129411,-3.550915651626));
#34442=CARTESIAN_POINT('Ctrl Pts',(-0.06637047515481,2.230896427315,-3.539852558722));
#34443=CARTESIAN_POINT('Ctrl Pts',(-0.0174057286524,2.046314967408,-3.537170858724));
#34444=CARTESIAN_POINT('Ctrl Pts',(0.01211878202876,1.943696215842,-3.541453508649));
#34445=CARTESIAN_POINT('Ctrl Pts',(0.02195442675702,1.910230935709,-3.543633877626));
#34446=CARTESIAN_POINT('Ctrl Pts',(-0.4243708118278,2.566620235427,-3.494607553578));
#34447=CARTESIAN_POINT('Ctrl Pts',(-0.4230739478696,2.561902098825,-3.492966852937));
#34448=CARTESIAN_POINT('Ctrl Pts',(-0.3995937923515,2.477362178471,-3.463646745939));
#34449=CARTESIAN_POINT('Ctrl Pts',(-0.3487237350337,2.323406995932,-3.413015804336));
#34450=CARTESIAN_POINT('Ctrl Pts',(-0.2708767291174,2.145991261584,-3.365007313014));
#34451=CARTESIAN_POINT('Ctrl Pts',(-0.2195329377334,2.048748290915,-3.345376679566));
#34452=CARTESIAN_POINT('Ctrl Pts',(-0.201883686884,2.017229602646,-3.339993364004));
#34453=CARTESIAN_POINT('Ctrl Pts',(-0.690961983047,2.559466295669,-3.673198060413));
#34454=CARTESIAN_POINT('Ctrl Pts',(-0.6903946011995,2.554739061783,-3.670467876084));
#34455=CARTESIAN_POINT('Ctrl Pts',(-0.6799039890472,2.4700342711,-3.621490833275));
#34456=CARTESIAN_POINT('Ctrl Pts',(-0.6499063603548,2.315721394201,-3.530587976339));
#34457=CARTESIAN_POINT('Ctrl Pts',(-0.5875528502187,2.137710345031,-3.425477056041));
#34458=CARTESIAN_POINT('Ctrl Pts',(-0.5397170591296,2.04002076473,-3.369465755649));
#34459=CARTESIAN_POINT('Ctrl Pts',(-0.5225146677906,2.008340357318,-3.351668795621));
#34460=CARTESIAN_POINT('Origin',(-0.4330128001874,2.355181195091,-4.049999829751));
#34461=CARTESIAN_POINT('Ctrl Pts',(0.1654598430731,3.816833346673,-4.09081615578));
#34462=CARTESIAN_POINT('Ctrl Pts',(0.1654730735783,3.811222474592,-4.090839257127));
#34463=CARTESIAN_POINT('Ctrl Pts',(0.1656678347127,3.645978055895,-4.091179623035));
#34464=CARTESIAN_POINT('Ctrl Pts',(0.1547816615116,3.320020093713,-4.072101884476));
#34465=CARTESIAN_POINT('Ctrl Pts',(0.10512844909,2.829224950023,-3.985158819806));
#34466=CARTESIAN_POINT('Ctrl Pts',(0.04761048988404,2.502918756874,-3.884629417663));
#34467=CARTESIAN_POINT('Ctrl Pts',(0.01060629136168,2.333799331458,-3.820069159035));
#34468=CARTESIAN_POINT('Ctrl Pts',(0.009485886303509,2.328709728431,-3.818114554056));
#34469=CARTESIAN_POINT('Ctrl Pts',(0.07652291890888,3.815887979875,-3.897696692651));
#34470=CARTESIAN_POINT('Ctrl Pts',(0.0765359932756,3.810592215503,-3.897718314945));
#34471=CARTESIAN_POINT('Ctrl Pts',(0.07672846980537,3.654627998194,-3.898036866885));
#34472=CARTESIAN_POINT('Ctrl Pts',(0.0659656221111,3.34697569895,-3.880183328377));
#34473=CARTESIAN_POINT('Ctrl Pts',(0.01686163208697,2.883542177093,-3.798793107701));
#34474=CARTESIAN_POINT('Ctrl Pts',(-0.04004963525953,2.575146492001,-3.704622957279));
#34475=CARTESIAN_POINT('Ctrl Pts',(-0.07668074743997,2.415194449956,-3.644109787001));
#34476=CARTESIAN_POINT('Ctrl Pts',(-0.07778986621121,2.410380629126,-3.642277679727));
#34477=CARTESIAN_POINT('Ctrl Pts',(-0.1058150100366,3.8150580125,-3.788344136655));
#34478=CARTESIAN_POINT('Ctrl Pts',(-0.1058022557841,3.810038889687,-3.788364161843));
#34479=CARTESIAN_POINT('Ctrl Pts',(-0.1056144631364,3.662222079724,-3.788659126644));
#34480=CARTESIAN_POINT('Ctrl Pts',(-0.1161244696433,3.370640483808,-3.772131476753));
#34481=CARTESIAN_POINT('Ctrl Pts',(-0.164102447323,2.930897223765,-3.696717648248));
#34482=CARTESIAN_POINT('Ctrl Pts',(-0.2197698787915,2.637543693865,-3.60930318436));
#34483=CARTESIAN_POINT('Ctrl Pts',(-0.2556360916734,2.485096894578,-3.553035639014));
#34484=CARTESIAN_POINT('Ctrl Pts',(-0.2567220713694,2.480508670394,-3.551331993714));
#34485=CARTESIAN_POINT('Ctrl Pts',(-0.318063882194,3.814632439165,-3.800835044618));
#34486=CARTESIAN_POINT('Ctrl Pts',(-0.3180515005676,3.809755165178,-3.800853910757));
#34487=CARTESIAN_POINT('Ctrl Pts',(-0.317869160152,3.666116041517,-3.801131728292));
#34488=CARTESIAN_POINT('Ctrl Pts',(-0.3280848490852,3.382774370883,-3.785569981205));
#34489=CARTESIAN_POINT('Ctrl Pts',(-0.3747521019391,2.954801064162,-3.714475113467));
#34490=CARTESIAN_POINT('Ctrl Pts',(-0.4289716571276,2.668383658588,-3.631860441071));
#34491=CARTESIAN_POINT('Ctrl Pts',(-0.463947495668,2.519166636135,-3.578558730762));
#34492=CARTESIAN_POINT('Ctrl Pts',(-0.4650065405256,2.5146752703,-3.576944781249));
#34493=CARTESIAN_POINT('Origin',(-0.2886751345948,3.800000001415,-4.3));
#34494=CARTESIAN_POINT('Ctrl Pts',(0.009474644457224,5.271341047008,-3.81809495663));
#34495=CARTESIAN_POINT('Ctrl Pts',(0.01059883418097,5.266234517663,-3.820056164353));
#34496=CARTESIAN_POINT('Ctrl Pts',(0.04384970191935,5.114274997728,-3.878067830231));
#34497=CARTESIAN_POINT('Ctrl Pts',(0.09915364759026,4.8078509,-3.974708076039));
#34498=CARTESIAN_POINT('Ctrl Pts',(0.1527214809499,4.318896431654,-4.068489655631));
#34499=CARTESIAN_POINT('Ctrl Pts',(0.1656911193838,3.973918157182,-4.091220206062));
#34500=CARTESIAN_POINT('Ctrl Pts',(0.1654730928291,3.788778562717,-4.090839298714));
#34501=CARTESIAN_POINT('Ctrl Pts',(0.1654598555027,3.783168271439,-4.090816203677));
#34502=CARTESIAN_POINT('Ctrl Pts',(-0.07780099825573,5.189667390479,-3.64225930114));
#34503=CARTESIAN_POINT('Ctrl Pts',(-0.07668813259209,5.184837560174,-3.644097597763));
#34504=CARTESIAN_POINT('Ctrl Pts',(-0.04377252156913,5.041115244204,-3.698472705015));
#34505=CARTESIAN_POINT('Ctrl Pts',(0.01095113947594,4.751489226246,-3.78900612516));
#34506=CARTESIAN_POINT('Ctrl Pts',(0.06392901869112,4.289755505572,-3.876803425784));
#34507=CARTESIAN_POINT('Ctrl Pts',(0.07675145353046,3.96415083195,-3.898074824767));
#34508=CARTESIAN_POINT('Ctrl Pts',(0.07653600951855,3.789408763611,-3.897718345517));
#34509=CARTESIAN_POINT('Ctrl Pts',(0.07652293035462,3.784113547511,-3.897696729157));
#34510=CARTESIAN_POINT('Ctrl Pts',(-0.2567329809504,5.119537094511,-3.551314900398));
#34511=CARTESIAN_POINT('Ctrl Pts',(-0.2556433318048,5.114933610283,-3.553024302135));
#34512=CARTESIAN_POINT('Ctrl Pts',(-0.2234150620255,4.977955008216,-3.603584480384));
#34513=CARTESIAN_POINT('Ctrl Pts',(-0.1698810969299,4.702401341059,-3.687639726247));
#34514=CARTESIAN_POINT('Ctrl Pts',(-0.1181127380514,4.264172564127,-3.769003987438));
#34515=CARTESIAN_POINT('Ctrl Pts',(-0.1055920991109,3.955575758191,-3.788694233295));
#34516=CARTESIAN_POINT('Ctrl Pts',(-0.1058022484096,3.789962038378,-3.788364190614));
#34517=CARTESIAN_POINT('Ctrl Pts',(-0.1058150033097,3.784943435394,-3.788344170997));
#34518=CARTESIAN_POINT('Ctrl Pts',(-0.4650171874587,5.085369528077,-3.576928594638));
#34519=CARTESIAN_POINT('Ctrl Pts',(-0.4639545632973,5.080863223263,-3.578547998901));
#34520=CARTESIAN_POINT('Ctrl Pts',(-0.4325263870696,4.946786683863,-3.626443236047));
#34521=CARTESIAN_POINT('Ctrl Pts',(-0.380377277119,4.677679646005,-3.705904659284));
#34522=CARTESIAN_POINT('Ctrl Pts',(-0.3300168497897,4.251055587502,-3.7826271049));
#34523=CARTESIAN_POINT('Ctrl Pts',(-0.3178475137206,3.951178776577,-3.801164753472));
#34524=CARTESIAN_POINT('Ctrl Pts',(-0.3180514997547,3.790245736745,-3.800853950616));
#34525=CARTESIAN_POINT('Ctrl Pts',(-0.3180638771985,3.785368968127,-3.800835089823));
#34526=CARTESIAN_POINT('Origin',(1.,18.3911851122,3.532050807569));
#34527=CARTESIAN_POINT('',(0.,0.,0.));
#34528=CARTESIAN_POINT('Origin',(0.,0.,-12.));
#34529=CARTESIAN_POINT('',(2.87791997799628E-16,2.35,-12.));
#34530=CARTESIAN_POINT('Origin',(0.,0.,-12.));
#34531=CARTESIAN_POINT('',(-0.6490486745229,-0.4,-12.));
#34532=CARTESIAN_POINT('',(-0.4,-0.6490486745229,-12.));
#34533=CARTESIAN_POINT('Origin',(-0.650954959386273,-0.650954959386273,
-12.));
#34534=CARTESIAN_POINT('',(-0.4,-1.100951325477,-12.));
#34535=CARTESIAN_POINT('',(-0.4,-0.6490486745229,-12.));
#34536=CARTESIAN_POINT('',(-0.1509513254771,-1.35,-12.));
#34537=CARTESIAN_POINT('Origin',(-0.149045040613789,-1.09904504061379,-12.));
#34538=CARTESIAN_POINT('',(0.1509513254771,-1.35,-12.));
#34539=CARTESIAN_POINT('',(-0.1509513254771,-1.35,-12.));
#34540=CARTESIAN_POINT('',(0.4,-1.100951325477,-12.));
#34541=CARTESIAN_POINT('Origin',(0.149045040614538,-1.09904504061454,-12.));
#34542=CARTESIAN_POINT('',(0.4,-0.6490486745229,-12.));
#34543=CARTESIAN_POINT('',(0.4,-1.100951325477,-12.));
#34544=CARTESIAN_POINT('',(0.6490486745229,-0.4,-12.));
#34545=CARTESIAN_POINT('Origin',(0.650954959386273,-0.650954959386273,-12.));
#34546=CARTESIAN_POINT('',(1.100951325477,-0.4,-12.));
#34547=CARTESIAN_POINT('',(0.6490486745229,-0.4,-12.));
#34548=CARTESIAN_POINT('',(1.35,-0.1509513254771,-12.));
#34549=CARTESIAN_POINT('Origin',(1.09904504061396,-0.149045040613957,-12.));
#34550=CARTESIAN_POINT('',(1.35,0.1509513254771,-12.));
#34551=CARTESIAN_POINT('',(1.35,-0.1509513254771,-12.));
#34552=CARTESIAN_POINT('',(1.100951325477,0.4,-12.));
#34553=CARTESIAN_POINT('Origin',(1.09904504061419,0.149045040614192,-12.));
#34554=CARTESIAN_POINT('',(0.6490486745229,0.4,-12.));
#34555=CARTESIAN_POINT('',(1.100951325477,0.4,-12.));
#34556=CARTESIAN_POINT('',(0.4,0.6490486745229,-12.));
#34557=CARTESIAN_POINT('Origin',(0.650954959386273,0.650954959386273,-12.));
#34558=CARTESIAN_POINT('',(0.4,1.100951325477,-12.));
#34559=CARTESIAN_POINT('',(0.4,0.6490486745229,-12.));
#34560=CARTESIAN_POINT('',(0.1509513254771,1.35,-12.));
#34561=CARTESIAN_POINT('Origin',(0.149045040614081,1.09904504061408,-12.));
#34562=CARTESIAN_POINT('',(-0.1509513254771,1.35,-12.));
#34563=CARTESIAN_POINT('',(0.1509513254771,1.35,-12.));
#34564=CARTESIAN_POINT('',(-0.4,1.100951325477,-12.));
#34565=CARTESIAN_POINT('Origin',(-0.149045040614321,1.09904504061432,-12.));
#34566=CARTESIAN_POINT('',(-0.4,0.6490486745229,-12.));
#34567=CARTESIAN_POINT('',(-0.4,1.100951325477,-12.));
#34568=CARTESIAN_POINT('',(-0.6490486745229,0.4,-12.));
#34569=CARTESIAN_POINT('Origin',(-0.650954959386273,0.650954959386273,-12.));
#34570=CARTESIAN_POINT('',(-1.100951325477,0.4,-12.));
#34571=CARTESIAN_POINT('',(-0.6490486745229,0.4,-12.));
#34572=CARTESIAN_POINT('',(-1.35,0.1509513254771,-12.));
#34573=CARTESIAN_POINT('Origin',(-1.09904504061453,0.149045040614529,-12.));
#34574=CARTESIAN_POINT('',(-1.35,-0.1509513254771,-12.));
#34575=CARTESIAN_POINT('',(-1.35,0.1509513254771,-12.));
#34576=CARTESIAN_POINT('',(-1.100951325477,-0.4,-12.));
#34577=CARTESIAN_POINT('Origin',(-1.09904504061437,-0.14904504061437,-12.));
#34578=CARTESIAN_POINT('',(-1.100951325477,-0.4,-12.));
#34579=CARTESIAN_POINT('Origin',(0.,0.,0.6));
#34580=CARTESIAN_POINT('',(2.87791997799628E-16,2.35,-11.75));
#34581=CARTESIAN_POINT('',(2.87791997799628E-16,2.35,0.6));
#34582=CARTESIAN_POINT('Origin',(0.,0.,-11.75));
#34583=CARTESIAN_POINT('Origin',(0.,0.,-11.125));
#34584=CARTESIAN_POINT('',(1.34711147906209E-16,1.1,-10.5));
#34585=CARTESIAN_POINT('',(2.11251572852918E-16,1.725,-11.125));
#34586=CARTESIAN_POINT('Origin',(0.,0.,-10.5));
#34587=CARTESIAN_POINT('Origin',(0.,0.,-10.00502525317));
#34588=CARTESIAN_POINT('',(1.34711147906209E-16,1.1,-9.510050506339));
#34589=CARTESIAN_POINT('Origin',(1.95328071842744E-16,1.594974746831,-10.00502525317));
#34590=CARTESIAN_POINT('',(0.,-1.1,-9.510050506339));
#34591=CARTESIAN_POINT('Origin',(0.,0.,-9.510050506339));
#34592=CARTESIAN_POINT('Origin',(0.,0.,-9.510050506339));
#34593=CARTESIAN_POINT('Origin',(0.,0.,-9.435050506339));
#34594=CARTESIAN_POINT('',(1.18854637777596,-0.387097539267644,-9.36025909322078));
#34595=CARTESIAN_POINT('',(1.1909259399931,-0.379730701223331,-9.360050506339));
#34596=CARTESIAN_POINT('Ctrl Pts',(1.18855167546869,-0.387098068634525,
-9.36027610426639));
#34597=CARTESIAN_POINT('Ctrl Pts',(1.18935069806761,-0.384644737745942,
-9.36020090495726));
#34598=CARTESIAN_POINT('Ctrl Pts',(1.19014212463371,-0.382188932913971,
-9.36012570564813));
#34599=CARTESIAN_POINT('Ctrl Pts',(1.1909259399931,-0.379730701223331,-9.360050506339));
#34600=CARTESIAN_POINT('',(1.53080849893419E-16,-1.25,-9.360050506339));
#34601=CARTESIAN_POINT('Origin',(0.,0.,-9.360050506339));
#34602=CARTESIAN_POINT('',(1.43895998899814E-16,-1.175,-9.435050506339));
#34603=CARTESIAN_POINT('Origin',(0.,0.,-9.360050506339));
#34604=CARTESIAN_POINT('Origin',(0.,0.,0.6));
#34605=CARTESIAN_POINT('',(1.18816042873021,-0.386967048621457,-8.91034431420074));
#34606=CARTESIAN_POINT('Ctrl Pts',(1.18855640372918,-0.38708355061195,-8.91058202070716));
#34607=CARTESIAN_POINT('Ctrl Pts',(1.16413132682989,-0.462081781651053,
-8.91508847295526));
#34608=CARTESIAN_POINT('Ctrl Pts',(1.13266199825274,-0.534601882845992,
-8.91946732035472));
#34609=CARTESIAN_POINT('Ctrl Pts',(1.06943293093651,-0.649247028299995,
-8.9267268440218));
#34610=CARTESIAN_POINT('Ctrl Pts',(1.04147855168549,-0.693203093692481,
-8.92960709921868));
#34611=CARTESIAN_POINT('Ctrl Pts',(0.97337862165096,-0.786826391411868,
-8.93616039337431));
#34612=CARTESIAN_POINT('Ctrl Pts',(0.932008000915598,-0.8354165182367,-8.93989564203244));
#34613=CARTESIAN_POINT('Ctrl Pts',(0.832546666127682,-0.935610250253769,
-8.94824133870191));
#34614=CARTESIAN_POINT('Ctrl Pts',(0.772978226416659,-0.985396518974392,
-8.95282616050993));
#34615=CARTESIAN_POINT('Ctrl Pts',(0.618671935476158,-1.09170780359273,
-8.96367433065787));
#34616=CARTESIAN_POINT('Ctrl Pts',(0.520329667238918,-1.14185818423537,
-8.96976236919656));
#34617=CARTESIAN_POINT('Ctrl Pts',(0.371691624455368,-1.19441355795944,
-8.97850737152109));
#34618=CARTESIAN_POINT('Ctrl Pts',(0.325816418750769,-1.2077341218078,-8.98115804797177));
#34619=CARTESIAN_POINT('Ctrl Pts',(0.220615147060026,-1.23184946901154,
-8.98728686123821));
#34620=CARTESIAN_POINT('Ctrl Pts',(0.161047964386293,-1.24104231737691,
-8.99082088203554));
#34621=CARTESIAN_POINT('Ctrl Pts',(0.0238806519370219,-1.2521682136863,
-8.99895621396837));
#34622=CARTESIAN_POINT('Ctrl Pts',(-0.0537157585731863,-1.25124389506131,
-9.00353896719078));
#34623=CARTESIAN_POINT('Ctrl Pts',(-0.239568482987995,-1.23169960660012,
-9.01435748756445));
#34624=CARTESIAN_POINT('Ctrl Pts',(-0.346435839153362,-1.20601051855738,
-9.02042076300827));
#34625=CARTESIAN_POINT('Ctrl Pts',(-0.493347783717673,-1.14952465294486,
-9.02915104624019));
#34626=CARTESIAN_POINT('Ctrl Pts',(-0.537072452143536,-1.12975739849677,
-9.03181314963083));
#34627=CARTESIAN_POINT('Ctrl Pts',(-0.632848812995777,-1.07963919468376,
-9.03795036581202));
#34628=CARTESIAN_POINT('Ctrl Pts',(-0.684056972718885,-1.047942167664,-9.04148084445673));
#34629=CARTESIAN_POINT('Ctrl Pts',(-0.795576763520356,-0.967246630185234,
-9.04961796971787));
#34630=CARTESIAN_POINT('Ctrl Pts',(-0.854015446033157,-0.916060693483113,
-9.0542061050254));
#34631=CARTESIAN_POINT('Ctrl Pts',(-0.983480523777688,-0.779436108665668,
-9.06510343699372));
#34632=CARTESIAN_POINT('Ctrl Pts',(-1.04861434943958,-0.689321925959037,
-9.07123258517349));
#34633=CARTESIAN_POINT('Ctrl Pts',(-1.12346025073986,-0.550074277954606,
-9.08000220024469));
#34634=CARTESIAN_POINT('Ctrl Pts',(-1.14349938581666,-0.507102987868424,
-9.08263399136271));
#34635=CARTESIAN_POINT('Ctrl Pts',(-1.18338925656768,-0.407094063396869,
-9.08874989646326));
#34636=CARTESIAN_POINT('Ctrl Pts',(-1.20164379046778,-0.349551485777399,
-9.09229079738387));
#34637=CARTESIAN_POINT('Ctrl Pts',(-1.23366235105788,-0.21575659514829,
-9.10042397685363));
#34638=CARTESIAN_POINT('Ctrl Pts',(-1.24464131079082,-0.139078612350456,
-9.10499760044744));
#34639=CARTESIAN_POINT('Ctrl Pts',(-1.25311600265331,0.0319140825237386,
-9.11490711541765));
#34640=CARTESIAN_POINT('Ctrl Pts',(-1.24718126828869,0.125932814875664,
-9.12015487713516));
#34641=CARTESIAN_POINT('Ctrl Pts',(-1.22089657875062,0.274054897676782,
-9.12849996685543));
#34642=CARTESIAN_POINT('Ctrl Pts',(-1.20725839404362,0.328970048428431,
-9.13161923643358));
#34643=CARTESIAN_POINT('Ctrl Pts',(-1.17214728603828,0.438122683060954,
-9.13809282547281));
#34644=CARTESIAN_POINT('Ctrl Pts',(-1.15050467962027,0.492156612235245,
-9.1414772579062));
#34645=CARTESIAN_POINT('Ctrl Pts',(-1.06622963442149,0.666312641266624,
-9.15289125023255));
#34646=CARTESIAN_POINT('Ctrl Pts',(-0.987868291319226,0.777780814022605,
-9.16085817819223));
#34647=CARTESIAN_POINT('Ctrl Pts',(-0.835093386727763,0.933813314838567,
-9.17315703402815));
#34648=CARTESIAN_POINT('Ctrl Pts',(-0.771268030342051,0.987184811152829,
-9.17770514022099));
#34649=CARTESIAN_POINT('Ctrl Pts',(-0.657321116790375,1.06462642447898,
-9.1853936547973));
#34650=CARTESIAN_POINT('Ctrl Pts',(-0.610048486753047,1.09240141502545,
-9.18849779461628));
#34651=CARTESIAN_POINT('Ctrl Pts',(-0.508610567848914,1.14335744969678,
-9.19512167880244));
#34652=CARTESIAN_POINT('Ctrl Pts',(-0.454323897972156,1.16599338879742,
-9.19861193166071));
#34653=CARTESIAN_POINT('Ctrl Pts',(-0.312550422081531,1.21369861571125,
-9.20744880516734));
#34654=CARTESIAN_POINT('Ctrl Pts',(-0.223544763956586,1.2332000923951,-9.21272511069972));
#34655=CARTESIAN_POINT('Ctrl Pts',(-0.0561715868345206,1.25113840523285,
-9.22224513286719));
#34656=CARTESIAN_POINT('Ctrl Pts',(0.021464382452435,1.25221492718816,-9.22651245554135));
#34657=CARTESIAN_POINT('Ctrl Pts',(0.159269818008017,1.24129960385597,-9.23419087281889));
#34658=CARTESIAN_POINT('Ctrl Pts',(0.219400811913379,1.23209357394894,-9.23758920462251));
#34659=CARTESIAN_POINT('Ctrl Pts',(0.326356131212141,1.20763766369272,-9.24395278280466));
#34660=CARTESIAN_POINT('Ctrl Pts',(0.373400299605481,1.19393006249441,-9.24684707489846));
#34661=CARTESIAN_POINT('Ctrl Pts',(0.521186162664686,1.1412771440385,-9.25612626363962));
#34662=CARTESIAN_POINT('Ctrl Pts',(0.617746000260806,1.09203603236742,-9.26243472457194));
#34663=CARTESIAN_POINT('Ctrl Pts',(0.771479412321522,0.986647072753507,
-9.27297496860113));
#34664=CARTESIAN_POINT('Ctrl Pts',(0.831858888671005,0.936303404942699,
-9.27729432363076));
#34665=CARTESIAN_POINT('Ctrl Pts',(0.92989420575625,0.837545636596112,-9.28503045659138));
#34666=CARTESIAN_POINT('Ctrl Pts',(0.969465204010896,0.791405612439474,
-9.28843293504891));
#34667=CARTESIAN_POINT('Ctrl Pts',(1.03482248474956,0.702903866462278,-9.29482777606118));
#34668=CARTESIAN_POINT('Ctrl Pts',(1.06174150119686,0.66154072979425,-9.29774880070318));
#34669=CARTESIAN_POINT('Ctrl Pts',(1.13749105883596,0.528559544995029,-9.30681538083952));
#34670=CARTESIAN_POINT('Ctrl Pts',(1.17742084251681,0.432371587683507,-9.3128900576519));
#34671=CARTESIAN_POINT('Ctrl Pts',(1.22453557398548,0.261547640566241,-9.32292858043613));
#34672=CARTESIAN_POINT('Ctrl Pts',(1.23778581263021,0.189159618845307,-9.32698346808543));
#34673=CARTESIAN_POINT('Ctrl Pts',(1.24816957810944,0.077773154565253,-9.33318083186472));
#34674=CARTESIAN_POINT('Ctrl Pts',(1.2499700776908,0.0393777287403109,-9.33531181110441));
#34675=CARTESIAN_POINT('Ctrl Pts',(1.25004417904819,-0.0569489147089241,
-9.34073521958816));
#34676=CARTESIAN_POINT('Ctrl Pts',(1.2460644211611,-0.114784823015238,-9.34409354123995));
#34677=CARTESIAN_POINT('Ctrl Pts',(1.22830219349293,-0.242544049892459,
-9.3516843718206));
#34678=CARTESIAN_POINT('Ctrl Pts',(1.21252321367746,-0.311996505960803,
-9.35590110221895));
#34679=CARTESIAN_POINT('Ctrl Pts',(1.1909259399931,-0.379730701223331,-9.360050506339));
#34680=CARTESIAN_POINT('',(1.188547950716,-0.3871095049826,-8.910050506339));
#34681=CARTESIAN_POINT('Ctrl Pts',(-0.9517960794344,0.08450243785415,-7.598835283632));
#34682=CARTESIAN_POINT('Ctrl Pts',(-0.9318560570757,0.3090975570804,-7.615735374824));
#34683=CARTESIAN_POINT('Ctrl Pts',(-0.7263408395568,0.7424211378759,-7.649535557208));
#34684=CARTESIAN_POINT('Ctrl Pts',(-0.06894632644086,1.036484977236,-7.700235830784));
#34685=CARTESIAN_POINT('Ctrl Pts',(0.6215603569723,0.832233457129,-7.75093610436));
#34686=CARTESIAN_POINT('Ctrl Pts',(1.013379111199,0.2281099298227,-7.801636377936));
#34687=CARTESIAN_POINT('Ctrl Pts',(0.9182129530189,-0.4856491429445,-7.852336651512));
#34688=CARTESIAN_POINT('Ctrl Pts',(0.3817962122075,-0.9660231513296,-7.903036925088));
#34689=CARTESIAN_POINT('Ctrl Pts',(-0.3380943571131,-0.9821719785036,-7.953737198664));
#34690=CARTESIAN_POINT('Ctrl Pts',(-0.8955122787772,-0.5263337477631,-8.00443747224));
#34691=CARTESIAN_POINT('Ctrl Pts',(-1.022588136825,0.1824362236354,-8.055137745816));
#34692=CARTESIAN_POINT('Ctrl Pts',(-0.6582551008476,0.8035357477226,-8.105838019392));
#34693=CARTESIAN_POINT('Ctrl Pts',(0.02240510300165,1.038492891054,-8.156538292968));
#34694=CARTESIAN_POINT('Ctrl Pts',(0.6922984435386,0.7743980496026,-8.207238566544));
#34695=CARTESIAN_POINT('Ctrl Pts',(1.029504948709,0.1381630724743,-8.25793884012));
#34696=CARTESIAN_POINT('Ctrl Pts',(0.8719786597657,-0.5644667314643,-8.308639113696));
#34697=CARTESIAN_POINT('Ctrl Pts',(0.2954194761216,-0.9958397497356,-8.359339387272));
#34698=CARTESIAN_POINT('Ctrl Pts',(-0.4231047393978,-0.9486579222881,-8.410039660848));
#34699=CARTESIAN_POINT('Ctrl Pts',(-0.9383042499798,-0.4455946683874,-8.460739934424));
#34700=CARTESIAN_POINT('Ctrl Pts',(-1.002597833476,0.2716009173896,-8.511440208));
#34701=CARTESIAN_POINT('Ctrl Pts',(-0.58508894663,0.8582775766289,-8.562140481576));
#34702=CARTESIAN_POINT('Ctrl Pts',(0.1135868154433,1.032505452534,-8.612840755152));
#34703=CARTESIAN_POINT('Ctrl Pts',(0.7576779706553,0.7105586296663,-8.663541028728));
#34704=CARTESIAN_POINT('Ctrl Pts',(1.037663893743,0.04714996588551,-8.714241302304));
#34705=CARTESIAN_POINT('Ctrl Pts',(0.8189962043018,-0.6389168103985,-8.76494157588));
#34706=CARTESIAN_POINT('Ctrl Pts',(0.2067565703236,-1.017949495851,-8.815641849456));
#34707=CARTESIAN_POINT('Ctrl Pts',(-0.5048408330584,-0.9078024691232,-8.866342123032));
#34708=CARTESIAN_POINT('Ctrl Pts',(-0.9738347030632,-0.3614070387674,-8.917042396608));
#34709=CARTESIAN_POINT('Ctrl Pts',(-0.9748491478262,0.3586631513228,-8.967742670184));
#34710=CARTESIAN_POINT('Ctrl Pts',(-0.50739285913,0.9063795284549,-9.01844294376));
#34711=CARTESIAN_POINT('Ctrl Pts',(0.2038819114907,1.018519499416,-9.069143217336));
#34712=CARTESIAN_POINT('Ctrl Pts',(0.8172222809373,0.6412506900624,-9.119843490912));
#34713=CARTESIAN_POINT('Ctrl Pts',(1.037686853011,-0.04434136061689,-9.170543764488));
#34714=CARTESIAN_POINT('Ctrl Pts',(0.8526090282577,-0.4867800898099,-9.204343946872));
#34715=CARTESIAN_POINT('Ctrl Pts',(0.6988314801645,-0.6516832061369,-9.221244038064));
#34716=CARTESIAN_POINT('Ctrl Pts',(-1.054366052901,0.09360881367962,-7.65828701626));
#34717=CARTESIAN_POINT('Ctrl Pts',(-1.032277200968,0.3424073478153,-7.675187107452));
#34718=CARTESIAN_POINT('Ctrl Pts',(-0.8046147075109,0.8224278935856,-7.708987289836));
#34719=CARTESIAN_POINT('Ctrl Pts',(-0.07637630333028,1.148181420319,-7.759687563412));
#34720=CARTESIAN_POINT('Ctrl Pts',(0.6885425926632,0.9219188061864,-7.810387836988));
#34721=CARTESIAN_POINT('Ctrl Pts',(1.122585558665,0.2526921170736,-7.861088110564));
#34722=CARTESIAN_POINT('Ctrl Pts',(1.017163852547,-0.5379849539255,-7.91178838414));
#34723=CARTESIAN_POINT('Ctrl Pts',(0.4229403482276,-1.070126300251,-7.962488657716));
#34724=CARTESIAN_POINT('Ctrl Pts',(-0.3745289779184,-1.088015400168,-8.013188931292));
#34725=CARTESIAN_POINT('Ctrl Pts',(-0.9920168480411,-0.5830539210323,-8.063889204868));
#34726=CARTESIAN_POINT('Ctrl Pts',(-1.132786991735,0.2020963998243,-8.114589478445));
#34727=CARTESIAN_POINT('Ctrl Pts',(-0.7291917328499,0.8901284981069,-8.165289752021));
#34728=CARTESIAN_POINT('Ctrl Pts',(0.02481958113415,1.150405716271,-8.215990025596));
#34729=CARTESIAN_POINT('Ctrl Pts',(0.7669037445257,0.857850786083,-8.266690299173));
#34730=CARTESIAN_POINT('Ctrl Pts',(1.140449191446,0.1530521679265,-8.317390572749));
#34731=CARTESIAN_POINT('Ctrl Pts',(0.9659471367619,-0.6252962924595,-8.368090846325));
#34732=CARTESIAN_POINT('Ctrl Pts',(0.3272552532192,-1.103156074014,-8.418791119901));
#34733=CARTESIAN_POINT('Ctrl Pts',(-0.4687004744835,-1.050889713341,-8.469491393477));
#34734=CARTESIAN_POINT('Ctrl Pts',(-1.039420281137,-0.4936140228487,-8.520191667053));
#34735=CARTESIAN_POINT('Ctrl Pts',(-1.110642440297,0.3008698957896,-8.570891940629));
#34736=CARTESIAN_POINT('Ctrl Pts',(-0.6481408534701,0.9507695611661,-8.621592214205));
#34737=CARTESIAN_POINT('Ctrl Pts',(0.1258274591041,1.143773043521,-8.672292487781));
#34738=CARTESIAN_POINT('Ctrl Pts',(0.8393288736432,0.7871317332605,-8.722992761357));
#34739=CARTESIAN_POINT('Ctrl Pts',(1.149487382353,0.05223106556044,-8.773693034933));
#34740=CARTESIAN_POINT('Ctrl Pts',(0.9072550454121,-0.7077694582564,-8.824393308509));
#34741=CARTESIAN_POINT('Ctrl Pts',(0.2290376202147,-1.127648469229,-8.875093582085));
#34742=CARTESIAN_POINT('Ctrl Pts',(-0.5592448298497,-1.005631486475,-8.925793855661));
#34743=CARTESIAN_POINT('Ctrl Pts',(-1.07877966114,-0.4003539426031,-8.976494129237));
#34744=CARTESIAN_POINT('Ctrl Pts',(-1.07990342719,0.3973143610824,-9.027194402813));
#34745=CARTESIAN_POINT('Ctrl Pts',(-0.5620718741233,1.004055203101,-9.077894676389));
#34746=CARTESIAN_POINT('Ctrl Pts',(0.2258531747725,1.128279899031,-9.128594949965));
#34747=CARTESIAN_POINT('Ctrl Pts',(0.9052899558132,0.7103548476505,-9.179295223541));
#34748=CARTESIAN_POINT('Ctrl Pts',(1.149512815819,-0.04911979192188,-9.229995497117));
#34749=CARTESIAN_POINT('Ctrl Pts',(0.9444901436511,-0.5392377768865,-9.263795679501));
#34750=CARTESIAN_POINT('Ctrl Pts',(0.7741408115714,-0.7219116201914,-9.280695770693));
#34751=CARTESIAN_POINT('Ctrl Pts',(-1.156936026367,0.1027151895051,-7.717738748889));
#34752=CARTESIAN_POINT('Ctrl Pts',(-1.13269834486,0.3757171385502,-7.734638840081));
#34753=CARTESIAN_POINT('Ctrl Pts',(-0.882888575465,0.9024346492954,-7.768439022465));
#34754=CARTESIAN_POINT('Ctrl Pts',(-0.0838062802197,1.259877863402,-7.819139296041));
#34755=CARTESIAN_POINT('Ctrl Pts',(0.7555248283541,1.011604155244,-7.869839569617));
#34756=CARTESIAN_POINT('Ctrl Pts',(1.231792006131,0.2772743043245,-7.920539843193));
#34757=CARTESIAN_POINT('Ctrl Pts',(1.116114752076,-0.5903207649065,-7.971240116769));
#34758=CARTESIAN_POINT('Ctrl Pts',(0.4640844842477,-1.174229449172,-8.021940390345));
#34759=CARTESIAN_POINT('Ctrl Pts',(-0.4109635987238,-1.193858821833,-8.072640663921));
#34760=CARTESIAN_POINT('Ctrl Pts',(-1.088521417305,-0.6397740943015,-8.123340937497));
#34761=CARTESIAN_POINT('Ctrl Pts',(-1.242985846645,0.2217565760132,-8.174041211073));
#34762=CARTESIAN_POINT('Ctrl Pts',(-0.8001283648521,0.9767212484911,-8.224741484649));
#34763=CARTESIAN_POINT('Ctrl Pts',(0.02723405926664,1.262318541488,-8.275441758225));
#34764=CARTESIAN_POINT('Ctrl Pts',(0.8415090455128,0.9413035225634,-8.326142031801));
#34765=CARTESIAN_POINT('Ctrl Pts',(1.251393434183,0.1679412633786,-8.376842305377));
#34766=CARTESIAN_POINT('Ctrl Pts',(1.059915613758,-0.6861258534547,-8.427542578953));
#34767=CARTESIAN_POINT('Ctrl Pts',(0.3590910303168,-1.210472398292,-8.478242852529));
#34768=CARTESIAN_POINT('Ctrl Pts',(-0.5142962095692,-1.153121504394,-8.528943126105));
#34769=CARTESIAN_POINT('Ctrl Pts',(-1.140536312295,-0.54163337731,-8.579643399681));
#34770=CARTESIAN_POINT('Ctrl Pts',(-1.218687047119,0.3301388741895,-8.630343673257));
#34771=CARTESIAN_POINT('Ctrl Pts',(-0.7111927603103,1.043261545703,-8.681043946833));
#34772=CARTESIAN_POINT('Ctrl Pts',(0.1380681027649,1.255040634509,-8.731744220409));
#34773=CARTESIAN_POINT('Ctrl Pts',(0.9209797766311,0.8637048368548,-8.782444493985));
#34774=CARTESIAN_POINT('Ctrl Pts',(1.261310870964,0.05731216523537,-8.833144767561));
#34775=CARTESIAN_POINT('Ctrl Pts',(0.9955138865225,-0.7766221061142,-8.883845041137));
#34776=CARTESIAN_POINT('Ctrl Pts',(0.2513186701059,-1.237347442608,-8.934545314713));
#34777=CARTESIAN_POINT('Ctrl Pts',(-0.613648826641,-1.103460503827,-8.985245588289));
#34778=CARTESIAN_POINT('Ctrl Pts',(-1.183724619217,-0.4393008464387,-9.035945861865));
#34779=CARTESIAN_POINT('Ctrl Pts',(-1.184957706554,0.4359655708419,-9.086646135441));
#34780=CARTESIAN_POINT('Ctrl Pts',(-0.6167508891167,1.101730877747,-9.137346409017));
#34781=CARTESIAN_POINT('Ctrl Pts',(0.2478244380543,1.238040298645,-9.188046682593));
#34782=CARTESIAN_POINT('Ctrl Pts',(0.9933576306892,0.7794590052386,-9.238746956169));
#34783=CARTESIAN_POINT('Ctrl Pts',(1.261338778627,-0.05389822322687,-9.289447229745));
#34784=CARTESIAN_POINT('Ctrl Pts',(1.036371259045,-0.5916954639631,-9.323247412129));
#34785=CARTESIAN_POINT('Ctrl Pts',(0.8494501429783,-0.7921400342458,-9.340147503321));
#34786=CARTESIAN_POINT('Ctrl Pts',(-1.259505999833,0.1118215653306,-7.777190481517));
#34787=CARTESIAN_POINT('Ctrl Pts',(-1.233119488752,0.4090269292851,-7.794090572709));
#34788=CARTESIAN_POINT('Ctrl Pts',(-0.9611624434191,0.9824414050051,-7.827890755093));
#34789=CARTESIAN_POINT('Ctrl Pts',(-0.09123625710912,1.371574306486,-7.878591028669));
#34790=CARTESIAN_POINT('Ctrl Pts',(0.8225070640451,1.101289504301,-7.929291302245));
#34791=CARTESIAN_POINT('Ctrl Pts',(1.340998453597,0.3018564915754,-7.979991575821));
#34792=CARTESIAN_POINT('Ctrl Pts',(1.215065651604,-0.6426565758875,-8.030691849397));
#34793=CARTESIAN_POINT('Ctrl Pts',(0.5052286202678,-1.278332598092,-8.081392122973));
#34794=CARTESIAN_POINT('Ctrl Pts',(-0.4473982195291,-1.299702243498,-8.132092396549));
#34795=CARTESIAN_POINT('Ctrl Pts',(-1.185025986569,-0.6964942675707,-8.182792670125));
#34796=CARTESIAN_POINT('Ctrl Pts',(-1.353184701554,0.2414167522021,-8.233492943701));
#34797=CARTESIAN_POINT('Ctrl Pts',(-0.8710649968543,1.063313998875,-8.284193217277));
#34798=CARTESIAN_POINT('Ctrl Pts',(0.02964853739914,1.374231366706,-8.334893490853));
#34799=CARTESIAN_POINT('Ctrl Pts',(0.9161143464999,1.024756259044,-8.385593764429));
#34800=CARTESIAN_POINT('Ctrl Pts',(1.362337676919,0.1828303588308,-8.436294038005));
#34801=CARTESIAN_POINT('Ctrl Pts',(1.153884090754,-0.7469554144499,-8.486994311581));
#34802=CARTESIAN_POINT('Ctrl Pts',(0.3909268074144,-1.31778872257,-8.537694585157));
#34803=CARTESIAN_POINT('Ctrl Pts',(-0.5598919446549,-1.255353295447,-8.588394858733));
#34804=CARTESIAN_POINT('Ctrl Pts',(-1.241652343453,-0.5896527317712,-8.639095132309));
#34805=CARTESIAN_POINT('Ctrl Pts',(-1.326731653941,0.3594078525894,-8.689795405885));
#34806=CARTESIAN_POINT('Ctrl Pts',(-0.7742446671504,1.13575353024,-8.740495679461));
#34807=CARTESIAN_POINT('Ctrl Pts',(0.1503087464258,1.366308225497,-8.791195953037));
#34808=CARTESIAN_POINT('Ctrl Pts',(1.002630679619,0.940277940449,-8.841896226613));
#34809=CARTESIAN_POINT('Ctrl Pts',(1.373134359574,0.0623932649103,-8.892596500189));
#34810=CARTESIAN_POINT('Ctrl Pts',(1.083772727633,-0.8454747539721,-8.943296773765));
#34811=CARTESIAN_POINT('Ctrl Pts',(0.273599719997,-1.347046415986,-8.993997047341));
#34812=CARTESIAN_POINT('Ctrl Pts',(-0.6680528234323,-1.201289521179,-9.044697320917));
#34813=CARTESIAN_POINT('Ctrl Pts',(-1.288669577293,-0.4782477502744,-9.095397594493));
#34814=CARTESIAN_POINT('Ctrl Pts',(-1.290011985917,0.4746167806014,-9.146097868069));
#34815=CARTESIAN_POINT('Ctrl Pts',(-0.67142990411,1.199406552392,-9.196798141645));
#34816=CARTESIAN_POINT('Ctrl Pts',(0.2697957013361,1.347800698259,-9.247498415221));
#34817=CARTESIAN_POINT('Ctrl Pts',(1.081425305565,0.8485631628267,-9.298198688797));
#34818=CARTESIAN_POINT('Ctrl Pts',(1.373164741435,-0.05867665453186,-9.348898962373));
#34819=CARTESIAN_POINT('Ctrl Pts',(1.128252374438,-0.6441531510397,-9.382699144757));
#34820=CARTESIAN_POINT('Ctrl Pts',(0.9247594743852,-0.8623684483003,-9.399599235949));
#34821=CARTESIAN_POINT('',(-1.08160103122666,0.6253104283322,-7.79966651028448));
#34822=CARTESIAN_POINT('Ctrl Pts',(1.18776445373124,-0.386850546630963,
-8.91010660769432));
#34823=CARTESIAN_POINT('Ctrl Pts',(1.21389894012659,-0.306820959780672,
-8.90533140571819));
#34824=CARTESIAN_POINT('Ctrl Pts',(1.23211911862249,-0.224180891334396,
-8.90053865713262));
#34825=CARTESIAN_POINT('Ctrl Pts',(1.25122914691389,-0.0591545543099526,
-8.89095571903426));
#34826=CARTESIAN_POINT('Ctrl Pts',(1.25248415592327,0.0224681132745424,
-8.88617355801157));
#34827=CARTESIAN_POINT('Ctrl Pts',(1.23165538021362,0.264497851938584,-8.87211169336854));
#34828=CARTESIAN_POINT('Ctrl Pts',(1.1863428738656,0.422140450351668,-8.86306238556405));
#34829=CARTESIAN_POINT('Ctrl Pts',(1.04450419562274,0.703018871730047,-8.84517378678212));
#34830=CARTESIAN_POINT('Ctrl Pts',(0.953795594053522,0.822133201515228,
-8.83652591928527));
#34831=CARTESIAN_POINT('Ctrl Pts',(0.780308428421203,0.979376320474896,
-8.82305675175317));
#34832=CARTESIAN_POINT('Ctrl Pts',(0.713162962239612,1.02897046095915,-8.8183374927106));
#34833=CARTESIAN_POINT('Ctrl Pts',(0.525446965343875,1.14122663202712,-8.80593816453637));
#34834=CARTESIAN_POINT('Ctrl Pts',(0.397793799379734,1.19237167907088,-8.79825794581198));
#34835=CARTESIAN_POINT('Ctrl Pts',(0.192918828743436,1.23724963922957,-8.78608919494597));
#34836=CARTESIAN_POINT('Ctrl Pts',(0.119687913895011,1.24636780342359,-8.78177732780935));
#34837=CARTESIAN_POINT('Ctrl Pts',(-0.03729988052084,1.25168049021511,-8.77273368780758));
#34838=CARTESIAN_POINT('Ctrl Pts',(-0.120613512342985,1.24613473199111,
-8.76801130831823));
#34839=CARTESIAN_POINT('Ctrl Pts',(-0.33665447329556,1.21044436773023,-8.75559831193133));
#34840=CARTESIAN_POINT('Ctrl Pts',(-0.467335101319121,1.16686544864178,
-8.74791083973229));
#34841=CARTESIAN_POINT('Ctrl Pts',(-0.65008425343955,1.07001048351806,-8.7359203427984));
#34842=CARTESIAN_POINT('Ctrl Pts',(-0.709377937988781,1.03157766149706,
-8.73178757367245));
#34843=CARTESIAN_POINT('Ctrl Pts',(-0.830858325738161,0.936965587454319,
-8.72290880511093));
#34844=CARTESIAN_POINT('Ctrl Pts',(-0.891244037039048,0.879305104391163,
-8.71818155284362));
#34845=CARTESIAN_POINT('Ctrl Pts',(-1.03546993961214,0.711901864368004,
-8.70565107281324));
#34846=CARTESIAN_POINT('Ctrl Pts',(-1.10864028494722,0.592727437309925,
-8.6978574373626));
#34847=CARTESIAN_POINT('Ctrl Pts',(-1.18512691006641,0.402970729603967,
-8.68600895298831));
#34848=CARTESIAN_POINT('Ctrl Pts',(-1.20481770744938,0.339515965118515,
-8.6821193980736));
#34849=CARTESIAN_POINT('Ctrl Pts',(-1.25429322635665,0.117218312956503,
-8.66895700908858));
#34850=CARTESIAN_POINT('Ctrl Pts',(-1.25838642150074,-0.0469307628035679,
-8.6598986947173));
#34851=CARTESIAN_POINT('Ctrl Pts',(-1.20751589435409,-0.355952994894355,
-8.64207574335479));
#34852=CARTESIAN_POINT('Ctrl Pts',(-1.15759529077901,-0.494611154047977,
-8.63355031817807));
#34853=CARTESIAN_POINT('Ctrl Pts',(-1.04190025748575,-0.694611964138388,
-8.62025658208172));
#34854=CARTESIAN_POINT('Ctrl Pts',(-0.993076972439734,-0.762340311683917,
-8.6155365106255));
#34855=CARTESIAN_POINT('Ctrl Pts',(-0.848865411150693,-0.92616222486434,
-8.60316511958854));
#34856=CARTESIAN_POINT('Ctrl Pts',(-0.743338004112428,-1.01355212264371,
-8.59551429489102));
#34857=CARTESIAN_POINT('Ctrl Pts',(-0.562747984357402,-1.11860166499361,
-8.58339622816306));
#34858=CARTESIAN_POINT('Ctrl Pts',(-0.496143011593621,-1.14959386922681,
-8.57910315151415));
#34859=CARTESIAN_POINT('Ctrl Pts',(-0.348671160649515,-1.20272546073072,
-8.57007625207931));
#34860=CARTESIAN_POINT('Ctrl Pts',(-0.26767690493351,-1.22301508983132,
-8.56535305329552));
#34861=CARTESIAN_POINT('Ctrl Pts',(-0.0507253936393136,-1.25540256524797,
-8.55291722473983));
#34862=CARTESIAN_POINT('Ctrl Pts',(0.0874273983933683,-1.25396265423072,
-8.54520870480266));
#34863=CARTESIAN_POINT('Ctrl Pts',(0.290674642156742,-1.21775450942126,
-8.53324200794464));
#34864=CARTESIAN_POINT('Ctrl Pts',(0.358162640473183,-1.19958054989174,
-8.52915331582327));
#34865=CARTESIAN_POINT('Ctrl Pts',(0.502149049544538,-1.14721725217231,
-8.52031534143725));
#34866=CARTESIAN_POINT('Ctrl Pts',(0.577345283375127,-1.11094026511625,
-8.51558709715192));
#34867=CARTESIAN_POINT('Ctrl Pts',(0.766486872415107,-0.995800335897715,
-8.50302902871571));
#34868=CARTESIAN_POINT('Ctrl Pts',(0.873103246093958,-0.904545584898014,
-8.49521040437098));
#34869=CARTESIAN_POINT('Ctrl Pts',(1.0038874648777,-0.747665133688777,-8.48338487869549));
#34870=CARTESIAN_POINT('Ctrl Pts',(1.04168379062914,-0.694013561883215,
-8.47954245776677));
#34871=CARTESIAN_POINT('Ctrl Pts',(1.15695333587187,-0.49851202972154,-8.4664186607839));
#34872=CARTESIAN_POINT('Ctrl Pts',(1.21147962906974,-0.343598554649147,
-8.45735706141955));
#34873=CARTESIAN_POINT('Ctrl Pts',(1.25980138563557,-0.0247520127629011,
-8.43900920418887));
#34874=CARTESIAN_POINT('Ctrl Pts',(1.25307161001532,0.131747980462025,-8.4299541617984));
#34875=CARTESIAN_POINT('Ctrl Pts',(1.19749640573096,0.365854046723757,-8.41614095741044));
#34876=CARTESIAN_POINT('Ctrl Pts',(1.17023996598552,0.444726326046827,-8.41142976340279));
#34877=CARTESIAN_POINT('Ctrl Pts',(1.08037111576438,0.640759304746671,-8.39920900687085));
#34878=CARTESIAN_POINT('Ctrl Pts',(1.00627911447861,0.752822141300582,-8.39169165367907));
#34879=CARTESIAN_POINT('Ctrl Pts',(0.861460438207615,0.909357876985145,
-8.37930071660415));
#34880=CARTESIAN_POINT('Ctrl Pts',(0.801207019656219,0.962639425462861,
-8.37461729888086));
#34881=CARTESIAN_POINT('Ctrl Pts',(0.668766012044842,1.0585690345103,-8.3652322592572));
#34882=CARTESIAN_POINT('Ctrl Pts',(0.596660491617955,1.10055509444973,-8.36052258402282));
#34883=CARTESIAN_POINT('Ctrl Pts',(0.395567112013034,1.19282720630039,-8.34798466330117));
#34884=CARTESIAN_POINT('Ctrl Pts',(0.244779745730883,1.23744693839987,-8.33921484735322));
#34885=CARTESIAN_POINT('Ctrl Pts',(-0.0942681465773919,1.25790359116205,
-8.31940062305443));
#34886=CARTESIAN_POINT('Ctrl Pts',(-0.252399206177538,1.23164286082107,
-8.31048791289327));
#34887=CARTESIAN_POINT('Ctrl Pts',(-0.467784515236734,1.16126395467836,
-8.29764481620107));
#34888=CARTESIAN_POINT('Ctrl Pts',(-0.544357799543096,1.12769434725901,
-8.2929197281268));
#34889=CARTESIAN_POINT('Ctrl Pts',(-0.749776900489063,1.01188378011857,
-8.27935841353761));
#34890=CARTESIAN_POINT('Ctrl Pts',(-0.86600004791654,0.914361460489527,
-8.27058987911233));
#34891=CARTESIAN_POINT('Ctrl Pts',(-1.06710474253659,0.668642688893352,
-8.25252788742803));
#34892=CARTESIAN_POINT('Ctrl Pts',(-1.14559934894644,0.524176456154759,
-8.24345516230645));
#34893=CARTESIAN_POINT('Ctrl Pts',(-1.21407898851338,0.305145856830464,
-8.2301790680903));
#34894=CARTESIAN_POINT('Ctrl Pts',(-1.22884349703746,0.238818066053841,
-8.22620043878002));
#34895=CARTESIAN_POINT('Ctrl Pts',(-1.25612073580432,0.0381673751078928,
-8.21449039586409));
#34896=CARTESIAN_POINT('Ctrl Pts',(-1.25237495437913,-0.0978504113494669,
-8.20690262720282));
#34897=CARTESIAN_POINT('Ctrl Pts',(-1.21277993941473,-0.310697275105849,
-8.19462470009645));
#34898=CARTESIAN_POINT('Ctrl Pts',(-1.18991780553033,-0.390117925561385,
-8.18994440728262));
#34899=CARTESIAN_POINT('Ctrl Pts',(-1.13233970320381,-0.534318190632865,
-8.18099119971793));
#34900=CARTESIAN_POINT('Ctrl Pts',(-1.09944107541918,-0.599225333096936,
-8.17673410877417));
#34901=CARTESIAN_POINT('Ctrl Pts',(-0.991820469578933,-0.771094829383288,
-8.16498621219696));
#34902=CARTESIAN_POINT('Ctrl Pts',(-0.905499002400952,-0.87005822003041,
-8.15764317860667));
#34903=CARTESIAN_POINT('Ctrl Pts',(-0.743019333840984,-1.0076087936808,
-8.14557711844874));
#34904=CARTESIAN_POINT('Ctrl Pts',(-0.674259098429422,-1.05517283860462,
-8.14085222770922));
#34905=CARTESIAN_POINT('Ctrl Pts',(-0.467693144054769,-1.16935883593837,
-8.12727963908351));
#34906=CARTESIAN_POINT('Ctrl Pts',(-0.323432900325891,-1.21716972897081,
-8.11849635205365));
#34907=CARTESIAN_POINT('Ctrl Pts',(-0.00839329125265246,-1.25925588611344,
-8.1004166149262));
#34908=CARTESIAN_POINT('Ctrl Pts',(0.155770183168729,-1.25015882797825,
-8.09134373978432));
#34909=CARTESIAN_POINT('Ctrl Pts',(0.378090424983517,-1.19337570940643,
-8.07806902379924));
#34910=CARTESIAN_POINT('Ctrl Pts',(0.442257656224971,-1.1711079765006,-8.0740921478462));
#34911=CARTESIAN_POINT('Ctrl Pts',(0.627331812925779,-1.08892563459141,
-8.06238196293534));
#34912=CARTESIAN_POINT('Ctrl Pts',(0.741135647012046,-1.01427047048467,
-8.05479229283736));
#34913=CARTESIAN_POINT('Ctrl Pts',(0.90147328248282,-0.8687435346021,-8.04251237370774));
#34914=CARTESIAN_POINT('Ctrl Pts',(0.957042269146757,-0.807569407056488,
-8.03783206363229));
#34915=CARTESIAN_POINT('Ctrl Pts',(1.04947806804033,-0.682848148974821,
-8.02888040521705));
#34916=CARTESIAN_POINT('Ctrl Pts',(1.08741193471821,-0.620783689543349,
-8.02462500675817));
#34917=CARTESIAN_POINT('Ctrl Pts',(1.17713726084828,-0.43892047919556,-8.0128768113644));
#34918=CARTESIAN_POINT('Ctrl Pts',(1.21601424604425,-0.313444814789549,
-8.00553174425828));
#34919=CARTESIAN_POINT('Ctrl Pts',(1.24770477684024,-0.102893502083894,
-7.99346343954392));
#34920=CARTESIAN_POINT('Ctrl Pts',(1.25205457048966,-0.0193983088591022,
-7.98873843434158));
#34921=CARTESIAN_POINT('Ctrl Pts',(1.24069759299588,0.216343298148389,-7.97516608454395));
#34922=CARTESIAN_POINT('Ctrl Pts',(1.20559856560545,0.364165796579141,-7.96638552286236));
#34923=CARTESIAN_POINT('Ctrl Pts',(1.0759763873466,0.654265009491629,-7.94831191257458));
#34924=CARTESIAN_POINT('Ctrl Pts',(0.982021918408664,0.789167333114058,
-7.93924045402717));
#34925=CARTESIAN_POINT('Ctrl Pts',(0.817143064963047,0.948332669867251,
-7.92598182701509));
#34926=CARTESIAN_POINT('Ctrl Pts',(0.764713742800238,0.991091263345376,
-7.92202024240717));
#34927=CARTESIAN_POINT('Ctrl Pts',(0.597517633845365,1.10562433966725,-7.91029806502895));
#34928=CARTESIAN_POINT('Ctrl Pts',(0.473816334907365,1.16346589742896,-7.90268225435661));
#34929=CARTESIAN_POINT('Ctrl Pts',(0.26536034312891,1.22350762209489,-7.8903783660904));
#34930=CARTESIAN_POINT('Ctrl Pts',(0.184146668761152,1.23863100039534,-7.88569985192011));
#34931=CARTESIAN_POINT('Ctrl Pts',(0.0284444971547855,1.25182002642501,
-7.8766907966508));
#34932=CARTESIAN_POINT('Ctrl Pts',(-0.0453326676439841,1.25137631558713,
-7.87237566436378));
#34933=CARTESIAN_POINT('Ctrl Pts',(-0.247385731590191,1.23159625989491,
-7.86062600752601));
#34934=CARTESIAN_POINT('Ctrl Pts',(-0.373685811337089,1.19876010514595,
-7.85333502383646));
#34935=CARTESIAN_POINT('Ctrl Pts',(-0.613162646726261,1.09626220568374,
-7.83857475953763));
#34936=CARTESIAN_POINT('Ctrl Pts',(-0.726484208237983,1.02564926372048,
-7.83105155416904));
#34937=CARTESIAN_POINT('Ctrl Pts',(-0.942729737103368,0.83543644984202,
-7.81423238529045));
#34938=CARTESIAN_POINT('Ctrl Pts',(-1.02459105923527,0.723752586323567,
-7.80643818382151));
#34939=CARTESIAN_POINT('Ctrl Pts',(-1.08145884712781,0.625207535945593,
-7.79998476760701));
#34940=CARTESIAN_POINT('',(-0.839759385524655,0.485493530587476,-7.63838400393921));
#34941=CARTESIAN_POINT('',(-0.8397594776816,0.485493583525,-7.638384013243));
#34942=CARTESIAN_POINT('',(0.921755949282111,-0.300215476520474,-9.19840833878276));
#34943=CARTESIAN_POINT('Ctrl Pts',(-0.839251282090052,0.485201661780047,
-7.63836822668404));
#34944=CARTESIAN_POINT('Ctrl Pts',(-0.786839191115696,0.57623383833446,
-7.64612438145625));
#34945=CARTESIAN_POINT('Ctrl Pts',(-0.710942044109715,0.675391276285392,
-7.65517867510834));
#34946=CARTESIAN_POINT('Ctrl Pts',(-0.49820857711537,0.841279740454847,
-7.67511813742176));
#34947=CARTESIAN_POINT('Ctrl Pts',(-0.381893017926294,0.899770411614538,
-7.68453883645515));
#34948=CARTESIAN_POINT('Ctrl Pts',(-0.135782197717578,0.968838493154299,
-7.70341336104795));
#34949=CARTESIAN_POINT('Ctrl Pts',(-0.00885791301167451,0.978380920800163,
-7.71264786533363));
#34950=CARTESIAN_POINT('Ctrl Pts',(0.243086422407635,0.946582318646724,
-7.73140195555427));
#34951=CARTESIAN_POINT('Ctrl Pts',(0.364893764354408,0.906795910405157,
-7.74067940423168));
#34952=CARTESIAN_POINT('Ctrl Pts',(0.602552308657543,0.774392065697426,
-7.76078092887998));
#34953=CARTESIAN_POINT('Ctrl Pts',(0.694580298594965,0.685114787931247,
-7.77006362922804));
#34954=CARTESIAN_POINT('Ctrl Pts',(0.837537470686194,0.502943306898377,
-7.78715621316132));
#34955=CARTESIAN_POINT('Ctrl Pts',(0.895666672303433,0.39143709728767,-7.79626984527518));
#34956=CARTESIAN_POINT('Ctrl Pts',(0.973351297906596,0.128895529785619,
-7.81651098819627));
#34957=CARTESIAN_POINT('Ctrl Pts',(0.974893322586702,-0.0019847928045931,
-7.82597019693368));
#34958=CARTESIAN_POINT('Ctrl Pts',(0.950357105839006,-0.225512712002595,
-7.84256438020254));
#34959=CARTESIAN_POINT('Ctrl Pts',(0.915137957151007,-0.343555912182618,
-7.85150366301155));
#34960=CARTESIAN_POINT('Ctrl Pts',(0.79895709032177,-0.565039921665155,
-7.86999754200814));
#34961=CARTESIAN_POINT('Ctrl Pts',(0.715226511460408,-0.666609469197207,
-7.87952665675726));
#34962=CARTESIAN_POINT('Ctrl Pts',(0.536741391990988,-0.813719169033563,
-7.89659574416654));
#34963=CARTESIAN_POINT('Ctrl Pts',(0.430157431758474,-0.881619871693293,
-7.90574434095616));
#34964=CARTESIAN_POINT('Ctrl Pts',(0.169879893219252,-0.963177221783432,
-7.92590779534851));
#34965=CARTESIAN_POINT('Ctrl Pts',(0.0397241532021394,-0.976746905277044,
-7.93537724319687));
#34966=CARTESIAN_POINT('Ctrl Pts',(-0.215567824952798,-0.954110740313475,
-7.95429743954781));
#34967=CARTESIAN_POINT('Ctrl Pts',(-0.335772498328983,-0.919014836607859,
-7.96338078352852));
#34968=CARTESIAN_POINT('Ctrl Pts',(-0.560640566968571,-0.800756976907155,
-7.98215056834433));
#34969=CARTESIAN_POINT('Ctrl Pts',(-0.661335943120196,-0.719769058763693,
-7.99150330602323));
#34970=CARTESIAN_POINT('Ctrl Pts',(-0.844482510173841,-0.502763426800802,
-8.01247835748223));
#34971=CARTESIAN_POINT('Ctrl Pts',(-0.895835357602949,-0.383242232620365,
-8.02187999800142));
#34972=CARTESIAN_POINT('Ctrl Pts',(-0.961546949955464,-0.173650789240346,
-8.03809694137713));
#34973=CARTESIAN_POINT('Ctrl Pts',(-0.976299127968145,-0.0474944798539713,
-8.04729710662085));
#34974=CARTESIAN_POINT('Ctrl Pts',(-0.955530645539919,0.224147261598761,
-8.06743276001601));
#34975=CARTESIAN_POINT('Ctrl Pts',(-0.911883259972712,0.345947006970901,
-8.07679308703859));
#34976=CARTESIAN_POINT('Ctrl Pts',(-0.80759222572764,0.549546991928824,
-8.09367559884552));
#34977=CARTESIAN_POINT('Ctrl Pts',(-0.731634438299219,0.648219317689523,
-8.10270570758665));
#34978=CARTESIAN_POINT('Ctrl Pts',(-0.519253362836709,0.835147785103093,
-8.12362513174581));
#34979=CARTESIAN_POINT('Ctrl Pts',(-0.394382545000837,0.890311605080876,
-8.13346376213966));
#34980=CARTESIAN_POINT('Ctrl Pts',(-0.22948769620124,0.945169712744923,
-8.14628763376929));
#34981=CARTESIAN_POINT('Ctrl Pts',(-0.10344025351597,0.977763677308026,
-8.15567354070393));
#34982=CARTESIAN_POINT('Ctrl Pts',(0.184189748428152,0.960792073154366,
-8.1769774940639));
#34983=CARTESIAN_POINT('Ctrl Pts',(0.311040850131799,0.926823882769418,
-8.18648132694537));
#34984=CARTESIAN_POINT('Ctrl Pts',(0.522317084702463,0.82373430143044,-8.20383254532107));
#34985=CARTESIAN_POINT('Ctrl Pts',(0.627925007800294,0.753621699865986,
-8.21301334868246));
#34986=CARTESIAN_POINT('Ctrl Pts',(0.808291869592365,0.550140906266646,
-8.23310786347754));
#34987=CARTESIAN_POINT('Ctrl Pts',(0.87394342749214,0.437853235013805,-8.2425203987734));
#34988=CARTESIAN_POINT('Ctrl Pts',(0.958431878966911,0.196473510716754,
-8.26140532400548));
#34989=CARTESIAN_POINT('Ctrl Pts',(0.975880231838361,0.0702848706249534,
-8.27064732836836));
#34990=CARTESIAN_POINT('Ctrl Pts',(0.959947904054335,-0.183126801657153,
-8.28939844178708));
#34991=CARTESIAN_POINT('Ctrl Pts',(0.9279613149587,-0.307075814244947,-8.29866694348103));
#34992=CARTESIAN_POINT('Ctrl Pts',(0.810836783038452,-0.552574182082263,
-8.31876610146149));
#34993=CARTESIAN_POINT('Ctrl Pts',(0.727428616466514,-0.650090720524161,
-8.32805586355408));
#34994=CARTESIAN_POINT('Ctrl Pts',(0.554830637668132,-0.804089741468125,
-8.34512936045986));
#34995=CARTESIAN_POINT('Ctrl Pts',(0.447347381110083,-0.869095961842081,
-8.35423363278207));
#34996=CARTESIAN_POINT('Ctrl Pts',(0.190085901191506,-0.963314868905316,
-8.37448821792598));
#34997=CARTESIAN_POINT('Ctrl Pts',(0.0593773685688153,-0.973041258364987,
-8.38395933661561));
#34998=CARTESIAN_POINT('Ctrl Pts',(-0.164812872673331,-0.962733764741733,
-8.40052072541264));
#34999=CARTESIAN_POINT('Ctrl Pts',(-0.284713736492386,-0.935119778603541,
-8.40945016383226));
#35000=CARTESIAN_POINT('Ctrl Pts',(-0.505500848301031,-0.836647957297407,
-8.42732628037607));
#35001=CARTESIAN_POINT('Ctrl Pts',(-0.606159982100895,-0.765891415849571,
-8.43625571879569));
#35002=CARTESIAN_POINT('Ctrl Pts',(-0.763625880418339,-0.605978941163821,
-8.45281710759272));
#35003=CARTESIAN_POINT('Ctrl Pts',(-0.843724779454851,-0.502231702523653,
-8.46228822628236));
#35004=CARTESIAN_POINT('Ctrl Pts',(-0.945519248298759,-0.247872591008094,
-8.48254281142633));
#35005=CARTESIAN_POINT('Ctrl Pts',(-0.968971023406308,-0.124468890204753,
-8.49164708374858));
#35006=CARTESIAN_POINT('Ctrl Pts',(-0.969718982672264,0.106843023223741,
-8.50872058065439));
#35007=CARTESIAN_POINT('Ctrl Pts',(-0.952896543688451,0.23405702822005,
-8.51801034274699));
#35008=CARTESIAN_POINT('Ctrl Pts',(-0.848502485829636,0.485233231854171,
-8.53810950072742));
#35009=CARTESIAN_POINT('Ctrl Pts',(-0.777655722913491,0.591850471490924,
-8.54737800242134));
#35010=CARTESIAN_POINT('Ctrl Pts',(-0.599760572964984,0.773026160649792,
-8.56612911584002));
#35011=CARTESIAN_POINT('Ctrl Pts',(-0.494216597850723,0.844359793833638,
-8.57537112020285));
#35012=CARTESIAN_POINT('Ctrl Pts',(-0.258175251552619,0.94278211128278,
-8.59425604543487));
#35013=CARTESIAN_POINT('Ctrl Pts',(-0.130765826826689,0.968963911470145,
-8.6036685807307));
#35014=CARTESIAN_POINT('Ctrl Pts',(0.141141368764911,0.970728899308695,
-8.62376309552574));
#35015=CARTESIAN_POINT('Ctrl Pts',(0.263869764194383,0.939002707061656,
-8.63294389888712));
#35016=CARTESIAN_POINT('Ctrl Pts',(0.48173765663666,0.850692512192601,-8.6502951172628));
#35017=CARTESIAN_POINT('Ctrl Pts',(0.59176831279852,0.779010613040475,-8.65979895014427));
#35018=CARTESIAN_POINT('Ctrl Pts',(0.796580869189747,0.576351120022339,
-8.68110290350424));
#35019=CARTESIAN_POINT('Ctrl Pts',(0.85655168261402,0.460792364963848,-8.69048881043887));
#35020=CARTESIAN_POINT('Ctrl Pts',(0.925914408979296,0.301454562392536,
-8.7033126820685));
#35021=CARTESIAN_POINT('Ctrl Pts',(0.96830685546231,0.171690743618838,-8.71315131246233));
#35022=CARTESIAN_POINT('Ctrl Pts',(0.97113684240774,-0.111222607635871,
-8.73407073662165));
#35023=CARTESIAN_POINT('Ctrl Pts',(0.948476372601596,-0.233665722796318,
-8.74310084536292));
#35024=CARTESIAN_POINT('Ctrl Pts',(0.866680152751085,-0.447298473368202,
-8.75998335717));
#35025=CARTESIAN_POINT('Ctrl Pts',(0.805223850365118,-0.561155379775387,
-8.76934368419274));
#35026=CARTESIAN_POINT('Ctrl Pts',(0.616996729226077,-0.758109984772489,
-8.78947933758782));
#35027=CARTESIAN_POINT('Ctrl Pts',(0.513278309612569,-0.831427994749491,
-8.79867950283134));
#35028=CARTESIAN_POINT('Ctrl Pts',(0.31343386006222,-0.922580517982861,
-8.81489644620692));
#35029=CARTESIAN_POINT('Ctrl Pts',(0.190196585754656,-0.964233909424807,
-8.82429808672594));
#35030=CARTESIAN_POINT('Ctrl Pts',(-0.0936305289987633,-0.972967651905942,
-8.84527313818489));
#35031=CARTESIAN_POINT('Ctrl Pts',(-0.221167848283893,-0.952162992497406,
-8.8546258758639));
#35032=CARTESIAN_POINT('Ctrl Pts',(-0.459402726619715,-0.863875323940818,
-8.87339566067979));
#35033=CARTESIAN_POINT('Ctrl Pts',(-0.565831472897797,-0.797891932666687,
-8.88247900466054));
#35034=CARTESIAN_POINT('Ctrl Pts',(-0.753251241861668,-0.623077115572175,
-8.90139920101144));
#35035=CARTESIAN_POINT('Ctrl Pts',(-0.830121335358713,-0.517173188849596,
-8.91086864885978));
#35036=CARTESIAN_POINT('Ctrl Pts',(-0.943351358027897,-0.269030164792746,
-8.93103210325212));
#35037=CARTESIAN_POINT('Ctrl Pts',(-0.964048729229666,-0.144361544739941,
-8.94018070004174));
#35038=CARTESIAN_POINT('Ctrl Pts',(-0.973856013903567,0.0867272235402916,
-8.95724978745104));
#35039=CARTESIAN_POINT('Ctrl Pts',(-0.954233524433084,0.216889202356323,
-8.96677890220017));
#35040=CARTESIAN_POINT('Ctrl Pts',(-0.867075844584165,0.451317654377401,
-8.98527278119678));
#35041=CARTESIAN_POINT('Ctrl Pts',(-0.802782957983991,0.556393866127067,
-8.9942120640058));
#35042=CARTESIAN_POINT('Ctrl Pts',(-0.652870452434927,0.724003523585268,
-9.01080624727465));
#35043=CARTESIAN_POINT('Ctrl Pts',(-0.554463941404066,0.81030645092931,
-9.02026545601205));
#35044=CARTESIAN_POINT('Ctrl Pts',(-0.307224094184924,0.927930571195957,
-9.0405065989331));
#35045=CARTESIAN_POINT('Ctrl Pts',(-0.18542229140729,0.959186925789853,
-9.04962023104691));
#35046=CARTESIAN_POINT('Ctrl Pts',(0.0456345727863304,0.974546843206883,
-9.06671281498016));
#35047=CARTESIAN_POINT('Ctrl Pts',(0.173547971727258,0.965729495041201,
-9.07599551532821));
#35048=CARTESIAN_POINT('Ctrl Pts',(0.430853797139275,0.877377505913246,
-9.09609703997657));
#35049=CARTESIAN_POINT('Ctrl Pts',(0.541843176296526,0.813335765249628,
-9.10537448865406));
#35050=CARTESIAN_POINT('Ctrl Pts',(0.733843091802084,0.647133684351997,
-9.12412857887477));
#35051=CARTESIAN_POINT('Ctrl Pts',(0.811550342016078,0.546324878994267,
-9.13336308316049));
#35052=CARTESIAN_POINT('Ctrl Pts',(0.924606730993034,0.317066970465827,
-9.1522376077533));
#35053=CARTESIAN_POINT('Ctrl Pts',(0.958807608424655,0.191445444025974,
-9.16165830678668));
#35054=CARTESIAN_POINT('Ctrl Pts',(0.97752676026398,-0.0776682060790321,
-9.18159750234122));
#35055=CARTESIAN_POINT('Ctrl Pts',(0.954466464728092,-0.200390318016599,
-9.19065177707848));
#35056=CARTESIAN_POINT('Ctrl Pts',(0.921755948798206,-0.300215476427702,
-9.19840833793598));
#35057=CARTESIAN_POINT('Ctrl Pts',(0.921755949557376,-0.300215476483715,
-9.1984083383494));
#35058=CARTESIAN_POINT('Ctrl Pts',(0.966258812022516,-0.314710037724431,
-9.22544687004147));
#35059=CARTESIAN_POINT('Ctrl Pts',(1.01076167448854,-0.329204598962977,
-9.25248540173324));
#35060=CARTESIAN_POINT('Ctrl Pts',(1.09965630787658,-0.358157538981693,
-9.30649496940931));
#35061=CARTESIAN_POINT('Ctrl Pts',(1.14404807879862,-0.372615917761862,
-9.33346600539358));
#35062=CARTESIAN_POINT('Ctrl Pts',(1.18843984972142,-0.387074296539831,
-9.36043704137777));
#35063=CARTESIAN_POINT('Ctrl Pts',(-1.259505999833,0.1118215653306,-7.310493359005));
#35064=CARTESIAN_POINT('Ctrl Pts',(-1.233119488752,0.4090269292851,-7.327393450197));
#35065=CARTESIAN_POINT('Ctrl Pts',(-0.9611624434191,0.9824414050051,-7.361193632581));
#35066=CARTESIAN_POINT('Ctrl Pts',(-0.09123625710912,1.371574306486,-7.411893906157));
#35067=CARTESIAN_POINT('Ctrl Pts',(0.8225070640451,1.101289504301,-7.462594179733));
#35068=CARTESIAN_POINT('Ctrl Pts',(1.340998453597,0.3018564915754,-7.513294453309));
#35069=CARTESIAN_POINT('Ctrl Pts',(1.215065651604,-0.6426565758875,-7.563994726885));
#35070=CARTESIAN_POINT('Ctrl Pts',(0.5052286202678,-1.278332598092,-7.614695000461));
#35071=CARTESIAN_POINT('Ctrl Pts',(-0.4473982195291,-1.299702243498,-7.665395274037));
#35072=CARTESIAN_POINT('Ctrl Pts',(-1.185025986569,-0.6964942675707,-7.716095547613));
#35073=CARTESIAN_POINT('Ctrl Pts',(-1.353184701554,0.2414167522021,-7.766795821189));
#35074=CARTESIAN_POINT('Ctrl Pts',(-0.8710649968543,1.063313998875,-7.817496094765));
#35075=CARTESIAN_POINT('Ctrl Pts',(0.02964853739914,1.374231366706,-7.868196368341));
#35076=CARTESIAN_POINT('Ctrl Pts',(0.9161143464999,1.024756259044,-7.918896641917));
#35077=CARTESIAN_POINT('Ctrl Pts',(1.362337676919,0.1828303588308,-7.969596915493));
#35078=CARTESIAN_POINT('Ctrl Pts',(1.153884090754,-0.7469554144499,-8.020297189069));
#35079=CARTESIAN_POINT('Ctrl Pts',(0.3909268074144,-1.31778872257,-8.070997462645));
#35080=CARTESIAN_POINT('Ctrl Pts',(-0.5598919446549,-1.255353295447,-8.121697736221));
#35081=CARTESIAN_POINT('Ctrl Pts',(-1.241652343453,-0.5896527317712,-8.172398009797));
#35082=CARTESIAN_POINT('Ctrl Pts',(-1.326731653941,0.3594078525894,-8.223098283373));
#35083=CARTESIAN_POINT('Ctrl Pts',(-0.7742446671504,1.13575353024,-8.273798556949));
#35084=CARTESIAN_POINT('Ctrl Pts',(0.1503087464258,1.366308225497,-8.324498830525));
#35085=CARTESIAN_POINT('Ctrl Pts',(1.002630679619,0.940277940449,-8.375199104101));
#35086=CARTESIAN_POINT('Ctrl Pts',(1.373134359574,0.0623932649103,-8.425899377677));
#35087=CARTESIAN_POINT('Ctrl Pts',(1.083772727633,-0.8454747539721,-8.476599651253));
#35088=CARTESIAN_POINT('Ctrl Pts',(0.273599719997,-1.347046415986,-8.527299924829));
#35089=CARTESIAN_POINT('Ctrl Pts',(-0.6680528234323,-1.201289521179,-8.578000198405));
#35090=CARTESIAN_POINT('Ctrl Pts',(-1.288669577293,-0.4782477502744,-8.628700471981));
#35091=CARTESIAN_POINT('Ctrl Pts',(-1.290011985917,0.4746167806014,-8.679400745557));
#35092=CARTESIAN_POINT('Ctrl Pts',(-0.67142990411,1.199406552392,-8.730101019133));
#35093=CARTESIAN_POINT('Ctrl Pts',(0.2697957013361,1.347800698259,-8.780801292709));
#35094=CARTESIAN_POINT('Ctrl Pts',(1.081425305565,0.8485631628267,-8.831501566285));
#35095=CARTESIAN_POINT('Ctrl Pts',(1.373164741435,-0.05867665453186,-8.882201839861));
#35096=CARTESIAN_POINT('Ctrl Pts',(1.128252374438,-0.6441531510397,-8.916002022245));
#35097=CARTESIAN_POINT('Ctrl Pts',(0.9247594743852,-0.8623684483003,-8.932902113437));
#35098=CARTESIAN_POINT('Ctrl Pts',(-1.156936026367,0.1027151895051,-7.369945091634));
#35099=CARTESIAN_POINT('Ctrl Pts',(-1.13269834486,0.3757171385502,-7.386845182826));
#35100=CARTESIAN_POINT('Ctrl Pts',(-0.882888575465,0.9024346492954,-7.42064536521));
#35101=CARTESIAN_POINT('Ctrl Pts',(-0.0838062802197,1.259877863402,-7.471345638786));
#35102=CARTESIAN_POINT('Ctrl Pts',(0.7555248283541,1.011604155244,-7.522045912362));
#35103=CARTESIAN_POINT('Ctrl Pts',(1.231792006131,0.2772743043245,-7.572746185938));
#35104=CARTESIAN_POINT('Ctrl Pts',(1.116114752076,-0.5903207649065,-7.623446459514));
#35105=CARTESIAN_POINT('Ctrl Pts',(0.4640844842477,-1.174229449172,-7.67414673309));
#35106=CARTESIAN_POINT('Ctrl Pts',(-0.4109635987238,-1.193858821833,-7.724847006666));
#35107=CARTESIAN_POINT('Ctrl Pts',(-1.088521417305,-0.6397740943015,-7.775547280242));
#35108=CARTESIAN_POINT('Ctrl Pts',(-1.242985846645,0.2217565760132,-7.826247553818));
#35109=CARTESIAN_POINT('Ctrl Pts',(-0.8001283648521,0.9767212484911,-7.876947827394));
#35110=CARTESIAN_POINT('Ctrl Pts',(0.02723405926664,1.262318541488,-7.92764810097));
#35111=CARTESIAN_POINT('Ctrl Pts',(0.8415090455128,0.9413035225634,-7.978348374546));
#35112=CARTESIAN_POINT('Ctrl Pts',(1.251393434183,0.1679412633786,-8.029048648122));
#35113=CARTESIAN_POINT('Ctrl Pts',(1.059915613758,-0.6861258534547,-8.079748921698));
#35114=CARTESIAN_POINT('Ctrl Pts',(0.3590910303168,-1.210472398292,-8.130449195274));
#35115=CARTESIAN_POINT('Ctrl Pts',(-0.5142962095692,-1.153121504394,-8.18114946885));
#35116=CARTESIAN_POINT('Ctrl Pts',(-1.140536312295,-0.54163337731,-8.231849742426));
#35117=CARTESIAN_POINT('Ctrl Pts',(-1.218687047119,0.3301388741895,-8.282550016002));
#35118=CARTESIAN_POINT('Ctrl Pts',(-0.7111927603103,1.043261545703,-8.333250289578));
#35119=CARTESIAN_POINT('Ctrl Pts',(0.1380681027649,1.255040634509,-8.383950563154));
#35120=CARTESIAN_POINT('Ctrl Pts',(0.9209797766311,0.8637048368548,-8.43465083673));
#35121=CARTESIAN_POINT('Ctrl Pts',(1.261310870964,0.05731216523537,-8.485351110306));
#35122=CARTESIAN_POINT('Ctrl Pts',(0.9955138865225,-0.7766221061142,-8.536051383882));
#35123=CARTESIAN_POINT('Ctrl Pts',(0.2513186701059,-1.237347442608,-8.586751657458));
#35124=CARTESIAN_POINT('Ctrl Pts',(-0.613648826641,-1.103460503827,-8.637451931034));
#35125=CARTESIAN_POINT('Ctrl Pts',(-1.183724619217,-0.4393008464388,-8.68815220461));
#35126=CARTESIAN_POINT('Ctrl Pts',(-1.184957706554,0.4359655708419,-8.738852478186));
#35127=CARTESIAN_POINT('Ctrl Pts',(-0.6167508891167,1.101730877747,-8.789552751762));
#35128=CARTESIAN_POINT('Ctrl Pts',(0.2478244380543,1.238040298645,-8.840253025338));
#35129=CARTESIAN_POINT('Ctrl Pts',(0.9933576306892,0.7794590052386,-8.890953298914));
#35130=CARTESIAN_POINT('Ctrl Pts',(1.261338778627,-0.05389822322687,-8.94165357249));
#35131=CARTESIAN_POINT('Ctrl Pts',(1.036371259045,-0.5916954639631,-8.975453754874));
#35132=CARTESIAN_POINT('Ctrl Pts',(0.8494501429783,-0.7921400342458,-8.992353846066));
#35133=CARTESIAN_POINT('Ctrl Pts',(-1.054366052901,0.09360881367962,-7.429396824262));
#35134=CARTESIAN_POINT('Ctrl Pts',(-1.032277200968,0.3424073478153,-7.446296915454));
#35135=CARTESIAN_POINT('Ctrl Pts',(-0.8046147075109,0.8224278935856,-7.480097097838));
#35136=CARTESIAN_POINT('Ctrl Pts',(-0.07637630333028,1.148181420319,-7.530797371414));
#35137=CARTESIAN_POINT('Ctrl Pts',(0.6885425926632,0.9219188061864,-7.58149764499));
#35138=CARTESIAN_POINT('Ctrl Pts',(1.122585558665,0.2526921170736,-7.632197918566));
#35139=CARTESIAN_POINT('Ctrl Pts',(1.017163852547,-0.5379849539255,-7.682898192142));
#35140=CARTESIAN_POINT('Ctrl Pts',(0.4229403482276,-1.070126300251,-7.733598465718));
#35141=CARTESIAN_POINT('Ctrl Pts',(-0.3745289779184,-1.088015400168,-7.784298739294));
#35142=CARTESIAN_POINT('Ctrl Pts',(-0.9920168480411,-0.5830539210323,-7.83499901287));
#35143=CARTESIAN_POINT('Ctrl Pts',(-1.132786991735,0.2020963998243,-7.885699286446));
#35144=CARTESIAN_POINT('Ctrl Pts',(-0.7291917328499,0.8901284981069,-7.936399560022));
#35145=CARTESIAN_POINT('Ctrl Pts',(0.02481958113415,1.150405716271,-7.987099833598));
#35146=CARTESIAN_POINT('Ctrl Pts',(0.7669037445257,0.857850786083,-8.037800107174));
#35147=CARTESIAN_POINT('Ctrl Pts',(1.140449191446,0.1530521679265,-8.08850038075));
#35148=CARTESIAN_POINT('Ctrl Pts',(0.9659471367619,-0.6252962924595,-8.139200654326));
#35149=CARTESIAN_POINT('Ctrl Pts',(0.3272552532192,-1.103156074014,-8.189900927902));
#35150=CARTESIAN_POINT('Ctrl Pts',(-0.4687004744835,-1.050889713341,-8.240601201478));
#35151=CARTESIAN_POINT('Ctrl Pts',(-1.039420281137,-0.4936140228487,-8.291301475054));
#35152=CARTESIAN_POINT('Ctrl Pts',(-1.110642440297,0.3008698957896,-8.34200174863));
#35153=CARTESIAN_POINT('Ctrl Pts',(-0.6481408534701,0.9507695611661,-8.392702022206));
#35154=CARTESIAN_POINT('Ctrl Pts',(0.1258274591041,1.143773043521,-8.443402295782));
#35155=CARTESIAN_POINT('Ctrl Pts',(0.8393288736432,0.7871317332605,-8.494102569358));
#35156=CARTESIAN_POINT('Ctrl Pts',(1.149487382353,0.05223106556044,-8.544802842934));
#35157=CARTESIAN_POINT('Ctrl Pts',(0.9072550454121,-0.7077694582564,-8.59550311651));
#35158=CARTESIAN_POINT('Ctrl Pts',(0.2290376202147,-1.127648469229,-8.646203390086));
#35159=CARTESIAN_POINT('Ctrl Pts',(-0.5592448298497,-1.005631486475,-8.696903663662));
#35160=CARTESIAN_POINT('Ctrl Pts',(-1.07877966114,-0.4003539426031,-8.747603937238));
#35161=CARTESIAN_POINT('Ctrl Pts',(-1.07990342719,0.3973143610824,-8.798304210814));
#35162=CARTESIAN_POINT('Ctrl Pts',(-0.5620718741233,1.004055203101,-8.84900448439));
#35163=CARTESIAN_POINT('Ctrl Pts',(0.2258531747725,1.128279899031,-8.899704757966));
#35164=CARTESIAN_POINT('Ctrl Pts',(0.9052899558132,0.7103548476505,-8.950405031542));
#35165=CARTESIAN_POINT('Ctrl Pts',(1.149512815819,-0.04911979192188,-9.001105305118));
#35166=CARTESIAN_POINT('Ctrl Pts',(0.9444901436511,-0.5392377768865,-9.034905487502));
#35167=CARTESIAN_POINT('Ctrl Pts',(0.7741408115714,-0.7219116201914,-9.051805578694));
#35168=CARTESIAN_POINT('Ctrl Pts',(-0.9517960794344,0.08450243785415,-7.48884855689));
#35169=CARTESIAN_POINT('Ctrl Pts',(-0.9318560570757,0.3090975570804,-7.505748648082));
#35170=CARTESIAN_POINT('Ctrl Pts',(-0.7263408395568,0.7424211378759,-7.539548830466));
#35171=CARTESIAN_POINT('Ctrl Pts',(-0.06894632644086,1.036484977236,-7.590249104042));
#35172=CARTESIAN_POINT('Ctrl Pts',(0.6215603569723,0.832233457129,-7.640949377618));
#35173=CARTESIAN_POINT('Ctrl Pts',(1.013379111199,0.2281099298227,-7.691649651194));
#35174=CARTESIAN_POINT('Ctrl Pts',(0.9182129530188,-0.4856491429445,-7.74234992477));
#35175=CARTESIAN_POINT('Ctrl Pts',(0.3817962122075,-0.9660231513296,-7.793050198346));
#35176=CARTESIAN_POINT('Ctrl Pts',(-0.3380943571131,-0.9821719785035,-7.843750471922));
#35177=CARTESIAN_POINT('Ctrl Pts',(-0.8955122787772,-0.5263337477631,-7.894450745498));
#35178=CARTESIAN_POINT('Ctrl Pts',(-1.022588136825,0.1824362236354,-7.945151019074));
#35179=CARTESIAN_POINT('Ctrl Pts',(-0.6582551008476,0.8035357477226,-7.99585129265));
#35180=CARTESIAN_POINT('Ctrl Pts',(0.02240510300165,1.038492891054,-8.046551566226));
#35181=CARTESIAN_POINT('Ctrl Pts',(0.6922984435386,0.7743980496026,-8.097251839802));
#35182=CARTESIAN_POINT('Ctrl Pts',(1.029504948709,0.1381630724743,-8.147952113378));
#35183=CARTESIAN_POINT('Ctrl Pts',(0.8719786597657,-0.5644667314643,-8.198652386954));
#35184=CARTESIAN_POINT('Ctrl Pts',(0.2954194761216,-0.9958397497356,-8.24935266053));
#35185=CARTESIAN_POINT('Ctrl Pts',(-0.4231047393978,-0.948657922288,-8.300052934106));
#35186=CARTESIAN_POINT('Ctrl Pts',(-0.9383042499798,-0.4455946683874,-8.350753207682));
#35187=CARTESIAN_POINT('Ctrl Pts',(-1.002597833476,0.2716009173896,-8.401453481258));
#35188=CARTESIAN_POINT('Ctrl Pts',(-0.58508894663,0.8582775766289,-8.452153754834));
#35189=CARTESIAN_POINT('Ctrl Pts',(0.1135868154433,1.032505452534,-8.50285402841));
#35190=CARTESIAN_POINT('Ctrl Pts',(0.7576779706553,0.7105586296663,-8.553554301986));
#35191=CARTESIAN_POINT('Ctrl Pts',(1.037663893743,0.04714996588551,-8.604254575562));
#35192=CARTESIAN_POINT('Ctrl Pts',(0.8189962043018,-0.6389168103985,-8.654954849138));
#35193=CARTESIAN_POINT('Ctrl Pts',(0.2067565703236,-1.017949495851,-8.705655122714));
#35194=CARTESIAN_POINT('Ctrl Pts',(-0.5048408330584,-0.9078024691232,-8.75635539629));
#35195=CARTESIAN_POINT('Ctrl Pts',(-0.9738347030632,-0.3614070387674,-8.807055669866));
#35196=CARTESIAN_POINT('Ctrl Pts',(-0.9748491478262,0.3586631513228,-8.857755943442));
#35197=CARTESIAN_POINT('Ctrl Pts',(-0.50739285913,0.9063795284549,-8.908456217018));
#35198=CARTESIAN_POINT('Ctrl Pts',(0.2038819114907,1.018519499416,-8.959156490594));
#35199=CARTESIAN_POINT('Ctrl Pts',(0.8172222809373,0.6412506900624,-9.00985676417));
#35200=CARTESIAN_POINT('Ctrl Pts',(1.037686853011,-0.04434136061689,-9.060557037746));
#35201=CARTESIAN_POINT('Ctrl Pts',(0.8526090282577,-0.4867800898099,-9.09435722013));
#35202=CARTESIAN_POINT('Ctrl Pts',(0.6988314801645,-0.6516832061369,-9.111257311322));
#35203=CARTESIAN_POINT('',(-1.08160102925865,0.625310431755989,-7.35041766696342));
#35204=CARTESIAN_POINT('Ctrl Pts',(-1.08141633891441,0.625226119210898,
-7.35008360873745));
#35205=CARTESIAN_POINT('Ctrl Pts',(-1.03390357444464,0.707597454903937,
-7.35557558080133));
#35206=CARTESIAN_POINT('Ctrl Pts',(-0.977165735444024,0.784700022705665,
-7.36105287658457));
#35207=CARTESIAN_POINT('Ctrl Pts',(-0.847428073212402,0.923895031085402,
-7.37187595599759));
#35208=CARTESIAN_POINT('Ctrl Pts',(-0.775218330200545,0.985002391821968,
-7.37715175724076));
#35209=CARTESIAN_POINT('Ctrl Pts',(-0.562372240877458,1.12689746391015,
-7.39180025301249));
#35210=CARTESIAN_POINT('Ctrl Pts',(-0.41080462578532,1.19043897709064,-7.40119985709024));
#35211=CARTESIAN_POINT('Ctrl Pts',(-0.0629664710684568,1.26354084983809,
-7.42162303400616));
#35212=CARTESIAN_POINT('Ctrl Pts',(0.103488374627705,1.25272346457742,-7.43077732184325));
#35213=CARTESIAN_POINT('Ctrl Pts',(0.393137413675227,1.19617600750093,-7.44776934087969));
#35214=CARTESIAN_POINT('Ctrl Pts',(0.544669237975361,1.13566521348015,-7.45708958155269));
#35215=CARTESIAN_POINT('Ctrl Pts',(0.74071771238418,1.00950579684395,-7.47039494437775));
#35216=CARTESIAN_POINT('Ctrl Pts',(0.798229981102956,0.964762914809237,
-7.4744740161231));
#35217=CARTESIAN_POINT('Ctrl Pts',(0.91161970049166,0.858715269389297,-7.48330419809846));
#35218=CARTESIAN_POINT('Ctrl Pts',(0.96585170887338,0.796699343698819,-7.48801878934439));
#35219=CARTESIAN_POINT('Ctrl Pts',(1.1051564507755,0.602515358859405,-7.50180807576398));
#35220=CARTESIAN_POINT('Ctrl Pts',(1.17325445808129,0.457773604427091,-7.51093744662193));
#35221=CARTESIAN_POINT('Ctrl Pts',(1.23173628114455,0.227803586493787,-7.52442350173589));
#35222=CARTESIAN_POINT('Ctrl Pts',(1.24360254337297,0.148809050123005,-7.52889719445281));
#35223=CARTESIAN_POINT('Ctrl Pts',(1.25210926732186,-0.0141296717769907,
-7.53823147511025));
#35224=CARTESIAN_POINT('Ctrl Pts',(1.24810293985508,-0.0976312140262272,
-7.54303303614898));
#35225=CARTESIAN_POINT('Ctrl Pts',(1.21512425843464,-0.32325358963531,-7.55620697967317));
#35226=CARTESIAN_POINT('Ctrl Pts',(1.16817801989322,-0.475178802142458,
-7.56524490596786));
#35227=CARTESIAN_POINT('Ctrl Pts',(1.0010569163738,-0.767448246501332,-7.5842773720152));
#35228=CARTESIAN_POINT('Ctrl Pts',(0.893699212068381,-0.883883124181553,
-7.59326625011072));
#35229=CARTESIAN_POINT('Ctrl Pts',(0.719401219493123,-1.02453980494428,
-7.60620759270894));
#35230=CARTESIAN_POINT('Ctrl Pts',(0.649553479442821,-1.07048344305116,
-7.6110122144122));
#35231=CARTESIAN_POINT('Ctrl Pts',(0.43533477113506,-1.18255361353768,-7.62485720834406));
#35232=CARTESIAN_POINT('Ctrl Pts',(0.284651569813539,-1.22753999642643,
-7.63351977150539));
#35233=CARTESIAN_POINT('Ctrl Pts',(-0.0378877950936454,-1.25878616455311,
-7.65219720012196));
#35234=CARTESIAN_POINT('Ctrl Pts',(-0.202527294014996,-1.24354442983782,
-7.66163547117351));
#35235=CARTESIAN_POINT('Ctrl Pts',(-0.432645253811083,-1.17535719485944,
-7.67529850407763));
#35236=CARTESIAN_POINT('Ctrl Pts',(-0.5044565720885,-1.14630075345231,-7.67963067502684));
#35237=CARTESIAN_POINT('Ctrl Pts',(-0.715088231070164,-1.03676845987327,
-7.69318388762178));
#35238=CARTESIAN_POINT('Ctrl Pts',(-0.842583200977805,-0.935593103413969,
-7.7024820512621));
#35239=CARTESIAN_POINT('Ctrl Pts',(-1.05492365451986,-0.690166554091875,
-7.72116588890207));
#35240=CARTESIAN_POINT('Ctrl Pts',(-1.13607731155066,-0.547058816969546,
-7.73020867810678));
#35241=CARTESIAN_POINT('Ctrl Pts',(-1.23686100235198,-0.236561521351647,
-7.74896782912686));
#35242=CARTESIAN_POINT('Ctrl Pts',(-1.25722144982577,-0.0738463772980785,
-7.75834693922323));
#35243=CARTESIAN_POINT('Ctrl Pts',(-1.24034494211375,0.18082038036121,-7.77296132059527));
#35244=CARTESIAN_POINT('Ctrl Pts',(-1.22343274900602,0.273643041743944,
-7.77822353566137));
#35245=CARTESIAN_POINT('Ctrl Pts',(-1.16761229453482,0.455287656065107,
-7.789032216188));
#35246=CARTESIAN_POINT('Ctrl Pts',(-1.12910782046682,0.542922433132975,
-7.79450905932452));
#35247=CARTESIAN_POINT('Ctrl Pts',(-1.08143574407104,0.625192553810161,
-7.80000057583712));
#35248=CARTESIAN_POINT('',(0.921755949135472,-0.300215476273863,-9.07172448818857));
#35249=CARTESIAN_POINT('Ctrl Pts',(1.18807733836104,-0.386956226761339,
-8.90991603565015));
#35250=CARTESIAN_POINT('Ctrl Pts',(1.14381077010285,-0.372538626432016,
-8.93681100245566));
#35251=CARTESIAN_POINT('Ctrl Pts',(1.09954420184343,-0.358121026106439,
-8.96370596926116));
#35252=CARTESIAN_POINT('Ctrl Pts',(1.01077040547201,-0.329207442646842,
-9.01764212018779));
#35253=CARTESIAN_POINT('Ctrl Pts',(0.96626317735999,-0.314711459512787,
-9.04468330430887));
#35254=CARTESIAN_POINT('Ctrl Pts',(0.921755949246852,-0.300215476382577,
-9.07172448843017));
#35255=CARTESIAN_POINT('',(-0.83975938535873,0.485493530516545,-7.51170016756324));
#35256=CARTESIAN_POINT('Ctrl Pts',(-0.839251224062929,0.485201762564704,
-7.51168438601709));
#35257=CARTESIAN_POINT('Ctrl Pts',(-0.78683913480634,0.576233911347829,
-7.51944053895476));
#35258=CARTESIAN_POINT('Ctrl Pts',(-0.710942002712494,0.675391308566732,
-7.52849482973451));
#35259=CARTESIAN_POINT('Ctrl Pts',(-0.498208577115371,0.841279740454846,
-7.54843428816774));
#35260=CARTESIAN_POINT('Ctrl Pts',(-0.381893017926296,0.899770411614537,
-7.55785498720109));
#35261=CARTESIAN_POINT('Ctrl Pts',(-0.135782197717577,0.968838493154299,
-7.57672951179386));
#35262=CARTESIAN_POINT('Ctrl Pts',(-0.00885791301167244,0.978380920800163,
-7.58596401607956));
#35263=CARTESIAN_POINT('Ctrl Pts',(0.243086422407639,0.946582318646723,
-7.60471810630025));
#35264=CARTESIAN_POINT('Ctrl Pts',(0.364893764354414,0.906795910405155,
-7.61399555497774));
#35265=CARTESIAN_POINT('Ctrl Pts',(0.602552308657548,0.774392065697422,
-7.63409707962608));
#35266=CARTESIAN_POINT('Ctrl Pts',(0.69458029859497,0.685114787931242,-7.64337977997413));
#35267=CARTESIAN_POINT('Ctrl Pts',(0.837537470686198,0.502943306898371,
-7.66047236390738));
#35268=CARTESIAN_POINT('Ctrl Pts',(0.895666672303435,0.391437097287665,
-7.6695859960212));
#35269=CARTESIAN_POINT('Ctrl Pts',(0.973351297906597,0.128895529785616,
-7.68982713894225));
#35270=CARTESIAN_POINT('Ctrl Pts',(0.974893322586701,-0.00198479280459631,
-7.69928634767966));
#35271=CARTESIAN_POINT('Ctrl Pts',(0.950357105839005,-0.225512712002599,
-7.71588053094852));
#35272=CARTESIAN_POINT('Ctrl Pts',(0.915137957151005,-0.343555912182622,
-7.72481981375755));
#35273=CARTESIAN_POINT('Ctrl Pts',(0.798957090321767,-0.56503992166516,
-7.74331369275417));
#35274=CARTESIAN_POINT('Ctrl Pts',(0.715226511460403,-0.666609469197212,
-7.75284280750332));
#35275=CARTESIAN_POINT('Ctrl Pts',(0.536741391990981,-0.813719169033567,
-7.76991189491262));
#35276=CARTESIAN_POINT('Ctrl Pts',(0.430157431758467,-0.881619871693296,
-7.77906049170225));
#35277=CARTESIAN_POINT('Ctrl Pts',(0.169879893219243,-0.963177221783434,
-7.79922394609459));
#35278=CARTESIAN_POINT('Ctrl Pts',(0.0397241532021311,-0.976746905277045,
-7.80869339394293));
#35279=CARTESIAN_POINT('Ctrl Pts',(-0.215567824952813,-0.954110740313473,
-7.82761359029387));
#35280=CARTESIAN_POINT('Ctrl Pts',(-0.335772498328998,-0.919014836607853,
-7.83669693427461));
#35281=CARTESIAN_POINT('Ctrl Pts',(-0.560640566968575,-0.800756976907151,
-7.85546671909044));
#35282=CARTESIAN_POINT('Ctrl Pts',(-0.661335943120198,-0.719769058763691,
-7.86481945676939));
#35283=CARTESIAN_POINT('Ctrl Pts',(-0.844482510173831,-0.502763426800814,
-7.88579450822828));
#35284=CARTESIAN_POINT('Ctrl Pts',(-0.89583535760294,-0.383242232620388,
-7.89519614874726));
#35285=CARTESIAN_POINT('Ctrl Pts',(-0.96154694995546,-0.173650789240365,
-7.91141309212273));
#35286=CARTESIAN_POINT('Ctrl Pts',(-0.976299127968143,-0.0474944798539945,
-7.92061325736621));
#35287=CARTESIAN_POINT('Ctrl Pts',(-0.955530645539925,0.224147261598739,
-7.94074891076125));
#35288=CARTESIAN_POINT('Ctrl Pts',(-0.91188325997272,0.34594700697088,-7.95010923778401));
#35289=CARTESIAN_POINT('Ctrl Pts',(-0.807592225727651,0.54954699192881,
-7.96699174959113));
#35290=CARTESIAN_POINT('Ctrl Pts',(-0.731634438299227,0.648219317689515,
-7.97602185833242));
#35291=CARTESIAN_POINT('Ctrl Pts',(-0.519253362836699,0.835147785103102,
-7.99694128249182));
#35292=CARTESIAN_POINT('Ctrl Pts',(-0.394382545000818,0.890311605080883,
-8.00677991288573));
#35293=CARTESIAN_POINT('Ctrl Pts',(-0.229487696201209,0.945169712744932,
-8.01960378451543));
#35294=CARTESIAN_POINT('Ctrl Pts',(-0.103440253515942,0.977763677308026,
-8.02898969145012));
#35295=CARTESIAN_POINT('Ctrl Pts',(0.184189748428156,0.960792073154365,
-8.0502936448101));
#35296=CARTESIAN_POINT('Ctrl Pts',(0.311040850131801,0.926823882769417,
-8.0597974776915));
#35297=CARTESIAN_POINT('Ctrl Pts',(0.522317084702464,0.82373430143044,-8.07714869606713));
#35298=CARTESIAN_POINT('Ctrl Pts',(0.627925007800295,0.753621699865985,
-8.08632949942849));
#35299=CARTESIAN_POINT('Ctrl Pts',(0.808291869592366,0.550140906266646,
-8.10642401422356));
#35300=CARTESIAN_POINT('Ctrl Pts',(0.87394342749214,0.437853235013805,-8.11583654951944));
#35301=CARTESIAN_POINT('Ctrl Pts',(0.958431878966911,0.196473510716756,
-8.13472147475153));
#35302=CARTESIAN_POINT('Ctrl Pts',(0.975880231838361,0.0702848706249561,
-8.14396347911438));
#35303=CARTESIAN_POINT('Ctrl Pts',(0.959947904054336,-0.183126801657149,
-8.16271459253308));
#35304=CARTESIAN_POINT('Ctrl Pts',(0.927961314958701,-0.307075814244942,
-8.17198309422699));
#35305=CARTESIAN_POINT('Ctrl Pts',(0.810836783038454,-0.55257418208226,
-8.19208225220743));
#35306=CARTESIAN_POINT('Ctrl Pts',(0.727428616466516,-0.650090720524158,
-8.20137201430004));
#35307=CARTESIAN_POINT('Ctrl Pts',(0.554830637668136,-0.804089741468123,
-8.21844551120585));
#35308=CARTESIAN_POINT('Ctrl Pts',(0.447347381110085,-0.869095961842079,
-8.22754978352812));
#35309=CARTESIAN_POINT('Ctrl Pts',(0.190085901191508,-0.963314868905315,
-8.24780436867206));
#35310=CARTESIAN_POINT('Ctrl Pts',(0.0593773685688175,-0.973041258364987,
-8.25727548736166));
#35311=CARTESIAN_POINT('Ctrl Pts',(-0.164812872673331,-0.962733764741733,
-8.27383687615867));
#35312=CARTESIAN_POINT('Ctrl Pts',(-0.284713736492387,-0.935119778603541,
-8.28276631457827));
#35313=CARTESIAN_POINT('Ctrl Pts',(-0.50550084830103,-0.836647957297407,
-8.30064243112206));
#35314=CARTESIAN_POINT('Ctrl Pts',(-0.606159982100893,-0.765891415849572,
-8.3095718695417));
#35315=CARTESIAN_POINT('Ctrl Pts',(-0.763625880418338,-0.605978941163823,
-8.32613325833872));
#35316=CARTESIAN_POINT('Ctrl Pts',(-0.843724779454849,-0.502231702523655,
-8.33560437702835));
#35317=CARTESIAN_POINT('Ctrl Pts',(-0.945519248298758,-0.2478725910081,
-8.35585896217228));
#35318=CARTESIAN_POINT('Ctrl Pts',(-0.968971023406307,-0.124468890204761,
-8.36496323449451));
#35319=CARTESIAN_POINT('Ctrl Pts',(-0.969718982672265,0.106843023223732,
-8.3820367314003));
#35320=CARTESIAN_POINT('Ctrl Pts',(-0.952896543688453,0.234057028220043,
-8.39132649349289));
#35321=CARTESIAN_POINT('Ctrl Pts',(-0.848502485829639,0.485233231854166,
-8.41142565147333));
#35322=CARTESIAN_POINT('Ctrl Pts',(-0.777655722913494,0.59185047149092,
-8.42069415316726));
#35323=CARTESIAN_POINT('Ctrl Pts',(-0.599760572964985,0.773026160649791,
-8.43944526658599));
#35324=CARTESIAN_POINT('Ctrl Pts',(-0.494216597850722,0.844359793833639,
-8.44868727094887));
#35325=CARTESIAN_POINT('Ctrl Pts',(-0.258175251552615,0.942782111282781,
-8.46757219618098));
#35326=CARTESIAN_POINT('Ctrl Pts',(-0.130765826826681,0.968963911470147,
-8.4769847314769));
#35327=CARTESIAN_POINT('Ctrl Pts',(0.141141368764922,0.970728899308694,
-8.49707924627199));
#35328=CARTESIAN_POINT('Ctrl Pts',(0.263869764194396,0.939002707061653,
-8.50626004963336));
#35329=CARTESIAN_POINT('Ctrl Pts',(0.481737656636674,0.850692512192593,
-8.52361126800899));
#35330=CARTESIAN_POINT('Ctrl Pts',(0.59176831279853,0.779010613040467,-8.53311510089038));
#35331=CARTESIAN_POINT('Ctrl Pts',(0.79658086918973,0.576351120022354,-8.55441905425033));
#35332=CARTESIAN_POINT('Ctrl Pts',(0.85655168261401,0.460792364963875,-8.56380496118504));
#35333=CARTESIAN_POINT('Ctrl Pts',(0.925914408979285,0.30145456239256,-8.57662883281474));
#35334=CARTESIAN_POINT('Ctrl Pts',(0.968306855462314,0.171690743618857,
-8.5864674632087));
#35335=CARTESIAN_POINT('Ctrl Pts',(0.971136842407738,-0.111222607635891,
-8.607386887368));
#35336=CARTESIAN_POINT('Ctrl Pts',(0.948476372601592,-0.233665722796339,
-8.61641699610915));
#35337=CARTESIAN_POINT('Ctrl Pts',(0.866680152751073,-0.447298473368225,
-8.63329950791612));
#35338=CARTESIAN_POINT('Ctrl Pts',(0.805223850365105,-0.561155379775405,
-8.64265983493872));
#35339=CARTESIAN_POINT('Ctrl Pts',(0.616996729226062,-0.758109984772501,
-8.66279548833384));
#35340=CARTESIAN_POINT('Ctrl Pts',(0.513278309612551,-0.831427994749503,
-8.6719956535775));
#35341=CARTESIAN_POINT('Ctrl Pts',(0.313433860062192,-0.922580517982871,
-8.68821259695317));
#35342=CARTESIAN_POINT('Ctrl Pts',(0.190196585754628,-0.964233909424812,
-8.69761423747229));
#35343=CARTESIAN_POINT('Ctrl Pts',(-0.0936305289987827,-0.972967651905939,
-8.71858928893115));
#35344=CARTESIAN_POINT('Ctrl Pts',(-0.221167848283909,-0.952162992497402,
-8.72794202661001));
#35345=CARTESIAN_POINT('Ctrl Pts',(-0.459402726619743,-0.863875323940806,
-8.74671181142578));
#35346=CARTESIAN_POINT('Ctrl Pts',(-0.565831472897816,-0.79789193266667,
-8.75579515540647));
#35347=CARTESIAN_POINT('Ctrl Pts',(-0.753251241861667,-0.623077115572176,
-8.77471535175737));
#35348=CARTESIAN_POINT('Ctrl Pts',(-0.830121335358711,-0.517173188849598,
-8.78418479960575));
#35349=CARTESIAN_POINT('Ctrl Pts',(-0.943351358027896,-0.269030164792749,
-8.80434825399811));
#35350=CARTESIAN_POINT('Ctrl Pts',(-0.964048729229666,-0.144361544739943,
-8.81349685078773));
#35351=CARTESIAN_POINT('Ctrl Pts',(-0.973856013903567,0.0867272235402903,
-8.830565938197));
#35352=CARTESIAN_POINT('Ctrl Pts',(-0.954233524433085,0.21688920235632,
-8.84009505294611));
#35353=CARTESIAN_POINT('Ctrl Pts',(-0.867075844584167,0.451317654377397,
-8.85858893194271));
#35354=CARTESIAN_POINT('Ctrl Pts',(-0.802782957983994,0.556393866127063,
-8.86752821475173));
#35355=CARTESIAN_POINT('Ctrl Pts',(-0.652870452434931,0.724003523585264,
-8.8841223980206));
#35356=CARTESIAN_POINT('Ctrl Pts',(-0.55446394140407,0.810306450929307,
-8.89358160675802));
#35357=CARTESIAN_POINT('Ctrl Pts',(-0.307224094184925,0.927930571195957,
-8.91382274967911));
#35358=CARTESIAN_POINT('Ctrl Pts',(-0.185422291407291,0.959186925789853,
-8.92293638179297));
#35359=CARTESIAN_POINT('Ctrl Pts',(0.0456345727863289,0.974546843206883,
-8.94002896572626));
#35360=CARTESIAN_POINT('Ctrl Pts',(0.173547971727256,0.965729495041201,
-8.94931166607434));
#35361=CARTESIAN_POINT('Ctrl Pts',(0.430853797139274,0.877377505913247,
-8.96941319072267));
#35362=CARTESIAN_POINT('Ctrl Pts',(0.541843176296524,0.813335765249629,
-8.9786906394001));
#35363=CARTESIAN_POINT('Ctrl Pts',(0.73384309180208,0.647133684352001,-8.99744472962074));
#35364=CARTESIAN_POINT('Ctrl Pts',(0.811550342016074,0.546324878994273,
-9.00667923390641));
#35365=CARTESIAN_POINT('Ctrl Pts',(0.924606730993031,0.317066970465836,
-9.02555375849916));
#35366=CARTESIAN_POINT('Ctrl Pts',(0.958807608424653,0.191445444025986,
-9.03497445753251));
#35367=CARTESIAN_POINT('Ctrl Pts',(0.977526763343717,-0.0776682503544696,
-9.05491365636751));
#35368=CARTESIAN_POINT('Ctrl Pts',(0.95446645028955,-0.200390361982081,
-9.06396793124116));
#35369=CARTESIAN_POINT('Ctrl Pts',(0.921755948887285,-0.300215476155852,
-9.07172448866066));
#35370=CARTESIAN_POINT('',(-1.082164275363,0.6256360612436,-7.350042088616));
#35371=CARTESIAN_POINT('Ctrl Pts',(0.9134609739509,-0.2804380286241,-6.038826865909));
#35372=CARTESIAN_POINT('Ctrl Pts',(0.8472860717472,-0.4959872211307,-6.055726957101));
#35373=CARTESIAN_POINT('Ctrl Pts',(0.5562136135091,-0.8771468390869,-6.089527139485));
#35374=CARTESIAN_POINT('Ctrl Pts',(-0.1479368148011,-1.028187435632,-6.140227413061));
#35375=CARTESIAN_POINT('Ctrl Pts',(-0.7809283426593,-0.6849092846179,-6.190927686637));
#35376=CARTESIAN_POINT('Ctrl Pts',(-1.038659599125,-0.01255389358613,-6.241627960213));
#35377=CARTESIAN_POINT('Ctrl Pts',(-0.7972539277561,0.6658500520475,-6.292328233789));
#35378=CARTESIAN_POINT('Ctrl Pts',(-0.1727259298309,1.024272829731,-6.343028507365));
#35379=CARTESIAN_POINT('Ctrl Pts',(0.5348065635462,0.8904782587224,-6.393728780941));
#35380=CARTESIAN_POINT('Ctrl Pts',(0.9853354927582,0.3287604328168,-6.444429054517));
#35381=CARTESIAN_POINT('Ctrl Pts',(0.962357464606,-0.3909444763488,-6.495129328093));
#35382=CARTESIAN_POINT('Ctrl Pts',(0.4769146324961,-0.9227794476316,-6.545829601669));
#35383=CARTESIAN_POINT('Ctrl Pts',(-0.2377114659494,-1.011168992981,-6.596529875245));
#35384=CARTESIAN_POINT('Ctrl Pts',(-0.8381043522096,-0.6136371639345,-6.647230148821));
#35385=CARTESIAN_POINT('Ctrl Pts',(-1.035742780039,0.07878050272052,-6.697930422397));
#35386=CARTESIAN_POINT('Ctrl Pts',(-0.7356507985394,0.7333398779728,-6.748630695973));
#35387=CARTESIAN_POINT('Ctrl Pts',(-0.08203883102345,1.035489789534,-6.799330969549));
#35388=CARTESIAN_POINT('Ctrl Pts',(0.6109972307107,0.8400308673404,-6.850031243125));
#35389=CARTESIAN_POINT('Ctrl Pts',(1.010416085914,0.240891692159,-6.900731516701));
#35390=CARTESIAN_POINT('Ctrl Pts',(0.9242753777111,-0.4740089663433,-6.951431790277));
#35391=CARTESIAN_POINT('Ctrl Pts',(0.3939703741324,-0.9611226864031,-7.002132063853));
#35392=CARTESIAN_POINT('Ctrl Pts',(-0.3256586966498,-0.9863649869347,-7.052832337429));
#35393=CARTESIAN_POINT('Ctrl Pts',(-0.8887911546714,-0.5376055773403,-7.103532611005));
#35394=CARTESIAN_POINT('Ctrl Pts',(-1.024811406463,0.169502380053,-7.154232884581));
#35395=CARTESIAN_POINT('Ctrl Pts',(-0.668354359975,0.7951552821763,-7.204933158157));
#35396=CARTESIAN_POINT('Ctrl Pts',(0.009283076393916,1.038693063406,-7.255633431733));
#35397=CARTESIAN_POINT('Ctrl Pts',(0.682459562086,0.7830827132473,-7.306333705309));
#35398=CARTESIAN_POINT('Ctrl Pts',(1.027677067702,0.151158595784,-7.357033978885));
#35399=CARTESIAN_POINT('Ctrl Pts',(0.8790411425118,-0.5534047225185,-7.407734252461));
#35400=CARTESIAN_POINT('Ctrl Pts',(0.3079748064376,-0.9920296778312,-7.458434526037));
#35401=CARTESIAN_POINT('Ctrl Pts',(-0.41107659886,-0.9539212936056,-7.509134799613));
#35402=CARTESIAN_POINT('Ctrl Pts',(-0.9326337707599,-0.4574373767019,-7.559835073189));
#35403=CARTESIAN_POINT('Ctrl Pts',(-1.005822266638,0.2590014075395,-7.610535346765));
#35404=CARTESIAN_POINT('Ctrl Pts',(-0.7328469964043,0.6533240319803,-7.644335529149));
#35405=CARTESIAN_POINT('Ctrl Pts',(-0.548159772547,0.7826731773806,-7.661235620341));
#35406=CARTESIAN_POINT('Ctrl Pts',(1.011899778108,-0.3106593352427,-6.098278598537));
#35407=CARTESIAN_POINT('Ctrl Pts',(0.9385935605836,-0.5494371115119,-6.115178689729));
#35408=CARTESIAN_POINT('Ctrl Pts',(0.6161537801183,-0.9716722631302,-6.148978872113));
#35409=CARTESIAN_POINT('Ctrl Pts',(-0.1638791741958,-1.138989697031,-6.199679145689));
#35410=CARTESIAN_POINT('Ctrl Pts',(-0.8650848138998,-0.7587182954638,-6.250379419265));
#35411=CARTESIAN_POINT('Ctrl Pts',(-1.150590389579,-0.0139067595622,-6.301079692841));
#35412=CARTESIAN_POINT('Ctrl Pts',(-0.8831697199965,0.7376051513243,-6.351779966417));
#35413=CARTESIAN_POINT('Ctrl Pts',(-0.1913396795852,1.134653234986,-6.402480239993));
#35414=CARTESIAN_POINT('Ctrl Pts',(0.5924398068615,0.9864403385659,-6.453180513569));
#35415=CARTESIAN_POINT('Ctrl Pts',(1.091519829436,0.3641891865167,-6.503880787145));
#35416=CARTESIAN_POINT('Ctrl Pts',(1.066065582072,-0.4330744718724,-6.554581060721));
#35417=CARTESIAN_POINT('Ctrl Pts',(0.5283091719965,-1.022222453864,-6.605281334297));
#35418=CARTESIAN_POINT('Ctrl Pts',(-0.2633283594015,-1.120137267826,-6.655981607873));
#35419=CARTESIAN_POINT('Ctrl Pts',(-0.9284223762335,-0.6797655594833,-6.706681881449));
#35420=CARTESIAN_POINT('Ctrl Pts',(-1.1473592405,0.0872702561964,-6.757382155025));
#35421=CARTESIAN_POINT('Ctrl Pts',(-0.8149279509853,0.8123679948675,-6.808082428601));
#35422=CARTESIAN_POINT('Ctrl Pts',(-0.09087971711565,1.147078986561,-6.858782702177));
#35423=CARTESIAN_POINT('Ctrl Pts',(0.6768411347738,0.9305565015973,-6.909482975753));
#35424=CARTESIAN_POINT('Ctrl Pts',(1.119303223991,0.2668513015826,-6.960183249329));
#35425=CARTESIAN_POINT('Ctrl Pts',(1.023879592328,-0.5250903777413,-7.010883522905));
#35426=CARTESIAN_POINT('Ctrl Pts',(0.4364264544781,-1.064697738426,-7.061583796481));
#35427=CARTESIAN_POINT('Ctrl Pts',(-0.3607531928305,-1.092660266695,-7.112284070057));
#35428=CARTESIAN_POINT('Ctrl Pts',(-0.9845714243337,-0.5955404554036,-7.162984343633));
#35429=CARTESIAN_POINT('Ctrl Pts',(-1.135249851252,0.1877687450866,-7.213684617209));
#35430=CARTESIAN_POINT('Ctrl Pts',(-0.7403793351246,0.8808449146057,-7.264384890785));
#35431=CARTESIAN_POINT('Ctrl Pts',(0.01028346389286,1.150627460127,-7.315085164361));
#35432=CARTESIAN_POINT('Ctrl Pts',(0.7560045794353,0.8674713494848,-7.365785437937));
#35433=CARTESIAN_POINT('Ctrl Pts',(1.138424329478,0.1674481492858,-7.416485711513));
#35434=CARTESIAN_POINT('Ctrl Pts',(0.9737707055048,-0.613042189967,-7.467185985089));
#35435=CARTESIAN_POINT('Ctrl Pts',(0.34116360434,-1.098935411036,-7.517886258665));
#35436=CARTESIAN_POINT('Ctrl Pts',(-0.455376125564,-1.056720290038,-7.568586532241));
#35437=CARTESIAN_POINT('Ctrl Pts',(-1.033138724697,-0.5067329565058,-7.619286805817));
#35438=CARTESIAN_POINT('Ctrl Pts',(-1.114214353379,0.2869126041425,-7.669987079393));
#35439=CARTESIAN_POINT('Ctrl Pts',(-0.8118219980882,0.7237292690611,-7.703787261777));
#35440=CARTESIAN_POINT('Ctrl Pts',(-0.607232019786,0.867017680128,-7.720687352969));
#35441=CARTESIAN_POINT('Ctrl Pts',(1.110338582265,-0.3408806418612,-6.157730331166));
#35442=CARTESIAN_POINT('Ctrl Pts',(1.02990104942,-0.6028870018931,-6.174630422358));
#35443=CARTESIAN_POINT('Ctrl Pts',(0.6760939467275,-1.066197687173,-6.208430604742));
#35444=CARTESIAN_POINT('Ctrl Pts',(-0.1798215335905,-1.249791958429,-6.259130878318));
#35445=CARTESIAN_POINT('Ctrl Pts',(-0.9492412851402,-0.8325273063098,-6.309831151894));
#35446=CARTESIAN_POINT('Ctrl Pts',(-1.262521180034,-0.01525962553827,-6.36053142547));
#35447=CARTESIAN_POINT('Ctrl Pts',(-0.9690855122368,0.8093602506011,-6.411231699046));
#35448=CARTESIAN_POINT('Ctrl Pts',(-0.2099534293395,1.24503364024,-6.461931972622));
#35449=CARTESIAN_POINT('Ctrl Pts',(0.6500730501767,1.08240241841,-6.512632246198));
#35450=CARTESIAN_POINT('Ctrl Pts',(1.197704166115,0.3996179402166,-6.563332519774));
#35451=CARTESIAN_POINT('Ctrl Pts',(1.169773699538,-0.475204467396,-6.61403279335));
#35452=CARTESIAN_POINT('Ctrl Pts',(0.5797037114969,-1.121665460096,-6.664733066926));
#35453=CARTESIAN_POINT('Ctrl Pts',(-0.2889452528537,-1.22910554267,-6.715433340502));
#35454=CARTESIAN_POINT('Ctrl Pts',(-1.018740400257,-0.7458939550322,-6.766133614078));
#35455=CARTESIAN_POINT('Ctrl Pts',(-1.25897570096,0.09576000967229,-6.816833887654));
#35456=CARTESIAN_POINT('Ctrl Pts',(-0.8942051034311,0.8913961117622,-6.86753416123));
#35457=CARTESIAN_POINT('Ctrl Pts',(-0.09972060320785,1.258668183588,-6.918234434806));
#35458=CARTESIAN_POINT('Ctrl Pts',(0.742685038837,1.021082135854,-6.968934708382));
#35459=CARTESIAN_POINT('Ctrl Pts',(1.228190362067,0.2928109110062,-7.019634981958));
#35460=CARTESIAN_POINT('Ctrl Pts',(1.123483806945,-0.5761717891393,-7.070335255534));
#35461=CARTESIAN_POINT('Ctrl Pts',(0.4788825348239,-1.168272790448,-7.12103552911));
#35462=CARTESIAN_POINT('Ctrl Pts',(-0.3958476890111,-1.198955546455,-7.171735802686));
#35463=CARTESIAN_POINT('Ctrl Pts',(-1.080351693996,-0.6534753334669,-7.222436076262));
#35464=CARTESIAN_POINT('Ctrl Pts',(-1.245688296041,0.2060351101202,-7.273136349838));
#35465=CARTESIAN_POINT('Ctrl Pts',(-0.8124043102742,0.966534547035,-7.323836623414));
#35466=CARTESIAN_POINT('Ctrl Pts',(0.0112838513918,1.262561856849,-7.37453689699));
#35467=CARTESIAN_POINT('Ctrl Pts',(0.8295495967846,0.9518599857224,-7.425237170566));
#35468=CARTESIAN_POINT('Ctrl Pts',(1.249171591254,0.1837377027876,-7.475937444142));
#35469=CARTESIAN_POINT('Ctrl Pts',(1.068500268498,-0.6726796574155,-7.526637717718));
#35470=CARTESIAN_POINT('Ctrl Pts',(0.3743524022424,-1.20584114424,-7.577337991294));
#35471=CARTESIAN_POINT('Ctrl Pts',(-0.499675652268,-1.15951928647,-7.62803826487));
#35472=CARTESIAN_POINT('Ctrl Pts',(-1.133643678633,-0.5560285363098,-7.678738538446));
#35473=CARTESIAN_POINT('Ctrl Pts',(-1.222606440119,0.3148238007455,-7.729438812022));
#35474=CARTESIAN_POINT('Ctrl Pts',(-0.8907969997721,0.7941345061418,-7.763238994406));
#35475=CARTESIAN_POINT('Ctrl Pts',(-0.666304267025,0.9513621828753,-7.780139085598));
#35476=CARTESIAN_POINT('Ctrl Pts',(1.208777386421,-0.3711019484798,-6.217182063794));
#35477=CARTESIAN_POINT('Ctrl Pts',(1.121208538256,-0.6563368922743,-6.234082154986));
#35478=CARTESIAN_POINT('Ctrl Pts',(0.7360341133366,-1.160723111217,-6.26788233737));
#35479=CARTESIAN_POINT('Ctrl Pts',(-0.1957638929852,-1.360594219827,-6.318582610946));
#35480=CARTESIAN_POINT('Ctrl Pts',(-1.033397756381,-0.9063363171557,-6.369282884522));
#35481=CARTESIAN_POINT('Ctrl Pts',(-1.374451970489,-0.01661249151435,-6.419983158098));
#35482=CARTESIAN_POINT('Ctrl Pts',(-1.055001304477,0.8811153498779,-6.470683431674));
#35483=CARTESIAN_POINT('Ctrl Pts',(-0.2285671790938,1.355414045495,-6.52138370525));
#35484=CARTESIAN_POINT('Ctrl Pts',(0.707706293492,1.178364498253,-6.572083978826));
#35485=CARTESIAN_POINT('Ctrl Pts',(1.303888502793,0.4350466939165,-6.622784252402));
#35486=CARTESIAN_POINT('Ctrl Pts',(1.273481817004,-0.5173344629195,-6.673484525978));
#35487=CARTESIAN_POINT('Ctrl Pts',(0.6310982509973,-1.221108466328,-6.724184799554));
#35488=CARTESIAN_POINT('Ctrl Pts',(-0.3145621463059,-1.338073817515,-6.77488507313));
#35489=CARTESIAN_POINT('Ctrl Pts',(-1.109058424281,-0.8120223505811,-6.825585346706));
#35490=CARTESIAN_POINT('Ctrl Pts',(-1.370592161421,0.1042497631482,-6.876285620282));
#35491=CARTESIAN_POINT('Ctrl Pts',(-0.973482255877,0.9704242286569,-6.926985893858));
#35492=CARTESIAN_POINT('Ctrl Pts',(-0.1085614893,1.370257380614,-6.977686167434));
#35493=CARTESIAN_POINT('Ctrl Pts',(0.8085289429002,1.111607770111,-7.02838644101));
#35494=CARTESIAN_POINT('Ctrl Pts',(1.337077500144,0.3187705204298,-7.079086714586));
#35495=CARTESIAN_POINT('Ctrl Pts',(1.223088021562,-0.6272532005374,-7.129786988162));
#35496=CARTESIAN_POINT('Ctrl Pts',(0.5213386151697,-1.271847842471,-7.180487261738));
#35497=CARTESIAN_POINT('Ctrl Pts',(-0.4309421851917,-1.305250826215,-7.231187535314));
#35498=CARTESIAN_POINT('Ctrl Pts',(-1.176131963658,-0.7114102115302,-7.28188780889));
#35499=CARTESIAN_POINT('Ctrl Pts',(-1.35612674083,0.2243014751538,-7.332588082466));
#35500=CARTESIAN_POINT('Ctrl Pts',(-0.8844292854238,1.052224179464,-7.383288356042));
#35501=CARTESIAN_POINT('Ctrl Pts',(0.01228423889075,1.37449625357,-7.433988629618));
#35502=CARTESIAN_POINT('Ctrl Pts',(0.9030946141339,1.03624862196,-7.484688903194));
#35503=CARTESIAN_POINT('Ctrl Pts',(1.359918853029,0.2000272562895,-7.53538917677));
#35504=CARTESIAN_POINT('Ctrl Pts',(1.163229831491,-0.732317124864,-7.586089450346));
#35505=CARTESIAN_POINT('Ctrl Pts',(0.4075412001447,-1.312746877444,-7.636789723922));
#35506=CARTESIAN_POINT('Ctrl Pts',(-0.5439751789721,-1.262318282903,-7.687489997498));
#35507=CARTESIAN_POINT('Ctrl Pts',(-1.23414863257,-0.6053241161137,-7.738190271074));
#35508=CARTESIAN_POINT('Ctrl Pts',(-1.330998526859,0.3427349973485,-7.78889054465));
#35509=CARTESIAN_POINT('Ctrl Pts',(-0.9697720014561,0.8645397432226,-7.822690727034));
#35510=CARTESIAN_POINT('Ctrl Pts',(-0.725376514264,1.035706685623,-7.839590818226));
#35511=CARTESIAN_POINT('',(0.9280544183911,-0.8364143225921,-6.23965809256072));
#35512=CARTESIAN_POINT('Ctrl Pts',(-1.08144091415521,0.625238554653748,
-7.35009940962399));
#35513=CARTESIAN_POINT('Ctrl Pts',(-1.13845941588873,0.526794183586659,
-7.34364665860282));
#35514=CARTESIAN_POINT('Ctrl Pts',(-1.19439067109551,0.400143823427812,
-7.33585368731547));
#35515=CARTESIAN_POINT('Ctrl Pts',(-1.25119108729651,0.118585425996973,
-7.31907932790072));
#35516=CARTESIAN_POINT('Ctrl Pts',(-1.25593947156391,-0.0140855441947595,
-7.31159686950582));
#35517=CARTESIAN_POINT('Ctrl Pts',(-1.22529757201621,-0.276529705002004,
-7.29662426640538));
#35518=CARTESIAN_POINT('Ctrl Pts',(-1.18906778938012,-0.406719794981607,
-7.28908149497592));
#35519=CARTESIAN_POINT('Ctrl Pts',(-1.10137406144739,-0.595950494314858,
-7.27699564285035));
#35520=CARTESIAN_POINT('Ctrl Pts',(-1.06370367262132,-0.660673233860386,
-7.27262032993749));
#35521=CARTESIAN_POINT('Ctrl Pts',(-0.971992258317847,-0.789531566420169,
-7.26351469895125));
#35522=CARTESIAN_POINT('Ctrl Pts',(-0.917017581242872,-0.852353804178172,
-7.2587927042533));
#35523=CARTESIAN_POINT('Ctrl Pts',(-0.756971603418245,-1.00285400129472,
-7.24633659192418));
#35524=CARTESIAN_POINT('Ctrl Pts',(-0.642298996377849,-1.08057458876947,
-7.23860555019741));
#35525=CARTESIAN_POINT('Ctrl Pts',(-0.453827957240571,-1.16684560048204,
-7.22658638206331));
#35526=CARTESIAN_POINT('Ctrl Pts',(-0.387529057819546,-1.19043933362089,
-7.22247029669801));
#35527=CARTESIAN_POINT('Ctrl Pts',(-0.238834653791269,-1.22930303428804,
-7.21360777094392));
#35528=CARTESIAN_POINT('Ctrl Pts',(-0.156340711699991,-1.24219522029809,
-7.20888047579269));
#35529=CARTESIAN_POINT('Ctrl Pts',(0.0641921503111542,-1.25493503764991,
-7.19635390921882));
#35530=CARTESIAN_POINT('Ctrl Pts',(0.203231193855402,-1.24059849399102,
-7.1885643218617));
#35531=CARTESIAN_POINT('Ctrl Pts',(0.400249068389142,-1.18604301244094,
-7.17672562103673));
#35532=CARTESIAN_POINT('Ctrl Pts',(0.462519894877283,-1.16315139144511,
-7.17284152673707));
#35533=CARTESIAN_POINT('Ctrl Pts',(0.669055230915653,-1.06741042621854,
-7.15968337989695));
#35534=CARTESIAN_POINT('Ctrl Pts',(0.801914381946556,-0.970913148856214,
-7.15062451754881));
#35535=CARTESIAN_POINT('Ctrl Pts',(1.01686078903117,-0.742279077871929,
-7.13276658058505));
#35536=CARTESIAN_POINT('Ctrl Pts',(1.0968524668718,-0.617844041552233,-7.12420955314268));
#35537=CARTESIAN_POINT('Ctrl Pts',(1.18530342790498,-0.403842745066263,
-7.11088809527967));
#35538=CARTESIAN_POINT('Ctrl Pts',(1.20932189186302,-0.32388207356038,-7.10616843028997));
#35539=CARTESIAN_POINT('Ctrl Pts',(1.25150036893193,-0.109861760058388,
-7.09380383094239));
#35540=CARTESIAN_POINT('Ctrl Pts',(1.2566190093772,0.0269369245505145,-7.08615896767945));
#35541=CARTESIAN_POINT('Ctrl Pts',(1.23004537676662,0.23457038514643,-7.074016349761));
#35542=CARTESIAN_POINT('Ctrl Pts',(1.213950499144,0.306782464954891,-7.06969350282979));
#35543=CARTESIAN_POINT('Ctrl Pts',(1.16603740630127,0.456571322769034,-7.06063903711535));
#35544=CARTESIAN_POINT('Ctrl Pts',(1.13276358119362,0.533151262793348,-7.05591658816548));
#35545=CARTESIAN_POINT('Ctrl Pts',(1.02636194887124,0.724653732998469,-7.0434971171023));
#35546=CARTESIAN_POINT('Ctrl Pts',(0.941242131519351,0.833109088899172,
-7.03580329128069));
#35547=CARTESIAN_POINT('Ctrl Pts',(0.788394273768947,0.972607904358993,
-7.0238063653535));
#35548=CARTESIAN_POINT('Ctrl Pts',(0.732231243339065,1.015483219647,-7.019673727507));
#35549=CARTESIAN_POINT('Ctrl Pts',(0.60222128539102,1.09797945750687,-7.01079519081006));
#35550=CARTESIAN_POINT('Ctrl Pts',(0.527586212742716,1.13540556649639,-7.00606801275208));
#35551=CARTESIAN_POINT('Ctrl Pts',(0.321385388788767,1.21478868557968,-6.99353817344243));
#35552=CARTESIAN_POINT('Ctrl Pts',(0.184535948543945,1.24352468862241,-6.98574504666367));
#35553=CARTESIAN_POINT('Ctrl Pts',(-0.0198864739890845,1.25160529301129,
-6.97389700631672));
#35554=CARTESIAN_POINT('Ctrl Pts',(-0.0862656311501007,1.24876529684857,
-6.97000742825624));
#35555=CARTESIAN_POINT('Ctrl Pts',(-0.312234498867914,1.22045076352206,
-6.95684511453382));
#35556=CARTESIAN_POINT('Ctrl Pts',(-0.46816438855612,1.16899975646828,-6.94778687483531));
#35557=CARTESIAN_POINT('Ctrl Pts',(-0.741904897123531,1.01702921803696,
-6.92996880361027));
#35558=CARTESIAN_POINT('Ctrl Pts',(-0.855594423444135,0.923368273219295,
-6.92144739328836));
#35559=CARTESIAN_POINT('Ctrl Pts',(-1.00491474173641,0.747120993151983,
-6.90815669347837));
#35560=CARTESIAN_POINT('Ctrl Pts',(-1.05224489991832,0.678340844485654,
-6.90343656893941));
#35561=CARTESIAN_POINT('Ctrl Pts',(-1.15794237658074,0.48736397670007,-6.89106390268326));
#35562=CARTESIAN_POINT('Ctrl Pts',(-1.20469386492157,0.358548019629921,
-6.88341191542826));
#35563=CARTESIAN_POINT('Ctrl Pts',(-1.24277040598387,0.153182356417834,
-6.87129720714745));
#35564=CARTESIAN_POINT('Ctrl Pts',(-1.24951852581418,0.0801083073668442,
-6.86700856005424));
#35565=CARTESIAN_POINT('Ctrl Pts',(-1.24990423010732,-0.076565829009687,
-6.85798576654047));
#35566=CARTESIAN_POINT('Ctrl Pts',(-1.24174330493025,-0.159663077316491,
-6.85326245846073));
#35567=CARTESIAN_POINT('Ctrl Pts',(-1.19919680323486,-0.374893580986194,
-6.84082429682175));
#35568=CARTESIAN_POINT('Ctrl Pts',(-1.15131189136542,-0.504534513233835,
-6.8331136881208));
#35569=CARTESIAN_POINT('Ctrl Pts',(-1.04881278268726,-0.68366199337213,
-6.82115117111684));
#35570=CARTESIAN_POINT('Ctrl Pts',(-1.00904387182181,-0.74100695815593,
-6.81706860902981));
#35571=CARTESIAN_POINT('Ctrl Pts',(-0.911352540719992,-0.858895892747815,
-6.80823628859876));
#35572=CARTESIAN_POINT('Ctrl Pts',(-0.851888287296867,-0.91749957652705,
-6.80350789605541));
#35573=CARTESIAN_POINT('Ctrl Pts',(-0.668265026613998,-1.06622345316516,
-6.79010655339088));
#35574=CARTESIAN_POINT('Ctrl Pts',(-0.524441825712136,-1.14729178292643,
-6.78096206157405));
#35575=CARTESIAN_POINT('Ctrl Pts',(-0.286619386009769,-1.2191432792449,
-6.76647656088353));
#35576=CARTESIAN_POINT('Ctrl Pts',(-0.2106650741897,-1.23429105046874,-6.76199825471631));
#35577=CARTESIAN_POINT('Ctrl Pts',(0.0254923040591906,-1.25902399119274,
-6.74840675794588));
#35578=CARTESIAN_POINT('Ctrl Pts',(0.188210080940334,-1.24518018289136,
-6.73941201231742));
#35579=CARTESIAN_POINT('Ctrl Pts',(0.533113525267708,-1.14801824337071,
-6.718874944052));
#35580=CARTESIAN_POINT('Ctrl Pts',(0.670006874045706,-1.06151480982223,
-6.70956035198521));
#35581=CARTESIAN_POINT('Ctrl Pts',(0.891167699619736,-0.889705845031928,
-6.69361240794748));
#35582=CARTESIAN_POINT('Ctrl Pts',(0.999690126438071,-0.766475194873538,
-6.68455777859975));
#35583=CARTESIAN_POINT('Ctrl Pts',(1.11677488123714,-0.565928020540905,
-6.67115191316097));
#35584=CARTESIAN_POINT('Ctrl Pts',(1.14705574486821,-0.50181209517784,-6.66700163097715));
#35585=CARTESIAN_POINT('Ctrl Pts',(1.2170828887025,-0.311952024704957,-6.65528522804467));
#35586=CARTESIAN_POINT('Ctrl Pts',(1.24269004423336,-0.181621278522362,
-6.64786488682457));
#35587=CARTESIAN_POINT('Ctrl Pts',(1.2515385009026,0.0325279813153482,-6.63571498520908));
#35588=CARTESIAN_POINT('Ctrl Pts',(1.24685187992131,0.116008148491328,-6.63098694881452));
#35589=CARTESIAN_POINT('Ctrl Pts',(1.21062276726679,0.345659149496376,-6.61760475355315));
#35590=CARTESIAN_POINT('Ctrl Pts',(1.16157099219993,0.485157474530085,-6.60905675358139));
#35591=CARTESIAN_POINT('Ctrl Pts',(1.0063728134479,0.756970110543001,-6.59124987992135));
#35592=CARTESIAN_POINT('Ctrl Pts',(0.89959439455553,0.881959799323835,-6.58217933370859));
#35593=CARTESIAN_POINT('Ctrl Pts',(0.719369820494962,1.02452385547995,-6.56888886194693));
#35594=CARTESIAN_POINT('Ctrl Pts',(0.662440624582576,1.06222165136825,-6.56489101070615));
#35595=CARTESIAN_POINT('Ctrl Pts',(0.48485220812677,1.15936247999066,-6.55318361156413));
#35596=CARTESIAN_POINT('Ctrl Pts',(0.356900686552398,1.20438281988483,-6.54561797582988));
#35597=CARTESIAN_POINT('Ctrl Pts',(0.144393426698886,1.24358475220579,-6.53336382990338));
#35598=CARTESIAN_POINT('Ctrl Pts',(0.0620477895094899,1.25068971498076,
-6.52868408387922));
#35599=CARTESIAN_POINT('Ctrl Pts',(-0.0936680948074589,1.24858819902552,
-6.51970677548154));
#35600=CARTESIAN_POINT('Ctrl Pts',(-0.166508017661877,1.24104336575588,
-6.51542333541335));
#35601=CARTESIAN_POINT('Ctrl Pts',(-0.365628590584132,1.20189232020038,
-6.50366515590112));
#35602=CARTESIAN_POINT('Ctrl Pts',(-0.488609145957327,1.15677135627177,
-6.49633876007959));
#35603=CARTESIAN_POINT('Ctrl Pts',(-0.674921949564665,1.0544298326615,-6.48429081890586));
#35604=CARTESIAN_POINT('Ctrl Pts',(-0.743941992643752,1.00724740684214,
-6.47956668412178));
#35605=CARTESIAN_POINT('Ctrl Pts',(-0.925097327137965,0.85473233049542,
-6.46595196737));
#35606=CARTESIAN_POINT('Ctrl Pts',(-1.02191142899692,0.736327243566084,
-6.45711337782292));
#35607=CARTESIAN_POINT('Ctrl Pts',(-1.17389129062308,0.455826182550516,
-6.43896668114914));
#35608=CARTESIAN_POINT('Ctrl Pts',(-1.22379685651126,0.299157012952662,
-6.42989288930313));
#35609=CARTESIAN_POINT('Ctrl Pts',(-1.24980716087092,0.0712298930941525,
-6.41662001494264));
#35610=CARTESIAN_POINT('Ctrl Pts',(-1.25182415933548,0.003398592608898,
-6.41264668251563));
#35611=CARTESIAN_POINT('Ctrl Pts',(-1.24088522508175,-0.198759275666808,
-6.40094010361306));
#35612=CARTESIAN_POINT('Ctrl Pts',(-1.21161252387838,-0.331695448278339,
-6.39335019059184));
#35613=CARTESIAN_POINT('Ctrl Pts',(-1.13265884776994,-0.53334288847137,
-6.38106921400184));
#35614=CARTESIAN_POINT('Ctrl Pts',(-1.09525941863046,-0.607048262681095,
-6.37638841497169));
#35615=CARTESIAN_POINT('Ctrl Pts',(-1.01180373953895,-0.737481050653887,
-6.36745862467547));
#35616=CARTESIAN_POINT('Ctrl Pts',(-0.967570521889716,-0.794721975412659,
-6.36322624106468));
#35617=CARTESIAN_POINT('Ctrl Pts',(-0.829606230581431,-0.943504132115711,
-6.35146920984007));
#35618=CARTESIAN_POINT('Ctrl Pts',(-0.725782883999061,-1.02485139482369,
-6.34409347751394));
#35619=CARTESIAN_POINT('Ctrl Pts',(-0.539826516001505,-1.12958576426288,
-6.33199527779046));
#35620=CARTESIAN_POINT('Ctrl Pts',(-0.463351068505991,-1.16333510483609,
-6.32727081415333));
#35621=CARTESIAN_POINT('Ctrl Pts',(-0.236432299447394,-1.23737660634955,
-6.31354543564448));
#35622=CARTESIAN_POINT('Ctrl Pts',(-0.083838606894931,-1.25671070950491,
-6.30466986447607));
#35623=CARTESIAN_POINT('Ctrl Pts',(0.234319781210057,-1.23724994774721,
-6.28655599010737));
#35624=CARTESIAN_POINT('Ctrl Pts',(0.393564405146679,-1.19675981713808,
-6.27748794480623));
#35625=CARTESIAN_POINT('Ctrl Pts',(0.611700856771692,-1.09306215307407,
-6.26349273975741));
#35626=CARTESIAN_POINT('Ctrl Pts',(0.680192833559366,-1.05171705293845,
-6.25880773384765));
#35627=CARTESIAN_POINT('Ctrl Pts',(0.810992282165546,-0.954164575612996,
-6.24939904171304));
#35628=CARTESIAN_POINT('Ctrl Pts',(0.872476840637322,-0.897918805592539,
-6.2446792108443));
#35629=CARTESIAN_POINT('Ctrl Pts',(0.927936718582964,-0.836284130747026,
-6.23997634988408));
#35630=CARTESIAN_POINT('',(0.720545178071692,-0.649395442066378,-6.07837558621596));
#35631=CARTESIAN_POINT('',(0.7205452572168,-0.6493955129983,-6.078375595519));
#35632=CARTESIAN_POINT('Ctrl Pts',(0.720108814885489,-0.649004361933079,
-6.07835980896107));
#35633=CARTESIAN_POINT('Ctrl Pts',(0.649924585346467,-0.727158430109657,
-6.08611596373328));
#35634=CARTESIAN_POINT('Ctrl Pts',(0.555079528159261,-0.80838028401483,
-6.09517025738535));
#35635=CARTESIAN_POINT('Ctrl Pts',(0.312518521341734,-0.926442422296045,
-6.11510971969884));
#35636=CARTESIAN_POINT('Ctrl Pts',(0.186587724758927,-0.959486368703356,
-6.12453041873231));
#35637=CARTESIAN_POINT('Ctrl Pts',(-0.0685031170829461,-0.975905812045906,
-6.14340494332513));
#35638=CARTESIAN_POINT('Ctrl Pts',(-0.194639787589674,-0.958865497291617,
-6.15263944761075));
#35639=CARTESIAN_POINT('Ctrl Pts',(-0.434477044399925,-0.875407786476393,
-6.17139353783132));
#35640=CARTESIAN_POINT('Ctrl Pts',(-0.545358094112512,-0.811178668098797,
-6.18067098650868));
#35641=CARTESIAN_POINT('Ctrl Pts',(-0.750315949779605,-0.63228026348299,
-6.2007725111569));
#35642=CARTESIAN_POINT('Ctrl Pts',(-0.82178362970336,-0.525828612563066,
-6.21005521150494));
#35643=CARTESIAN_POINT('Ctrl Pts',(-0.92376570001596,-0.317927532987132,
-6.22714779543817));
#35644=CARTESIAN_POINT('Ctrl Pts',(-0.957455434114765,-0.196776219833821,
-6.23626142755198));
#35645=CARTESIAN_POINT('Ctrl Pts',(-0.978889084396869,0.076177209082542,
-6.25650257047306));
#35646=CARTESIAN_POINT('Ctrl Pts',(-0.953200947514868,0.204521107671369,
-6.26596177921051));
#35647=CARTESIAN_POINT('Ctrl Pts',(-0.882751937182648,0.418071320821551,
-6.2825559624794));
#35648=CARTESIAN_POINT('Ctrl Pts',(-0.82377256068534,0.52621945391236,-6.29149524528844));
#35649=CARTESIAN_POINT('Ctrl Pts',(-0.664104034634088,0.718726913669791,
-6.30998912428504));
#35650=CARTESIAN_POINT('Ctrl Pts',(-0.561095305033122,0.800680464223247,
-6.31951823903411));
#35651=CARTESIAN_POINT('Ctrl Pts',(-0.35593723957073,0.90749043488932,-6.33658732644336));
#35652=CARTESIAN_POINT('Ctrl Pts',(-0.237570247179751,0.95176120530112,
-6.34573592323295));
#35653=CARTESIAN_POINT('Ctrl Pts',(0.0339733113907493,0.977453504160468,
-6.36589937762531));
#35654=CARTESIAN_POINT('Ctrl Pts',(0.16410775167376,0.963681052608347,-6.37536882547371));
#35655=CARTESIAN_POINT('Ctrl Pts',(0.409123503410254,0.888490152389851,
-6.39428902182473));
#35656=CARTESIAN_POINT('Ctrl Pts',(0.519411539030056,0.829182183637508,
-6.40337236580551));
#35657=CARTESIAN_POINT('Ctrl Pts',(0.714797598489669,0.666778804844548,
-6.42214215062138));
#35658=CARTESIAN_POINT('Ctrl Pts',(0.79646597496153,0.566634519196591,-6.43149488830038));
#35659=CARTESIAN_POINT('Ctrl Pts',(0.930521764899172,0.316308422852225,
-6.45246993975933));
#35660=CARTESIAN_POINT('Ctrl Pts',(0.955917571323847,0.188725180169855,
-6.46187158027833));
#35661=CARTESIAN_POINT('Ctrl Pts',(0.97664239769674,-0.0299459612263952,
-6.47808852365388));
#35662=CARTESIAN_POINT('Ctrl Pts',(0.964857697793123,-0.156413988815773,
-6.48728868889742));
#35663=CARTESIAN_POINT('Ctrl Pts',(0.888096285138142,-0.417810720029666,
-6.50742434229249));
#35664=CARTESIAN_POINT('Ctrl Pts',(0.820092045273133,-0.527882040545075,
-6.51678466931517));
#35665=CARTESIAN_POINT('Ctrl Pts',(0.675770062615426,-0.705366515980331,
-6.53366718112217));
#35666=CARTESIAN_POINT('Ctrl Pts',(0.5809664933872,-0.786101245828098,-6.54269728986336));
#35667=CARTESIAN_POINT('Ctrl Pts',(0.334378142358148,-0.924817352612472,
-6.56361671402265));
#35668=CARTESIAN_POINT('Ctrl Pts',(0.200770139829655,-0.95282931152194,
-6.57345534441649));
#35669=CARTESIAN_POINT('Ctrl Pts',(0.0280752756794515,-0.972225368674033,
-6.58627921604608));
#35670=CARTESIAN_POINT('Ctrl Pts',(-0.101993726346509,-0.977915627493418,
-6.59566512298073));
#35671=CARTESIAN_POINT('Ctrl Pts',(-0.37981870565778,-0.901545906814718,
-6.61696907634072));
#35672=CARTESIAN_POINT('Ctrl Pts',(-0.49684242670466,-0.841959929657246,
-6.62647290922221));
#35673=CARTESIAN_POINT('Ctrl Pts',(-0.682085252789105,-0.697218075104707,
-6.64382412759795));
#35674=CARTESIAN_POINT('Ctrl Pts',(-0.77081880044234,-0.606690908795046,
-6.65300493095937));
#35675=CARTESIAN_POINT('Ctrl Pts',(-0.904965977547019,-0.370172044703089,
-6.67309944575452));
#35676=CARTESIAN_POINT('Ctrl Pts',(-0.945851484996125,-0.246693206634984,
-6.68251198105045));
#35677=CARTESIAN_POINT('Ctrl Pts',(-0.978337809142477,0.00697411187024545,
-6.70139690628255));
#35678=CARTESIAN_POINT('Ctrl Pts',(-0.969183713860661,0.134034020754471,
-6.71063891064538));
#35679=CARTESIAN_POINT('Ctrl Pts',(-0.900941041069729,0.378603545282209,
-6.72939002406403));
#35680=CARTESIAN_POINT('Ctrl Pts',(-0.843896455480788,0.493200294182256,
-6.73865852575791));
#35681=CARTESIAN_POINT('Ctrl Pts',(-0.678314757631577,0.709001837100137,
-6.7587576837383));
#35682=CARTESIAN_POINT('Ctrl Pts',(-0.576463604726424,0.787057843739473,
-6.76804744583087));
#35683=CARTESIAN_POINT('Ctrl Pts',(-0.375632597250351,0.901830084169005,
-6.78512094273665));
#35684=CARTESIAN_POINT('Ctrl Pts',(-0.256987402283606,0.943082682135299,
-6.79422521505888));
#35685=CARTESIAN_POINT('Ctrl Pts',(0.0142369621639247,0.981786888990614,
-6.81447980020282));
#35686=CARTESIAN_POINT('Ctrl Pts',(0.144113504802178,0.964140166216503,
-6.82395091889248));
#35687=CARTESIAN_POINT('Ctrl Pts',(0.361268264905602,0.907471666524345,
-6.8405123076895));
#35688=CARTESIAN_POINT('Ctrl Pts',(0.472813840474943,0.855545430902499,
-6.84944174610912));
#35689=CARTESIAN_POINT('Ctrl Pts',(0.668319496067421,0.713344210924143,
-6.86731786265288));
#35690=CARTESIAN_POINT('Ctrl Pts',(0.752078467845626,0.623215502836168,
-6.87624730107246));
#35691=CARTESIAN_POINT('Ctrl Pts',(0.872877916954441,0.43407269491594,-6.89280868986945));
#35692=CARTESIAN_POINT('Ctrl Pts',(0.929670083339895,0.315945758997088,
-6.90227980855905));
#35693=CARTESIAN_POINT('Ctrl Pts',(0.976387595491632,0.0459862332221396,
-6.92253439370301));
#35694=CARTESIAN_POINT('Ctrl Pts',(0.97368458119012,-0.0795970174180683,
-6.9316386660253));
#35695=CARTESIAN_POINT('Ctrl Pts',(0.926350356148606,-0.306015284960221,
-6.94871216293115));
#35696=CARTESIAN_POINT('Ctrl Pts',(0.883460463339687,-0.426956818832671,
-6.95800192502379));
#35697=CARTESIAN_POINT('Ctrl Pts',(0.729151523474463,-0.650957612728575,
-6.97810108300424));
#35698=CARTESIAN_POINT('Ctrl Pts',(0.637696488394232,-0.740525889266283,
-6.98736958469814));
#35699=CARTESIAN_POINT('Ctrl Pts',(0.426036713628733,-0.880780851615593,
-7.00612069811684));
#35700=CARTESIAN_POINT('Ctrl Pts',(0.307973653875435,-0.928625724149746,
-7.0153627024797));
#35701=CARTESIAN_POINT('Ctrl Pts',(0.0566327757125236,-0.975851063730747,
-7.03424762771179));
#35702=CARTESIAN_POINT('Ctrl Pts',(-0.0734360522994339,-0.974986107295992,
-7.0436601630077));
#35703=CARTESIAN_POINT('Ctrl Pts',(-0.339774824632758,-0.920211144507616,
-7.06375467780277));
#35704=CARTESIAN_POINT('Ctrl Pts',(-0.453231709580488,-0.863674912079865,
-7.07293548116414));
#35705=CARTESIAN_POINT('Ctrl Pts',(-0.647993419123852,-0.732020115088863,
-7.09028669953976));
#35706=CARTESIAN_POINT('Ctrl Pts',(-0.740727065661021,-0.639038876328688,
-7.09979053242116));
#35707=CARTESIAN_POINT('Ctrl Pts',(-0.898957001061358,-0.398243650235556,
-7.12109448578108));
#35708=CARTESIAN_POINT('Ctrl Pts',(-0.933606042652205,-0.27274556957179,
-7.1304803927157));
#35709=CARTESIAN_POINT('Ctrl Pts',(-0.968344848134613,-0.102472440362377,
-7.14330426434533));
#35710=CARTESIAN_POINT('Ctrl Pts',(-0.982847457133258,0.0332679092532401,
-7.15314289473918));
#35711=CARTESIAN_POINT('Ctrl Pts',(-0.926827203591237,0.310593898546053,
-7.1740623188985));
#35712=CARTESIAN_POINT('Ctrl Pts',(-0.879218087597563,0.425655557739472,
-7.18309242763976));
#35713=CARTESIAN_POINT('Ctrl Pts',(-0.754815127384698,0.617628152630065,
-7.19997493944684));
#35714=CARTESIAN_POINT('Ctrl Pts',(-0.671041199110333,0.716229375650086,
-7.20933526646956));
#35715=CARTESIAN_POINT('Ctrl Pts',(-0.445996172083125,0.869771882377502,
-7.22947091986463));
#35716=CARTESIAN_POINT('Ctrl Pts',(-0.329306472663791,0.91993716124174,
-7.23867108510816));
#35717=CARTESIAN_POINT('Ctrl Pts',(-0.114883025917202,0.967572988022602,
-7.25488802848372));
#35718=CARTESIAN_POINT('Ctrl Pts',(0.0143196672288365,0.982708868611547,
-7.26428966900275));
#35719=CARTESIAN_POINT('Ctrl Pts',(0.293766255479787,0.932273626548167,
-7.28526472046171));
#35720=CARTESIAN_POINT('Ctrl Pts',(0.414196553987357,0.885421253450072,
-7.29461745814069));
#35721=CARTESIAN_POINT('Ctrl Pts',(0.628885360373169,0.749556298117646,
-7.31338724295661));
#35722=CARTESIAN_POINT('Ctrl Pts',(0.719279850675252,0.662897645454415,
-7.3224705869374));
#35723=CARTESIAN_POINT('Ctrl Pts',(0.866282680323135,0.45295346680244,-7.34139078328843));
#35724=CARTESIAN_POINT('Ctrl Pts',(0.91946836671907,0.33338785413682,-7.35086023113688));
#35725=CARTESIAN_POINT('Ctrl Pts',(0.978663500387982,0.0671324606298182,
-7.37102368552925));
#35726=CARTESIAN_POINT('Ctrl Pts',(0.973003359148487,-0.0591157425322254,
-7.38017228231881));
#35727=CARTESIAN_POINT('Ctrl Pts',(0.934577081667824,-0.287198233874419,
-7.397241369728));
#35728=CARTESIAN_POINT('Ctrl Pts',(0.888335678485908,-0.410441551965415,
-7.40677048447703));
#35729=CARTESIAN_POINT('Ctrl Pts',(0.75436700942129,-0.621641826545463,
-7.42526436347355));
#35730=CARTESIAN_POINT('Ctrl Pts',(0.669643013392061,-0.71106458673487,
-7.43420364628256));
#35731=CARTESIAN_POINT('Ctrl Pts',(0.488174055667406,-0.843864338148941,
-7.45079782955139));
#35732=CARTESIAN_POINT('Ctrl Pts',(0.373982093359788,-0.90783489720384,
-7.4602570382888));
#35733=CARTESIAN_POINT('Ctrl Pts',(0.107697083087079,-0.971515891430713,
-7.4804981812099));
#35734=CARTESIAN_POINT('Ctrl Pts',(-0.0179410017595397,-0.976779967655474,
-7.48961181332377));
#35735=CARTESIAN_POINT('Ctrl Pts',(-0.247146104311301,-0.943791749784903,
-7.50670439725705));
#35736=CARTESIAN_POINT('Ctrl Pts',(-0.370435197427262,-0.90858688114603,
-7.51598709760512));
#35737=CARTESIAN_POINT('Ctrl Pts',(-0.603765305235316,-0.768696128900332,
-7.53608862225344));
#35738=CARTESIAN_POINT('Ctrl Pts',(-0.699024347697691,-0.682989059985113,
-7.54536607093089));
#35739=CARTESIAN_POINT('Ctrl Pts',(-0.852297046956421,-0.480517879540376,
-7.56412016115156));
#35740=CARTESIAN_POINT('Ctrl Pts',(-0.90736036616704,-0.365762213662909,
-7.57335466543725));
#35741=CARTESIAN_POINT('Ctrl Pts',(-0.97030992135747,-0.118015792472393,
-7.59222919003006));
#35742=CARTESIAN_POINT('Ctrl Pts',(-0.977660521401202,0.0119705014249978,
-7.60164988906344));
#35743=CARTESIAN_POINT('Ctrl Pts',(-0.940049641385491,0.279103247274372,
-7.62158934749669));
#35744=CARTESIAN_POINT('Ctrl Pts',(-0.891989890508622,0.394354383619942,
-7.63064363827625));
#35745=CARTESIAN_POINT('Ctrl Pts',(-0.839252972699874,0.48519873794285,
-7.63839979121393));
#35746=CARTESIAN_POINT('Ctrl Pts',(1.208777386421,-0.3711019484798,-5.750484941282));
#35747=CARTESIAN_POINT('Ctrl Pts',(1.121208538256,-0.6563368922743,-5.767385032474));
#35748=CARTESIAN_POINT('Ctrl Pts',(0.7360341133366,-1.160723111217,-5.801185214858));
#35749=CARTESIAN_POINT('Ctrl Pts',(-0.1957638929852,-1.360594219827,-5.851885488434));
#35750=CARTESIAN_POINT('Ctrl Pts',(-1.033397756381,-0.9063363171557,-5.90258576201));
#35751=CARTESIAN_POINT('Ctrl Pts',(-1.374451970489,-0.01661249151435,-5.953286035586));
#35752=CARTESIAN_POINT('Ctrl Pts',(-1.055001304477,0.8811153498779,-6.003986309162));
#35753=CARTESIAN_POINT('Ctrl Pts',(-0.2285671790938,1.355414045495,-6.054686582738));
#35754=CARTESIAN_POINT('Ctrl Pts',(0.707706293492,1.178364498253,-6.105386856314));
#35755=CARTESIAN_POINT('Ctrl Pts',(1.303888502793,0.4350466939165,-6.15608712989));
#35756=CARTESIAN_POINT('Ctrl Pts',(1.273481817004,-0.5173344629195,-6.206787403466));
#35757=CARTESIAN_POINT('Ctrl Pts',(0.6310982509973,-1.221108466328,-6.257487677042));
#35758=CARTESIAN_POINT('Ctrl Pts',(-0.3145621463059,-1.338073817515,-6.308187950618));
#35759=CARTESIAN_POINT('Ctrl Pts',(-1.109058424281,-0.8120223505811,-6.358888224194));
#35760=CARTESIAN_POINT('Ctrl Pts',(-1.370592161421,0.1042497631482,-6.40958849777));
#35761=CARTESIAN_POINT('Ctrl Pts',(-0.973482255877,0.9704242286569,-6.460288771346));
#35762=CARTESIAN_POINT('Ctrl Pts',(-0.1085614893001,1.370257380614,-6.510989044922));
#35763=CARTESIAN_POINT('Ctrl Pts',(0.8085289429002,1.111607770111,-6.561689318498));
#35764=CARTESIAN_POINT('Ctrl Pts',(1.337077500144,0.3187705204298,-6.612389592074));
#35765=CARTESIAN_POINT('Ctrl Pts',(1.223088021562,-0.6272532005374,-6.66308986565));
#35766=CARTESIAN_POINT('Ctrl Pts',(0.5213386151697,-1.271847842471,-6.713790139226));
#35767=CARTESIAN_POINT('Ctrl Pts',(-0.4309421851917,-1.305250826215,-6.764490412802));
#35768=CARTESIAN_POINT('Ctrl Pts',(-1.176131963658,-0.7114102115302,-6.815190686378));
#35769=CARTESIAN_POINT('Ctrl Pts',(-1.35612674083,0.2243014751538,-6.865890959954));
#35770=CARTESIAN_POINT('Ctrl Pts',(-0.8844292854238,1.052224179464,-6.91659123353));
#35771=CARTESIAN_POINT('Ctrl Pts',(0.01228423889075,1.37449625357,-6.967291507106));
#35772=CARTESIAN_POINT('Ctrl Pts',(0.9030946141339,1.03624862196,-7.017991780682));
#35773=CARTESIAN_POINT('Ctrl Pts',(1.359918853029,0.2000272562895,-7.068692054258));
#35774=CARTESIAN_POINT('Ctrl Pts',(1.163229831491,-0.732317124864,-7.119392327834));
#35775=CARTESIAN_POINT('Ctrl Pts',(0.4075412001447,-1.312746877444,-7.17009260141));
#35776=CARTESIAN_POINT('Ctrl Pts',(-0.5439751789721,-1.262318282903,-7.220792874986));
#35777=CARTESIAN_POINT('Ctrl Pts',(-1.23414863257,-0.6053241161137,-7.271493148562));
#35778=CARTESIAN_POINT('Ctrl Pts',(-1.330998526859,0.3427349973485,-7.322193422138));
#35779=CARTESIAN_POINT('Ctrl Pts',(-0.9697720014561,0.8645397432226,-7.355993604522));
#35780=CARTESIAN_POINT('Ctrl Pts',(-0.725376514264,1.035706685623,-7.372893695714));
#35781=CARTESIAN_POINT('Ctrl Pts',(1.110338582265,-0.3408806418612,-5.80993667391));
#35782=CARTESIAN_POINT('Ctrl Pts',(1.02990104942,-0.6028870018931,-5.826836765102));
#35783=CARTESIAN_POINT('Ctrl Pts',(0.6760939467275,-1.066197687173,-5.860636947486));
#35784=CARTESIAN_POINT('Ctrl Pts',(-0.1798215335905,-1.249791958429,-5.911337221062));
#35785=CARTESIAN_POINT('Ctrl Pts',(-0.9492412851402,-0.8325273063098,-5.962037494638));
#35786=CARTESIAN_POINT('Ctrl Pts',(-1.262521180034,-0.01525962553827,-6.012737768214));
#35787=CARTESIAN_POINT('Ctrl Pts',(-0.9690855122368,0.8093602506011,-6.06343804179));
#35788=CARTESIAN_POINT('Ctrl Pts',(-0.2099534293395,1.24503364024,-6.114138315366));
#35789=CARTESIAN_POINT('Ctrl Pts',(0.6500730501767,1.08240241841,-6.164838588942));
#35790=CARTESIAN_POINT('Ctrl Pts',(1.197704166115,0.3996179402166,-6.215538862518));
#35791=CARTESIAN_POINT('Ctrl Pts',(1.169773699538,-0.475204467396,-6.266239136094));
#35792=CARTESIAN_POINT('Ctrl Pts',(0.5797037114969,-1.121665460096,-6.31693940967));
#35793=CARTESIAN_POINT('Ctrl Pts',(-0.2889452528537,-1.22910554267,-6.367639683246));
#35794=CARTESIAN_POINT('Ctrl Pts',(-1.018740400257,-0.7458939550322,-6.418339956822));
#35795=CARTESIAN_POINT('Ctrl Pts',(-1.25897570096,0.09576000967229,-6.469040230398));
#35796=CARTESIAN_POINT('Ctrl Pts',(-0.8942051034311,0.8913961117622,-6.519740503974));
#35797=CARTESIAN_POINT('Ctrl Pts',(-0.09972060320785,1.258668183588,-6.57044077755));
#35798=CARTESIAN_POINT('Ctrl Pts',(0.742685038837,1.021082135854,-6.621141051126));
#35799=CARTESIAN_POINT('Ctrl Pts',(1.228190362067,0.2928109110062,-6.671841324702));
#35800=CARTESIAN_POINT('Ctrl Pts',(1.123483806945,-0.5761717891393,-6.722541598278));
#35801=CARTESIAN_POINT('Ctrl Pts',(0.4788825348239,-1.168272790448,-6.773241871854));
#35802=CARTESIAN_POINT('Ctrl Pts',(-0.3958476890111,-1.198955546455,-6.82394214543));
#35803=CARTESIAN_POINT('Ctrl Pts',(-1.080351693996,-0.6534753334669,-6.874642419006));
#35804=CARTESIAN_POINT('Ctrl Pts',(-1.245688296041,0.2060351101202,-6.925342692582));
#35805=CARTESIAN_POINT('Ctrl Pts',(-0.8124043102742,0.966534547035,-6.976042966158));
#35806=CARTESIAN_POINT('Ctrl Pts',(0.0112838513918,1.262561856849,-7.026743239734));
#35807=CARTESIAN_POINT('Ctrl Pts',(0.8295495967846,0.9518599857224,-7.07744351331));
#35808=CARTESIAN_POINT('Ctrl Pts',(1.249171591254,0.1837377027876,-7.128143786886));
#35809=CARTESIAN_POINT('Ctrl Pts',(1.068500268498,-0.6726796574155,-7.178844060462));
#35810=CARTESIAN_POINT('Ctrl Pts',(0.3743524022424,-1.20584114424,-7.229544334038));
#35811=CARTESIAN_POINT('Ctrl Pts',(-0.499675652268,-1.15951928647,-7.280244607614));
#35812=CARTESIAN_POINT('Ctrl Pts',(-1.133643678633,-0.5560285363098,-7.33094488119));
#35813=CARTESIAN_POINT('Ctrl Pts',(-1.222606440119,0.3148238007455,-7.381645154766));
#35814=CARTESIAN_POINT('Ctrl Pts',(-0.8907969997721,0.7941345061418,-7.415445337151));
#35815=CARTESIAN_POINT('Ctrl Pts',(-0.666304267025,0.9513621828753,-7.432345428343));
#35816=CARTESIAN_POINT('Ctrl Pts',(1.011899778108,-0.3106593352427,-5.869388406539));
#35817=CARTESIAN_POINT('Ctrl Pts',(0.9385935605836,-0.5494371115119,-5.886288497731));
#35818=CARTESIAN_POINT('Ctrl Pts',(0.6161537801183,-0.9716722631302,-5.920088680115));
#35819=CARTESIAN_POINT('Ctrl Pts',(-0.1638791741958,-1.138989697031,-5.970788953691));
#35820=CARTESIAN_POINT('Ctrl Pts',(-0.8650848138998,-0.7587182954638,-6.021489227267));
#35821=CARTESIAN_POINT('Ctrl Pts',(-1.150590389579,-0.0139067595622,-6.072189500843));
#35822=CARTESIAN_POINT('Ctrl Pts',(-0.8831697199965,0.7376051513243,-6.122889774419));
#35823=CARTESIAN_POINT('Ctrl Pts',(-0.1913396795852,1.134653234986,-6.173590047995));
#35824=CARTESIAN_POINT('Ctrl Pts',(0.5924398068615,0.9864403385659,-6.224290321571));
#35825=CARTESIAN_POINT('Ctrl Pts',(1.091519829436,0.3641891865167,-6.274990595147));
#35826=CARTESIAN_POINT('Ctrl Pts',(1.066065582072,-0.4330744718724,-6.325690868723));
#35827=CARTESIAN_POINT('Ctrl Pts',(0.5283091719965,-1.022222453864,-6.376391142299));
#35828=CARTESIAN_POINT('Ctrl Pts',(-0.2633283594015,-1.120137267826,-6.427091415875));
#35829=CARTESIAN_POINT('Ctrl Pts',(-0.9284223762335,-0.6797655594833,-6.477791689451));
#35830=CARTESIAN_POINT('Ctrl Pts',(-1.1473592405,0.0872702561964,-6.528491963027));
#35831=CARTESIAN_POINT('Ctrl Pts',(-0.8149279509853,0.8123679948675,-6.579192236603));
#35832=CARTESIAN_POINT('Ctrl Pts',(-0.09087971711565,1.147078986561,-6.629892510179));
#35833=CARTESIAN_POINT('Ctrl Pts',(0.6768411347738,0.9305565015973,-6.680592783755));
#35834=CARTESIAN_POINT('Ctrl Pts',(1.119303223991,0.2668513015826,-6.731293057331));
#35835=CARTESIAN_POINT('Ctrl Pts',(1.023879592328,-0.5250903777413,-6.781993330907));
#35836=CARTESIAN_POINT('Ctrl Pts',(0.4364264544781,-1.064697738426,-6.832693604483));
#35837=CARTESIAN_POINT('Ctrl Pts',(-0.3607531928305,-1.092660266695,-6.883393878059));
#35838=CARTESIAN_POINT('Ctrl Pts',(-0.9845714243337,-0.5955404554036,-6.934094151635));
#35839=CARTESIAN_POINT('Ctrl Pts',(-1.135249851252,0.1877687450866,-6.984794425211));
#35840=CARTESIAN_POINT('Ctrl Pts',(-0.7403793351246,0.8808449146057,-7.035494698787));
#35841=CARTESIAN_POINT('Ctrl Pts',(0.01028346389286,1.150627460127,-7.086194972363));
#35842=CARTESIAN_POINT('Ctrl Pts',(0.7560045794353,0.8674713494848,-7.136895245939));
#35843=CARTESIAN_POINT('Ctrl Pts',(1.138424329478,0.1674481492858,-7.187595519515));
#35844=CARTESIAN_POINT('Ctrl Pts',(0.9737707055048,-0.613042189967,-7.238295793091));
#35845=CARTESIAN_POINT('Ctrl Pts',(0.34116360434,-1.098935411036,-7.288996066667));
#35846=CARTESIAN_POINT('Ctrl Pts',(-0.455376125564,-1.056720290038,-7.339696340243));
#35847=CARTESIAN_POINT('Ctrl Pts',(-1.033138724697,-0.5067329565058,-7.390396613819));
#35848=CARTESIAN_POINT('Ctrl Pts',(-1.114214353379,0.2869126041425,-7.441096887395));
#35849=CARTESIAN_POINT('Ctrl Pts',(-0.8118219980882,0.7237292690611,-7.474897069779));
#35850=CARTESIAN_POINT('Ctrl Pts',(-0.607232019786,0.867017680128,-7.491797160971));
#35851=CARTESIAN_POINT('Ctrl Pts',(0.9134609739509,-0.2804380286241,-5.928840139167));
#35852=CARTESIAN_POINT('Ctrl Pts',(0.8472860717472,-0.4959872211307,-5.945740230359));
#35853=CARTESIAN_POINT('Ctrl Pts',(0.5562136135091,-0.8771468390869,-5.979540412743));
#35854=CARTESIAN_POINT('Ctrl Pts',(-0.1479368148011,-1.028187435632,-6.030240686319));
#35855=CARTESIAN_POINT('Ctrl Pts',(-0.7809283426593,-0.6849092846179,-6.080940959895));
#35856=CARTESIAN_POINT('Ctrl Pts',(-1.038659599125,-0.01255389358613,-6.131641233471));
#35857=CARTESIAN_POINT('Ctrl Pts',(-0.7972539277561,0.6658500520475,-6.182341507047));
#35858=CARTESIAN_POINT('Ctrl Pts',(-0.1727259298309,1.024272829731,-6.233041780623));
#35859=CARTESIAN_POINT('Ctrl Pts',(0.5348065635462,0.8904782587224,-6.283742054199));
#35860=CARTESIAN_POINT('Ctrl Pts',(0.9853354927582,0.3287604328168,-6.334442327775));
#35861=CARTESIAN_POINT('Ctrl Pts',(0.962357464606,-0.3909444763488,-6.385142601351));
#35862=CARTESIAN_POINT('Ctrl Pts',(0.4769146324961,-0.9227794476316,-6.435842874927));
#35863=CARTESIAN_POINT('Ctrl Pts',(-0.2377114659494,-1.011168992981,-6.486543148503));
#35864=CARTESIAN_POINT('Ctrl Pts',(-0.8381043522096,-0.6136371639345,-6.537243422079));
#35865=CARTESIAN_POINT('Ctrl Pts',(-1.035742780039,0.07878050272052,-6.587943695655));
#35866=CARTESIAN_POINT('Ctrl Pts',(-0.7356507985394,0.7333398779728,-6.638643969231));
#35867=CARTESIAN_POINT('Ctrl Pts',(-0.08203883102345,1.035489789534,-6.689344242807));
#35868=CARTESIAN_POINT('Ctrl Pts',(0.6109972307107,0.8400308673404,-6.740044516383));
#35869=CARTESIAN_POINT('Ctrl Pts',(1.010416085914,0.240891692159,-6.790744789959));
#35870=CARTESIAN_POINT('Ctrl Pts',(0.9242753777111,-0.4740089663433,-6.841445063535));
#35871=CARTESIAN_POINT('Ctrl Pts',(0.3939703741324,-0.9611226864031,-6.892145337111));
#35872=CARTESIAN_POINT('Ctrl Pts',(-0.3256586966498,-0.9863649869346,-6.942845610687));
#35873=CARTESIAN_POINT('Ctrl Pts',(-0.8887911546714,-0.5376055773403,-6.993545884263));
#35874=CARTESIAN_POINT('Ctrl Pts',(-1.024811406463,0.169502380053,-7.044246157839));
#35875=CARTESIAN_POINT('Ctrl Pts',(-0.668354359975,0.7951552821763,-7.094946431415));
#35876=CARTESIAN_POINT('Ctrl Pts',(0.009283076393917,1.038693063406,-7.145646704991));
#35877=CARTESIAN_POINT('Ctrl Pts',(0.682459562086,0.7830827132473,-7.196346978567));
#35878=CARTESIAN_POINT('Ctrl Pts',(1.027677067702,0.151158595784,-7.247047252143));
#35879=CARTESIAN_POINT('Ctrl Pts',(0.8790411425118,-0.5534047225185,-7.297747525719));
#35880=CARTESIAN_POINT('Ctrl Pts',(0.3079748064376,-0.9920296778312,-7.348447799295));
#35881=CARTESIAN_POINT('Ctrl Pts',(-0.41107659886,-0.9539212936056,-7.399148072871));
#35882=CARTESIAN_POINT('Ctrl Pts',(-0.9326337707599,-0.4574373767019,-7.449848346447));
#35883=CARTESIAN_POINT('Ctrl Pts',(-1.005822266638,0.2590014075395,-7.500548620023));
#35884=CARTESIAN_POINT('Ctrl Pts',(-0.7328469964043,0.6533240319803,-7.534348802407));
#35885=CARTESIAN_POINT('Ctrl Pts',(-0.548159772547,0.7826731773806,-7.551248893599));
#35886=CARTESIAN_POINT('',(0.928054415751644,-0.836414325535831,-5.79040924924187));
#35887=CARTESIAN_POINT('Ctrl Pts',(0.92789124572231,-0.836293509745428,
-5.79007519368924));
#35888=CARTESIAN_POINT('Ctrl Pts',(0.864371518669428,-0.90691332511516,
-5.79556091081753));
#35889=CARTESIAN_POINT('Ctrl Pts',(0.792940913081216,-0.970478590785472,
-5.80103199531844));
#35890=CARTESIAN_POINT('Ctrl Pts',(0.637425660624765,-1.07951704358424,
-5.81183551894919));
#35891=CARTESIAN_POINT('Ctrl Pts',(0.554333481303023,-1.1242195195087,-5.81709774994574));
#35892=CARTESIAN_POINT('Ctrl Pts',(0.316929185470185,-1.21890506887434,
-5.83173271154793));
#35893=CARTESIAN_POINT('Ctrl Pts',(0.155475401581182,-1.24969237459365,
-5.84113306986631));
#35894=CARTESIAN_POINT('Ctrl Pts',(-0.199054089558224,-1.2492012766419,
-5.86150526396104));
#35895=CARTESIAN_POINT('Ctrl Pts',(-0.359646947934741,-1.20454904675112,
-5.87065369581061));
#35896=CARTESIAN_POINT('Ctrl Pts',(-0.632160151649209,-1.08893348546595,
-5.88769715376775));
#35897=CARTESIAN_POINT('Ctrl Pts',(-0.767902086473319,-0.99835874169403,
-5.89701866654246));
#35898=CARTESIAN_POINT('Ctrl Pts',(-0.933329311671832,-0.834622917109364,
-5.91030361631294));
#35899=CARTESIAN_POINT('Ctrl Pts',(-0.980121164363449,-0.779260291825079,
-5.91436218117752));
#35900=CARTESIAN_POINT('Ctrl Pts',(-1.06900391284112,-0.65245114369523,
-5.92316811919274));
#35901=CARTESIAN_POINT('Ctrl Pts',(-1.10928952019647,-0.580596899049868,
-5.92788168288861));
#35902=CARTESIAN_POINT('Ctrl Pts',(-1.20570785544617,-0.361601373980931,
-5.94168728141064));
#35903=CARTESIAN_POINT('Ctrl Pts',(-1.24253207170567,-0.205605311439727,
-5.95083527081061));
#35904=CARTESIAN_POINT('Ctrl Pts',(-1.25221879358022,0.0317429523925532,
-5.964337522886));
#35905=CARTESIAN_POINT('Ctrl Pts',(-1.24750844541546,0.111429598253442,
-5.96880751915366));
#35906=CARTESIAN_POINT('Ctrl Pts',(-1.22216876165356,0.272568462527646,
-5.97813844804283));
#35907=CARTESIAN_POINT('Ctrl Pts',(-1.20099175532748,0.353439666303131,
-5.98293973961609));
#35908=CARTESIAN_POINT('Ctrl Pts',(-1.12195753346685,0.567748349892674,
-5.99613650557584));
#35909=CARTESIAN_POINT('Ctrl Pts',(-1.04444831027652,0.706761633037904,
-6.00518390553283));
#35910=CARTESIAN_POINT('Ctrl Pts',(-0.820493665574736,0.95807855509362,
-6.02421369458117));
#35911=CARTESIAN_POINT('Ctrl Pts',(-0.691465108533078,1.04962810774492,
-6.03319175461902));
#35912=CARTESIAN_POINT('Ctrl Pts',(-0.492229169061597,1.15105288157756,
-6.04610966506214));
#35913=CARTESIAN_POINT('Ctrl Pts',(-0.414398218128557,1.18157328874261,
-6.0509144337977));
#35914=CARTESIAN_POINT('Ctrl Pts',(-0.181971563564285,1.24688313303702,
-6.06474168436814));
#35915=CARTESIAN_POINT('Ctrl Pts',(-0.0251387762637779,1.25994099328009,
-6.0734095518453));
#35916=CARTESIAN_POINT('Ctrl Pts',(0.297440616610082,1.22372522263434,-6.09211825370061));
#35917=CARTESIAN_POINT('Ctrl Pts',(0.455350712066313,1.17475757835444,-6.1015560033069));
#35918=CARTESIAN_POINT('Ctrl Pts',(0.666423373946411,1.06043904118231,-6.11522248205187));
#35919=CARTESIAN_POINT('Ctrl Pts',(0.730710728774875,1.01713258649561,-6.11955696212495));
#35920=CARTESIAN_POINT('Ctrl Pts',(0.914149524679502,0.866358631852595,
-6.13311138351778));
#35921=CARTESIAN_POINT('Ctrl Pts',(1.01793347598042,0.741001899059063,-6.14240830870793));
#35922=CARTESIAN_POINT('Ctrl Pts',(1.16083313914051,0.48240175293223,-6.15941888380699));
#35923=CARTESIAN_POINT('Ctrl Pts',(1.22181971482467,0.327451104671911,-6.16855859432356));
#35924=CARTESIAN_POINT('Ctrl Pts',(1.25904048842782,-0.0245884022575979,
-6.18890019477955));
#35925=CARTESIAN_POINT('Ctrl Pts',(1.24527503627133,-0.187976080808616,
-6.19827840885629));
#35926=CARTESIAN_POINT('Ctrl Pts',(1.17601279473243,-0.433788014109638,
-6.21290291514525));
#35927=CARTESIAN_POINT('Ctrl Pts',(1.14016946501633,-0.521266518177868,
-6.21817569961738));
#35928=CARTESIAN_POINT('Ctrl Pts',(1.04771956613206,-0.687695788509239,
-6.22900408748747));
#35929=CARTESIAN_POINT('Ctrl Pts',(0.99175891804555,-0.765569396789959,
-6.23449075487895));
#35930=CARTESIAN_POINT('Ctrl Pts',(0.927917233057705,-0.836264674901695,
-6.23999215811417));
#35931=CARTESIAN_POINT('',(0.720545177924135,-0.649395441962508,-5.95169174984025));
#35932=CARTESIAN_POINT('Ctrl Pts',(0.720108737182204,-0.649004448460025,
-5.95167596829406));
#35933=CARTESIAN_POINT('Ctrl Pts',(0.649924515094261,-0.727158489828415,
-5.95943212123172));
#35934=CARTESIAN_POINT('Ctrl Pts',(0.555079480957704,-0.808380306989316,
-5.96848641201143));
#35935=CARTESIAN_POINT('Ctrl Pts',(0.312518521341791,-0.926442422296025,
-5.98842587044456));
#35936=CARTESIAN_POINT('Ctrl Pts',(0.186587724758989,-0.959486368703343,
-5.99784656947781));
#35937=CARTESIAN_POINT('Ctrl Pts',(-0.0685031170828884,-0.975905812045911,
-6.01672109407051));
#35938=CARTESIAN_POINT('Ctrl Pts',(-0.194639787589624,-0.958865497291628,
-6.02595559835624));
#35939=CARTESIAN_POINT('Ctrl Pts',(-0.434477044399887,-0.875407786476413,
-6.04470968857699));
#35940=CARTESIAN_POINT('Ctrl Pts',(-0.545358094112484,-0.811178668098817,
-6.05398713725455));
#35941=CARTESIAN_POINT('Ctrl Pts',(-0.750315949779591,-0.632280263483006,
-6.07408866190298));
#35942=CARTESIAN_POINT('Ctrl Pts',(-0.821783629703353,-0.525828612563079,
-6.08337136225105));
#35943=CARTESIAN_POINT('Ctrl Pts',(-0.923765700015957,-0.31792753298714,
-6.10046394618437));
#35944=CARTESIAN_POINT('Ctrl Pts',(-0.957455434114764,-0.196776219833828,
-6.10957757829825));
#35945=CARTESIAN_POINT('Ctrl Pts',(-0.978889084396869,0.0761772090825361,
-6.12981872121936));
#35946=CARTESIAN_POINT('Ctrl Pts',(-0.953200947514869,0.204521107671363,
-6.13927792995675));
#35947=CARTESIAN_POINT('Ctrl Pts',(-0.882751937182649,0.418071320821548,
-6.1558721132256));
#35948=CARTESIAN_POINT('Ctrl Pts',(-0.823772560685341,0.526219453912358,
-6.16481139603458));
#35949=CARTESIAN_POINT('Ctrl Pts',(-0.664104034634087,0.718726913669793,
-6.18330527503119));
#35950=CARTESIAN_POINT('Ctrl Pts',(-0.561095305033117,0.800680464223251,
-6.19283438978037));
#35951=CARTESIAN_POINT('Ctrl Pts',(-0.355937239570725,0.907490434889322,
-6.2099034771897));
#35952=CARTESIAN_POINT('Ctrl Pts',(-0.237570247179744,0.951761205301122,
-6.21905207397936));
#35953=CARTESIAN_POINT('Ctrl Pts',(0.0339733113907507,0.977453504160467,
-6.23921552837171));
#35954=CARTESIAN_POINT('Ctrl Pts',(0.164107751673757,0.963681052608347,
-6.24868497622005));
#35955=CARTESIAN_POINT('Ctrl Pts',(0.409123503410246,0.888490152389854,
-6.26760517257095));
#35956=CARTESIAN_POINT('Ctrl Pts',(0.519411539030041,0.829182183637515,
-6.27668851655165));
#35957=CARTESIAN_POINT('Ctrl Pts',(0.714797598489648,0.66677880484457,-6.29545830136734));
#35958=CARTESIAN_POINT('Ctrl Pts',(0.79646597496151,0.566634519196618,-6.30481103904617));
#35959=CARTESIAN_POINT('Ctrl Pts',(0.930521764899155,0.316308422852269,
-6.32578609050498));
#35960=CARTESIAN_POINT('Ctrl Pts',(0.955917571323838,0.188725180169905,
-6.33518773102405));
#35961=CARTESIAN_POINT('Ctrl Pts',(0.976642397696742,-0.0299459612263604,
-6.35140467439967));
#35962=CARTESIAN_POINT('Ctrl Pts',(0.964857697793128,-0.156413988815745,
-6.36060483964335));
#35963=CARTESIAN_POINT('Ctrl Pts',(0.888096285138152,-0.417810720029647,
-6.38074049303855));
#35964=CARTESIAN_POINT('Ctrl Pts',(0.820092045273143,-0.52788204054506,
-6.39010082006124));
#35965=CARTESIAN_POINT('Ctrl Pts',(0.675770062615433,-0.705366515980325,
-6.4069833318683));
#35966=CARTESIAN_POINT('Ctrl Pts',(0.580966493387205,-0.786101245828095,
-6.4160134406095));
#35967=CARTESIAN_POINT('Ctrl Pts',(0.334378142358139,-0.924817352612478,
-6.43693286476891));
#35968=CARTESIAN_POINT('Ctrl Pts',(0.200770139829639,-0.952829311521942,
-6.44677149516289));
#35969=CARTESIAN_POINT('Ctrl Pts',(0.0280752756794855,-0.972225368674028,
-6.45959536679255));
#35970=CARTESIAN_POINT('Ctrl Pts',(-0.101993726346479,-0.977915627493428,
-6.46898127372728));
#35971=CARTESIAN_POINT('Ctrl Pts',(-0.379818705657778,-0.901545906814717,
-6.49028522708722));
#35972=CARTESIAN_POINT('Ctrl Pts',(-0.496842426704654,-0.841959929657249,
-6.49978905996859));
#35973=CARTESIAN_POINT('Ctrl Pts',(-0.682085252789091,-0.697218075104719,
-6.51714027834417));
#35974=CARTESIAN_POINT('Ctrl Pts',(-0.770818800442323,-0.606690908795065,
-6.52632108170549));
#35975=CARTESIAN_POINT('Ctrl Pts',(-0.904965977547005,-0.370172044703121,
-6.54641559650045));
#35976=CARTESIAN_POINT('Ctrl Pts',(-0.945851484996115,-0.24669320663502,
-6.55582813179624));
#35977=CARTESIAN_POINT('Ctrl Pts',(-0.978337809142478,0.00697411187020937,
-6.57471305702824));
#35978=CARTESIAN_POINT('Ctrl Pts',(-0.969183713860666,0.134034020754438,
-6.58395506139111));
#35979=CARTESIAN_POINT('Ctrl Pts',(-0.900941041069741,0.378603545282184,
-6.60270617480985));
#35980=CARTESIAN_POINT('Ctrl Pts',(-0.8438964554808,0.493200294182236,-6.61197467650383));
#35981=CARTESIAN_POINT('Ctrl Pts',(-0.678314757631588,0.709001837100127,
-6.63207383448436));
#35982=CARTESIAN_POINT('Ctrl Pts',(-0.576463604726434,0.787057843739467,
-6.64136359657699));
#35983=CARTESIAN_POINT('Ctrl Pts',(-0.375632597250357,0.901830084169003,
-6.65843709348284));
#35984=CARTESIAN_POINT('Ctrl Pts',(-0.256987402283611,0.943082682135298,
-6.66754136580511));
#35985=CARTESIAN_POINT('Ctrl Pts',(0.0142369621639232,0.981786888990614,
-6.68779595094908));
#35986=CARTESIAN_POINT('Ctrl Pts',(0.144113504802177,0.964140166216503,
-6.69726706963869));
#35987=CARTESIAN_POINT('Ctrl Pts',(0.361268264905602,0.907471666524346,
-6.71382845843568));
#35988=CARTESIAN_POINT('Ctrl Pts',(0.472813840474943,0.855545430902499,
-6.72275789685528));
#35989=CARTESIAN_POINT('Ctrl Pts',(0.668319496067421,0.713344210924142,
-6.74063401339906));
#35990=CARTESIAN_POINT('Ctrl Pts',(0.752078467845626,0.623215502836167,
-6.7495634518187));
#35991=CARTESIAN_POINT('Ctrl Pts',(0.872877916954441,0.43407269491594,-6.76612484061573));
#35992=CARTESIAN_POINT('Ctrl Pts',(0.929670083339896,0.315945758997087,
-6.7755959593054));
#35993=CARTESIAN_POINT('Ctrl Pts',(0.976387595491632,0.045986233222139,
-6.79585054444934));
#35994=CARTESIAN_POINT('Ctrl Pts',(0.97368458119012,-0.0795970174180682,
-6.80495481677156));
#35995=CARTESIAN_POINT('Ctrl Pts',(0.926350356148606,-0.30601528496022,
-6.82202831367734));
#35996=CARTESIAN_POINT('Ctrl Pts',(0.883460463339688,-0.426956818832668,
-6.8313180757699));
#35997=CARTESIAN_POINT('Ctrl Pts',(0.729151523474468,-0.650957612728569,
-6.85141723375034));
#35998=CARTESIAN_POINT('Ctrl Pts',(0.637696488394238,-0.740525889266277,
-6.8606857354443));
#35999=CARTESIAN_POINT('Ctrl Pts',(0.426036713628743,-0.880780851615588,
-6.87943684886301));
#36000=CARTESIAN_POINT('Ctrl Pts',(0.307973653875445,-0.928625724149743,
-6.88867885322587));
#36001=CARTESIAN_POINT('Ctrl Pts',(0.0566327757125344,-0.975851063730746,
-6.90756377845789));
#36002=CARTESIAN_POINT('Ctrl Pts',(-0.0734360522994191,-0.974986107295992,
-6.91697631375371));
#36003=CARTESIAN_POINT('Ctrl Pts',(-0.339774824632742,-0.920211144507622,
-6.93707082854873));
#36004=CARTESIAN_POINT('Ctrl Pts',(-0.453231709580473,-0.863674912079873,
-6.9462516319101));
#36005=CARTESIAN_POINT('Ctrl Pts',(-0.64799341912384,-0.732020115088874,
-6.96360285028577));
#36006=CARTESIAN_POINT('Ctrl Pts',(-0.74072706566101,-0.6390388763287,-6.97310668316723));
#36007=CARTESIAN_POINT('Ctrl Pts',(-0.89895700106135,-0.398243650235574,
-6.99441063652728));
#36008=CARTESIAN_POINT('Ctrl Pts',(-0.933606042652201,-0.272745569571806,
-7.00379654346201));
#36009=CARTESIAN_POINT('Ctrl Pts',(-0.968344848134609,-0.102472440362395,
-7.01662041509172));
#36010=CARTESIAN_POINT('Ctrl Pts',(-0.982847457133263,0.0332679092532288,
-7.02645904548568));
#36011=CARTESIAN_POINT('Ctrl Pts',(-0.926827203591233,0.310593898546063,
-7.04737846964495));
#36012=CARTESIAN_POINT('Ctrl Pts',(-0.879218087597559,0.425655557739481,
-7.0564085783861));
#36013=CARTESIAN_POINT('Ctrl Pts',(-0.75481512738469,0.617628152630076,
-7.07329109019308));
#36014=CARTESIAN_POINT('Ctrl Pts',(-0.671041199110324,0.716229375650094,
-7.08265141721569));
#36015=CARTESIAN_POINT('Ctrl Pts',(-0.445996172083117,0.869771882377507,
-7.10278707061082));
#36016=CARTESIAN_POINT('Ctrl Pts',(-0.329306472663781,0.919937161241744,
-7.11198723585447));
#36017=CARTESIAN_POINT('Ctrl Pts',(-0.114883025917167,0.967572988022609,
-7.12820417923012));
#36018=CARTESIAN_POINT('Ctrl Pts',(0.0143196672288667,0.982708868611544,
-7.13760581974923));
#36019=CARTESIAN_POINT('Ctrl Pts',(0.293766255479796,0.932273626548164,
-7.15858087120812));
#36020=CARTESIAN_POINT('Ctrl Pts',(0.414196553987364,0.885421253450069,
-7.16793360888701));
#36021=CARTESIAN_POINT('Ctrl Pts',(0.628885360373163,0.749556298117649,
-7.18670339370275));
#36022=CARTESIAN_POINT('Ctrl Pts',(0.719279850675244,0.662897645454425,
-7.19578673768343));
#36023=CARTESIAN_POINT('Ctrl Pts',(0.866282680323126,0.452953466802456,
-7.21470693403423));
#36024=CARTESIAN_POINT('Ctrl Pts',(0.919468366719059,0.333387854136846,
-7.22417638188249));
#36025=CARTESIAN_POINT('Ctrl Pts',(0.978663500387979,0.0671324606298572,
-7.24433983627477));
#36026=CARTESIAN_POINT('Ctrl Pts',(0.973003359148489,-0.0591157425321842,
-7.2534884330644));
#36027=CARTESIAN_POINT('Ctrl Pts',(0.934577081667836,-0.287198233874384,
-7.27055752047376));
#36028=CARTESIAN_POINT('Ctrl Pts',(0.888335678485921,-0.410441551965388,
-7.28008663522298));
#36029=CARTESIAN_POINT('Ctrl Pts',(0.754367009421304,-0.621641826545447,
-7.29858051421967));
#36030=CARTESIAN_POINT('Ctrl Pts',(0.669643013392075,-0.711064586734859,
-7.30751979702871));
#36031=CARTESIAN_POINT('Ctrl Pts',(0.488174055667416,-0.843864338148935,
-7.32411398029761));
#36032=CARTESIAN_POINT('Ctrl Pts',(0.373982093359797,-0.907834897203836,
-7.33357318903505));
#36033=CARTESIAN_POINT('Ctrl Pts',(0.107697083087087,-0.971515891430713,
-7.35381433195615));
#36034=CARTESIAN_POINT('Ctrl Pts',(-0.0179410017595324,-0.976779967655474,
-7.36292796406999));
#36035=CARTESIAN_POINT('Ctrl Pts',(-0.247146104311293,-0.943791749784905,
-7.38002054800323));
#36036=CARTESIAN_POINT('Ctrl Pts',(-0.370435197427253,-0.908586881146033,
-7.38930324835126));
#36037=CARTESIAN_POINT('Ctrl Pts',(-0.603765305235306,-0.76869612890034,
-7.40940477299955));
#36038=CARTESIAN_POINT('Ctrl Pts',(-0.699024347697681,-0.682989059985123,
-7.41868222167699));
#36039=CARTESIAN_POINT('Ctrl Pts',(-0.852297046956413,-0.480517879540391,
-7.43743631189764));
#36040=CARTESIAN_POINT('Ctrl Pts',(-0.907360366167034,-0.365762213662926,
-7.44667081618334));
#36041=CARTESIAN_POINT('Ctrl Pts',(-0.970309921357468,-0.118015792472412,
-7.46554534077611));
#36042=CARTESIAN_POINT('Ctrl Pts',(-0.977660521401202,0.0119705014249765,
-7.47496603980946));
#36043=CARTESIAN_POINT('Ctrl Pts',(-0.940049634066545,0.2791032992575,-7.49490550212285));
#36044=CARTESIAN_POINT('Ctrl Pts',(-0.891989855331675,0.394354468850662,
-7.50395979577473));
#36045=CARTESIAN_POINT('Ctrl Pts',(-0.839252914313109,0.48519883851959,
-7.51171595054694));
#36046=CARTESIAN_POINT('',(0.928537702599,-0.8368498878844,-5.790033670893));
#36047=CARTESIAN_POINT('Ctrl Pts',(-0.8352478720641,0.4641308339706,-4.478818448186));
#36048=CARTESIAN_POINT('Ctrl Pts',(-0.7257270174981,0.6612240973944,-4.495718539378));
#36049=CARTESIAN_POINT('Ctrl Pts',(-0.3618043599731,0.973579871545,-4.529518721762));
#36050=CARTESIAN_POINT('Ctrl Pts',(0.3583616355052,0.9750034062319,-4.580218995338));
#36051=CARTESIAN_POINT('Ctrl Pts',(0.9062041683878,0.5076847542727,-4.630919268914));
#36052=CARTESIAN_POINT('Ctrl Pts',(1.018596427125,-0.203550194661,-4.68161954249));
#36053=CARTESIAN_POINT('Ctrl Pts',(0.6414900337905,-0.8169826520078,-4.732319816066));
#36054=CARTESIAN_POINT('Ctrl Pts',(-0.0438848651729,-1.037806916131,-4.783020089642));
#36055=CARTESIAN_POINT('Ctrl Pts',(-0.7081712873547,-0.759909874548,-4.833720363218));
#36056=CARTESIAN_POINT('Ctrl Pts',(-1.032142960739,-0.1168347725255,-4.884420636794));
#36057=CARTESIAN_POINT('Ctrl Pts',(-0.8601141737781,0.5823856809165,-4.93512091037));
#36058=CARTESIAN_POINT('Ctrl Pts',(-0.2747540081207,1.00173834442,-4.985821183946));
#36059=CARTESIAN_POINT('Ctrl Pts',(0.4426403116802,0.9397015632025,-5.036521457522));
#36060=CARTESIAN_POINT('Ctrl Pts',(0.9473220285466,0.4260873717732,-5.087221731098));
#36061=CARTESIAN_POINT('Ctrl Pts',(0.9967642879194,-0.2922848411075,-5.137922004674));
#36062=CARTESIAN_POINT('Ctrl Pts',(0.5672074110512,-0.8701983836261,-5.18862227825));
#36063=CARTESIAN_POINT('Ctrl Pts',(-0.1349232962637,-1.029934550421,-5.239322551826));
#36064=CARTESIAN_POINT('Ctrl Pts',(-0.7722160642937,-0.694731476232,-5.290022825402));
#36065=CARTESIAN_POINT('Ctrl Pts',(-1.038417259008,-0.02567236295293,-5.340723098978));
#36066=CARTESIAN_POINT('Ctrl Pts',(-0.8056028125943,0.6557237088569,-5.391423372554));
#36067=CARTESIAN_POINT('Ctrl Pts',(-0.1856526550803,1.022009082971,-5.44212364613));
#36068=CARTESIAN_POINT('Ctrl Pts',(0.5235136417157,0.897163831801,-5.492823919706));
#36069=CARTESIAN_POINT('Ctrl Pts',(0.9811033264056,0.3411828488149,-5.543524193282));
#36070=CARTESIAN_POINT('Ctrl Pts',(0.9672198151093,-0.3787549404562,-5.594224466858));
#36071=CARTESIAN_POINT('Ctrl Pts',(0.4885348785918,-0.9166805035943,-5.644924740434));
#36072=CARTESIAN_POINT('Ctrl Pts',(-0.2249174616962,-1.014091510121,-5.69562501401));
#36073=CARTESIAN_POINT('Ctrl Pts',(-0.8302848782164,-0.6241767463422,-5.746325287586));
#36074=CARTESIAN_POINT('Ctrl Pts',(-1.036655225136,0.0656888176107,-5.797025561162));
#36075=CARTESIAN_POINT('Ctrl Pts',(-0.74485777085,0.7239868909991,-5.847725834738));
#36076=CARTESIAN_POINT('Ctrl Pts',(-0.09511182443393,1.034371840274,-5.898426108314));
#36077=CARTESIAN_POINT('Ctrl Pts',(0.6003253513746,0.8476787581516,-5.94912638189));
#36078=CARTESIAN_POINT('Ctrl Pts',(1.007330257735,0.2536542052052,-5.999826655466));
#36079=CARTESIAN_POINT('Ctrl Pts',(0.9300475649187,-0.4623545048573,-6.050526929042));
#36080=CARTESIAN_POINT('Ctrl Pts',(0.5810918409035,-0.7913465001737,-6.084327111426));
#36081=CARTESIAN_POINT('Ctrl Pts',(0.3735576354296,-0.8794948162679,-6.101227202618));
#36082=CARTESIAN_POINT('Ctrl Pts',(-0.9252580684986,0.5141477318691,-4.538270180814));
#36083=CARTESIAN_POINT('Ctrl Pts',(-0.8039347371316,0.7324806822769,-4.555170272006));
#36084=CARTESIAN_POINT('Ctrl Pts',(-0.4007940809903,1.078497367792,-4.58897045439));
#36085=CARTESIAN_POINT('Ctrl Pts',(0.3969803525175,1.080074309199,-4.639670727966));
#36086=CARTESIAN_POINT('Ctrl Pts',(1.003860945417,0.5623952252446,-4.690371001542));
#36087=CARTESIAN_POINT('Ctrl Pts',(1.128365116827,-0.225485710594,-4.741071275118));
#36088=CARTESIAN_POINT('Ctrl Pts',(0.7106199841722,-0.9050245033555,-4.791771548694));
#36089=CARTESIAN_POINT('Ctrl Pts',(-0.04861410240514,-1.1496458175,-4.84247182227));
#36090=CARTESIAN_POINT('Ctrl Pts',(-0.7844871198351,-0.8418012978826,-4.893172095846));
#36091=CARTESIAN_POINT('Ctrl Pts',(-1.143371487925,-0.1294254311517,-4.943872369422));
#36092=CARTESIAN_POINT('Ctrl Pts',(-0.9528040785683,0.6451462712671,-4.994572642998));
#36093=CARTESIAN_POINT('Ctrl Pts',(-0.3043627782466,1.109690328703,-5.045272916574));
#36094=CARTESIAN_POINT('Ctrl Pts',(0.4903412909185,1.040968175334,-5.09597319015));
#36095=CARTESIAN_POINT('Ctrl Pts',(1.049409857475,0.4720045291995,-5.146673463726));
#36096=CARTESIAN_POINT('Ctrl Pts',(1.104180244733,-0.323782815353,-5.197373737302));
#36097=CARTESIAN_POINT('Ctrl Pts',(0.6283323204288,-0.9639750097833,-5.248074010878));
#36098=CARTESIAN_POINT('Ctrl Pts',(-0.1494632583593,-1.140925089037,-5.298774284454));
#36099=CARTESIAN_POINT('Ctrl Pts',(-0.8554336598862,-0.7695989721411,-5.34947455803));
#36100=CARTESIAN_POINT('Ctrl Pts',(-1.150321933764,-0.02843893621772,-5.400174831606));
#36101=CARTESIAN_POINT('Ctrl Pts',(-0.8924183195055,0.7263875462816,-5.450875105182));
#36102=CARTESIAN_POINT('Ctrl Pts',(-0.2056594488852,1.132145536343,-5.501575378758));
#36103=CARTESIAN_POINT('Ctrl Pts',(0.5799299072375,0.9938463801022,-5.552275652334));
#36104=CARTESIAN_POINT('Ctrl Pts',(1.086831585149,0.3779502998543,-5.60297592591));
#36105=CARTESIAN_POINT('Ctrl Pts',(1.071451922086,-0.4195713348838,-5.653676199486));
#36106=CARTESIAN_POINT('Ctrl Pts',(0.5411816698712,-1.015466259243,-5.704376473062));
#36107=CARTESIAN_POINT('Ctrl Pts',(-0.2491556137298,-1.123374729009,-5.755076746638));
#36108=CARTESIAN_POINT('Ctrl Pts',(-0.919760239345,-0.6914409363236,-5.805777020214));
#36109=CARTESIAN_POINT('Ctrl Pts',(-1.148370014925,0.072767750194,-5.85647729379));
#36110=CARTESIAN_POINT('Ctrl Pts',(-0.8251271094647,0.8020070865056,-5.907177567366));
#36111=CARTESIAN_POINT('Ctrl Pts',(-0.1053615171142,1.145840561887,-5.957877840942));
#36112=CARTESIAN_POINT('Ctrl Pts',(0.6650192040728,0.9390285647018,-6.008578114518));
#36113=CARTESIAN_POINT('Ctrl Pts',(1.115884852611,0.2809891624084,-6.059278388094));
#36114=CARTESIAN_POINT('Ctrl Pts',(1.030273817282,-0.5121799772668,-6.10997866167));
#36115=CARTESIAN_POINT('Ctrl Pts',(0.6437130010352,-0.8766256805353,-6.143778844054));
#36116=CARTESIAN_POINT('Ctrl Pts',(0.4138139440886,-0.9742732692555,-6.160678935246));
#36117=CARTESIAN_POINT('Ctrl Pts',(-1.015268264933,0.5641646297676,-4.597721913443));
#36118=CARTESIAN_POINT('Ctrl Pts',(-0.882142456765,0.8037372671594,-4.614622004635));
#36119=CARTESIAN_POINT('Ctrl Pts',(-0.4397838020076,1.183414864038,-4.648422187019));
#36120=CARTESIAN_POINT('Ctrl Pts',(0.4355990695298,1.185145212166,-4.699122460595));
#36121=CARTESIAN_POINT('Ctrl Pts',(1.101517722446,0.6171056962164,-4.749822734171));
#36122=CARTESIAN_POINT('Ctrl Pts',(1.238133806529,-0.2474212265271,-4.800523007747));
#36123=CARTESIAN_POINT('Ctrl Pts',(0.7797499345539,-0.9930663547032,-4.851223281323));
#36124=CARTESIAN_POINT('Ctrl Pts',(-0.05334333963738,-1.261484718868,-4.901923554899));
#36125=CARTESIAN_POINT('Ctrl Pts',(-0.8608029523155,-0.9236927212173,-4.952623828475));
#36126=CARTESIAN_POINT('Ctrl Pts',(-1.254600015111,-0.1420160897778,-5.003324102051));
#36127=CARTESIAN_POINT('Ctrl Pts',(-1.045493983358,0.7079068616178,-5.054024375627));
#36128=CARTESIAN_POINT('Ctrl Pts',(-0.3339715483725,1.217642312985,-5.104724649203));
#36129=CARTESIAN_POINT('Ctrl Pts',(0.5380422701567,1.142234787465,-5.155424922779));
#36130=CARTESIAN_POINT('Ctrl Pts',(1.151497686404,0.5179216866258,-5.206125196355));
#36131=CARTESIAN_POINT('Ctrl Pts',(1.211596201547,-0.3552807895985,-5.256825469931));
#36132=CARTESIAN_POINT('Ctrl Pts',(0.6894572298064,-1.05775163594,-5.307525743507));
#36133=CARTESIAN_POINT('Ctrl Pts',(-0.164003220455,-1.251915627652,-5.358226017083));
#36134=CARTESIAN_POINT('Ctrl Pts',(-0.9386512554787,-0.8444664680501,-5.408926290659));
#36135=CARTESIAN_POINT('Ctrl Pts',(-1.262226608521,-0.03120550948252,-5.459626564235));
#36136=CARTESIAN_POINT('Ctrl Pts',(-0.9792338264167,0.7970513837064,-5.510326837811));
#36137=CARTESIAN_POINT('Ctrl Pts',(-0.2256662426901,1.242281989715,-5.561027111387));
#36138=CARTESIAN_POINT('Ctrl Pts',(0.6363461727594,1.090528928403,-5.611727384963));
#36139=CARTESIAN_POINT('Ctrl Pts',(1.192559843892,0.4147177508937,-5.662427658539));
#36140=CARTESIAN_POINT('Ctrl Pts',(1.175684029063,-0.4603877293114,-5.713127932115));
#36141=CARTESIAN_POINT('Ctrl Pts',(0.5938284611506,-1.114252014892,-5.763828205691));
#36142=CARTESIAN_POINT('Ctrl Pts',(-0.2733937657633,-1.232657947897,-5.814528479267));
#36143=CARTESIAN_POINT('Ctrl Pts',(-1.009235600474,-0.758705126305,-5.865228752843));
#36144=CARTESIAN_POINT('Ctrl Pts',(-1.260084804714,0.0798466827773,-5.915929026419));
#36145=CARTESIAN_POINT('Ctrl Pts',(-0.9053964480795,0.8800272820121,-5.966629299995));
#36146=CARTESIAN_POINT('Ctrl Pts',(-0.1156112097945,1.2573092835,-6.017329573571));
#36147=CARTESIAN_POINT('Ctrl Pts',(0.729713056771,1.030378371252,-6.068029847147));
#36148=CARTESIAN_POINT('Ctrl Pts',(1.224439447487,0.3083241196116,-6.118730120723));
#36149=CARTESIAN_POINT('Ctrl Pts',(1.130500069646,-0.5620054496762,-6.169430394299));
#36150=CARTESIAN_POINT('Ctrl Pts',(0.7063341611668,-0.9619048608968,-6.203230576683));
#36151=CARTESIAN_POINT('Ctrl Pts',(0.4540702527476,-1.069051722243,-6.220130667875));
#36152=CARTESIAN_POINT('Ctrl Pts',(-1.105278461367,0.6141815276661,-4.657173646071));
#36153=CARTESIAN_POINT('Ctrl Pts',(-0.9603501763984,0.8749938520419,-4.674073737263));
#36154=CARTESIAN_POINT('Ctrl Pts',(-0.4787735230248,1.288332360285,-4.707873919647));
#36155=CARTESIAN_POINT('Ctrl Pts',(0.4742177865421,1.290216115133,-4.758574193223));
#36156=CARTESIAN_POINT('Ctrl Pts',(1.199174499476,0.6718161671883,-4.809274466799));
#36157=CARTESIAN_POINT('Ctrl Pts',(1.347902496231,-0.2693567424601,-4.859974740375));
#36158=CARTESIAN_POINT('Ctrl Pts',(0.8488798849356,-1.081108206051,-4.910675013951));
#36159=CARTESIAN_POINT('Ctrl Pts',(-0.05807257686961,-1.373323620236,-4.961375287527));
#36160=CARTESIAN_POINT('Ctrl Pts',(-0.9371187847959,-1.005584144552,-5.012075561103));
#36161=CARTESIAN_POINT('Ctrl Pts',(-1.365828542296,-0.154606748404,-5.062775834679));
#36162=CARTESIAN_POINT('Ctrl Pts',(-1.138183888149,0.7706674519685,-5.113476108255));
#36163=CARTESIAN_POINT('Ctrl Pts',(-0.3635803184984,1.325594297268,-5.164176381831));
#36164=CARTESIAN_POINT('Ctrl Pts',(0.585743249395,1.243501399596,-5.214876655407));
#36165=CARTESIAN_POINT('Ctrl Pts',(1.253585515332,0.563838844052,-5.265576928983));
#36166=CARTESIAN_POINT('Ctrl Pts',(1.319012158361,-0.386778763844,-5.316277202559));
#36167=CARTESIAN_POINT('Ctrl Pts',(0.7505821391841,-1.151528262098,-5.366977476135));
#36168=CARTESIAN_POINT('Ctrl Pts',(-0.1785431825506,-1.362906166268,-5.417677749711));
#36169=CARTESIAN_POINT('Ctrl Pts',(-1.021868851071,-0.9193339639592,-5.468378023287));
#36170=CARTESIAN_POINT('Ctrl Pts',(-1.374131283277,-0.03397208274731,-5.519078296863));
#36171=CARTESIAN_POINT('Ctrl Pts',(-1.066049333328,0.8677152211312,-5.569778570439));
#36172=CARTESIAN_POINT('Ctrl Pts',(-0.245673036495,1.352418443088,-5.620478844015));
#36173=CARTESIAN_POINT('Ctrl Pts',(0.6927624382813,1.187211476704,-5.671179117591));
#36174=CARTESIAN_POINT('Ctrl Pts',(1.298288102635,0.4514852019331,-5.721879391167));
#36175=CARTESIAN_POINT('Ctrl Pts',(1.27991613604,-0.501204123739,-5.772579664743));
#36176=CARTESIAN_POINT('Ctrl Pts',(0.64647525243,-1.213037770542,-5.823279938319));
#36177=CARTESIAN_POINT('Ctrl Pts',(-0.2976319177969,-1.341941166785,-5.873980211895));
#36178=CARTESIAN_POINT('Ctrl Pts',(-1.098710961602,-0.8259693162864,-5.924680485471));
#36179=CARTESIAN_POINT('Ctrl Pts',(-1.371799594503,0.0869256153606,-5.975380759047));
#36180=CARTESIAN_POINT('Ctrl Pts',(-0.9856657866942,0.9580474775185,-6.026081032623));
#36181=CARTESIAN_POINT('Ctrl Pts',(-0.1258609024749,1.368778005114,-6.076781306199));
#36182=CARTESIAN_POINT('Ctrl Pts',(0.7944069094692,1.121728177802,-6.127481579775));
#36183=CARTESIAN_POINT('Ctrl Pts',(1.332994042363,0.3356590768148,-6.178181853351));
#36184=CARTESIAN_POINT('Ctrl Pts',(1.23072632201,-0.6118309220856,-6.228882126927));
#36185=CARTESIAN_POINT('Ctrl Pts',(0.7689553212985,-1.047184041258,-6.262682309311));
#36186=CARTESIAN_POINT('Ctrl Pts',(0.4943265614066,-1.16383017523,-6.279582400503));
#36187=CARTESIAN_POINT('',(-0.733992718634193,1.01100376434735,-4.67964967483772));
#36188=CARTESIAN_POINT('Ctrl Pts',(0.927912398543726,-0.83631111477366,
-5.79009102008202));
#36189=CARTESIAN_POINT('Ctrl Pts',(0.984303033291466,-0.773842119781296,
-5.78531766274095));
#36190=CARTESIAN_POINT('Ctrl Pts',(1.03452888871054,-0.705774985620509,
-5.78052678031108));
#36191=CARTESIAN_POINT('Ctrl Pts',(1.11910171243664,-0.562755852325079,
-5.7709425432084));
#36192=CARTESIAN_POINT('Ctrl Pts',(1.15345589545556,-0.488641509593253,
-5.76615705971969));
#36193=CARTESIAN_POINT('Ctrl Pts',(1.2328253590026,-0.258988426301621,-5.75209196287802));
#36194=CARTESIAN_POINT('Ctrl Pts',(1.25550476406795,-0.0965386012710815,
-5.74304269490003));
#36195=CARTESIAN_POINT('Ctrl Pts',(1.24008869637804,0.217686148614962,-5.72515730558005));
#36196=CARTESIAN_POINT('Ctrl Pts',(1.20565282886093,0.363340832817156,-5.71651231673383));
#36197=CARTESIAN_POINT('Ctrl Pts',(1.11110647759861,0.577496730223301,-5.70304565128118));
#36198=CARTESIAN_POINT('Ctrl Pts',(1.06992642102215,0.650107404166377,-5.69832635750262));
#36199=CARTESIAN_POINT('Ctrl Pts',(0.944063252293379,0.828999426635918,
-5.68592634355134));
#36200=CARTESIAN_POINT('Ctrl Pts',(0.84822354797798,0.927636413561337,-5.67824551246648));
#36201=CARTESIAN_POINT('Ctrl Pts',(0.679323690640051,1.05191055815686,-5.66607914245479));
#36202=CARTESIAN_POINT('Ctrl Pts',(0.616172065736563,1.08999231276497,-5.66177019919714));
#36203=CARTESIAN_POINT('Ctrl Pts',(0.474958779197421,1.15866792269239,-5.65272926901884));
#36204=CARTESIAN_POINT('Ctrl Pts',(0.396590390856506,1.18748335031581,-5.64800681550211));
#36205=CARTESIAN_POINT('Ctrl Pts',(0.184681379976035,1.24274328140347,-5.63559226990401));
#36206=CARTESIAN_POINT('Ctrl Pts',(0.0475448526567326,1.25607405418918,
-5.62790341017278));
#36207=CARTESIAN_POINT('Ctrl Pts',(-0.158747611208275,1.2419016812461,-5.6159160019639));
#36208=CARTESIAN_POINT('Ctrl Pts',(-0.228471459127974,1.23091869803186,
-5.61178760980794));
#36209=CARTESIAN_POINT('Ctrl Pts',(-0.37786010424686,1.19392417930954,-5.60291288201398));
#36210=CARTESIAN_POINT('Ctrl Pts',(-0.456479036779733,1.16581410705845,
-5.5981855228565));
#36211=CARTESIAN_POINT('Ctrl Pts',(-0.656372372773785,1.07153597232633,
-5.58565226936609));
#36212=CARTESIAN_POINT('Ctrl Pts',(-0.771729822950002,0.992397318754269,
-5.57785612991876));
#36213=CARTESIAN_POINT('Ctrl Pts',(-0.918751299420806,0.850173600540487,
-5.56601005253366));
#36214=CARTESIAN_POINT('Ctrl Pts',(-0.962497177798991,0.800278747680704,
-5.56212531860281));
#36215=CARTESIAN_POINT('Ctrl Pts',(-1.09809180565154,0.61740790137033,-5.54896687865545));
#36216=CARTESIAN_POINT('Ctrl Pts',(-1.16861654247585,0.469121166842377,
-5.5399082273327));
#36217=CARTESIAN_POINT('Ctrl Pts',(-1.24801622685103,0.165592839605571,
-5.52205386008585));
#36218=CARTESIAN_POINT('Ctrl Pts',(-1.25875502195331,0.0181262164159631,
-5.51350071541098));
#36219=CARTESIAN_POINT('Ctrl Pts',(-1.23412796614598,-0.212041691723438,
-5.50018362657264));
#36220=CARTESIAN_POINT('Ctrl Pts',(-1.21699110135391,-0.293754636185665,
-5.49546390692046));
#36221=CARTESIAN_POINT('Ctrl Pts',(-1.15170546985013,-0.501892996514001,
-5.48309930106408));
#36222=CARTESIAN_POINT('Ctrl Pts',(-1.09079317412563,-0.624488677481668,
-5.47545453135052));
#36223=CARTESIAN_POINT('Ctrl Pts',(-0.968198663043609,-0.794116403411135,
-5.46331411522335));
#36224=CARTESIAN_POINT('Ctrl Pts',(-0.919561652350412,-0.849819592194169,
-5.4589932792317));
#36225=CARTESIAN_POINT('Ctrl Pts',(-0.80589568154704,-0.958454179706746,
-5.44994066352474));
#36226=CARTESIAN_POINT('Ctrl Pts',(-0.740060554789238,-1.00980945165427,
-5.44521815995594));
#36227=CARTESIAN_POINT('Ctrl Pts',(-0.555034233455757,-1.12715793426829,
-5.43279722929553));
#36228=CARTESIAN_POINT('Ctrl Pts',(-0.428397427015014,-1.1817312067325,
-5.42510206701911));
#36229=CARTESIAN_POINT('Ctrl Pts',(-0.22749238542697,-1.23116591024906,
-5.41310748150614));
#36230=CARTESIAN_POINT('Ctrl Pts',(-0.15772833475297,-1.24196725387437,
-5.40897845163875));
#36231=CARTESIAN_POINT('Ctrl Pts',(-0.00416229030680703,-1.25228372556958,
-5.40010325075728));
#36232=CARTESIAN_POINT('Ctrl Pts',(0.0792836668379041,-1.24948344807876,
-5.3953759861892));
#36233=CARTESIAN_POINT('Ctrl Pts',(0.298384557946442,-1.22064573563774,
-5.38284396242009));
#36234=CARTESIAN_POINT('Ctrl Pts',(0.432359677060051,-1.18045766426295,
-5.37504886840061));
#36235=CARTESIAN_POINT('Ctrl Pts',(0.61574593083661,-1.08984333067015,-5.36320281722287));
#36236=CARTESIAN_POINT('Ctrl Pts',(0.672636691788199,-1.05565545308738,
-5.35931712106376));
#36237=CARTESIAN_POINT('Ctrl Pts',(0.857545353227488,-0.922828082187633,
-5.34615798430428));
#36238=CARTESIAN_POINT('Ctrl Pts',(0.969925654675212,-0.803108263823864,
-5.33709947109674));
#36239=CARTESIAN_POINT('Ctrl Pts',(1.1379918851384,-0.538406840277865,-5.31925596605873));
#36240=CARTESIAN_POINT('Ctrl Pts',(1.19315942434402,-0.401401621351654,
-5.31071209962985));
#36241=CARTESIAN_POINT('Ctrl Pts',(1.25564597191947,-0.0988166122171712,
-5.29293654959551));
#36242=CARTESIAN_POINT('Ctrl Pts',(1.25758497619127,0.0650321485579314,
-5.2839084079254));
#36243=CARTESIAN_POINT('Ctrl Pts',(1.20050647840116,0.384378933204612,-5.26539551259472));
#36244=CARTESIAN_POINT('Ctrl Pts',(1.14101560074235,0.535904535944659,-5.25596917053691));
#36245=CARTESIAN_POINT('Ctrl Pts',(0.965647218495031,0.808142751845912,
-5.23747522437915));
#36246=CARTESIAN_POINT('Ctrl Pts',(0.853232698893263,0.926317530602951,
-5.22848854524482));
#36247=CARTESIAN_POINT('Ctrl Pts',(0.665665056433136,1.06018710828656,-5.21524692817884));
#36248=CARTESIAN_POINT('Ctrl Pts',(0.605133327280159,1.096025339646,-5.21115359580372));
#36249=CARTESIAN_POINT('Ctrl Pts',(0.408216854292134,1.19043053073033,-5.19844162651996));
#36250=CARTESIAN_POINT('Ctrl Pts',(0.263350841531732,1.22982241083698,-5.19008170770061));
#36251=CARTESIAN_POINT('Ctrl Pts',(0.0335648761284514,1.25151546350363,
-5.17699740304561));
#36252=CARTESIAN_POINT('Ctrl Pts',(-0.0500459869614035,1.25124308234069,
-5.17226878091564));
#36253=CARTESIAN_POINT('Ctrl Pts',(-0.208300430875469,1.23477564161633,
-5.16310870515926));
#36254=CARTESIAN_POINT('Ctrl Pts',(-0.282555681669839,1.22002648641904,
-5.15868427269107));
#36255=CARTESIAN_POINT('Ctrl Pts',(-0.478021396008706,1.16165000945984,
-5.1468570784796));
#36256=CARTESIAN_POINT('Ctrl Pts',(-0.594870942271891,1.10574458873467,
-5.13960585708624));
#36257=CARTESIAN_POINT('Ctrl Pts',(-0.769702136393781,0.987344731511731,
-5.12763966246471));
#36258=CARTESIAN_POINT('Ctrl Pts',(-0.834035584823648,0.933969583596118,
-5.1229190306032));
#36259=CARTESIAN_POINT('Ctrl Pts',(-1.00316562863355,0.762421362002899,
-5.10908186946697));
#36260=CARTESIAN_POINT('Ctrl Pts',(-1.08914063838115,0.632938430723606,
-5.10009921704361));
#36261=CARTESIAN_POINT('Ctrl Pts',(-1.2131050151576,0.337887886550823,-5.08189295875165));
#36262=CARTESIAN_POINT('Ctrl Pts',(-1.24730782029891,0.177086377376111,
-5.07282160821827));
#36263=CARTESIAN_POINT('Ctrl Pts',(-1.25074524640195,-0.0525654262503107,
-5.05953660300103));
#36264=CARTESIAN_POINT('Ctrl Pts',(-1.24602919303149,-0.120557140971158,
-5.05554602046806));
#36265=CARTESIAN_POINT('Ctrl Pts',(-1.21508721635405,-0.320625864321934,
-5.04383769939516));
#36266=CARTESIAN_POINT('Ctrl Pts',(-1.1729085372533,-0.449710654044156,
-5.03626377490034));
#36267=CARTESIAN_POINT('Ctrl Pts',(-1.07460800163896,-0.64232073157027,
-5.02400074382649));
#36268=CARTESIAN_POINT('Ctrl Pts',(-1.03012914619204,-0.711980852772414,
-5.0193208046912));
#36269=CARTESIAN_POINT('Ctrl Pts',(-0.933790186201797,-0.834123228088677,
-5.01035222997315));
#36270=CARTESIAN_POINT('Ctrl Pts',(-0.883594995637419,-0.887213249032559,
-5.00607834253427));
#36271=CARTESIAN_POINT('Ctrl Pts',(-0.731433976648951,-1.02139932002522,
-4.99432409243777));
#36272=CARTESIAN_POINT('Ctrl Pts',(-0.62070490816199,-1.09160845194591,
-4.98699183988445));
#36273=CARTESIAN_POINT('Ctrl Pts',(-0.426016127082591,-1.17722388431758,
-4.97493746758731));
#36274=CARTESIAN_POINT('Ctrl Pts',(-0.34657396684484,-1.20328297600705,
-4.97021303498468));
#36275=CARTESIAN_POINT('Ctrl Pts',(-0.115622456347341,-1.25415584664946,
-4.95661561497873));
#36276=CARTESIAN_POINT('Ctrl Pts',(0.0368662084239702,-1.25895993925486,
-4.94779868968955));
#36277=CARTESIAN_POINT('Ctrl Pts',(0.351529427749479,-1.20922475185803,
-4.92967766044937));
#36278=CARTESIAN_POINT('Ctrl Pts',(0.506265466721744,-1.15363052022541,
-4.92060437148523));
#36279=CARTESIAN_POINT('Ctrl Pts',(0.703078291497398,-1.03574785005439,
-4.90733154021851));
#36280=CARTESIAN_POINT('Ctrl Pts',(0.758179953516722,-0.996113189942167,
-4.90335736874744));
#36281=CARTESIAN_POINT('Ctrl Pts',(0.912123771114747,-0.864496136601418,
-4.89164540875892));
#36282=CARTESIAN_POINT('Ctrl Pts',(0.999929842988508,-0.7603863800361,-4.88405121228351));
#36283=CARTESIAN_POINT('Ctrl Pts',(1.11206374453665,-0.575053273671101,
-4.87176636926986));
#36284=CARTESIAN_POINT('Ctrl Pts',(1.14784383137581,-0.500556456462736,
-4.86708591728025));
#36285=CARTESIAN_POINT('Ctrl Pts',(1.20078259690565,-0.354683630615294,
-4.85813714691876));
#36286=CARTESIAN_POINT('Ctrl Pts',(1.21939666046203,-0.284428275635072,
-4.85388508961195));
#36287=CARTESIAN_POINT('Ctrl Pts',(1.25344291010085,-0.0846396456922892,
-4.84214457874379));
#36288=CARTESIAN_POINT('Ctrl Pts',(1.25488801214753,0.0466453714559938,
-4.83480351565871));
#36289=CARTESIAN_POINT('Ctrl Pts',(1.22518787451642,0.257424044102171,-4.82273908138619));
#36290=CARTESIAN_POINT('Ctrl Pts',(1.20553022119135,0.338691454838772,-4.818014011537));
#36291=CARTESIAN_POINT('Ctrl Pts',(1.12765509076486,0.560590428986372,-4.80449001523444));
#36292=CARTESIAN_POINT('Ctrl Pts',(1.05233406416851,0.691764352615165,-4.79574497940039));
#36293=CARTESIAN_POINT('Ctrl Pts',(0.845984873630827,0.932814566662742,
-4.77769025112686));
#36294=CARTESIAN_POINT('Ctrl Pts',(0.717528423108332,1.03553798967812,-4.76861321402929));
#36295=CARTESIAN_POINT('Ctrl Pts',(0.512820905109634,1.14205854283913,-4.75526850807405));
#36296=CARTESIAN_POINT('Ctrl Pts',(0.448974984218303,1.168624308156,-4.75122133408201));
#36297=CARTESIAN_POINT('Ctrl Pts',(0.255819218906257,1.23026373995105,-4.73950657944032));
#36298=CARTESIAN_POINT('Ctrl Pts',(0.122213546647829,1.25010859997572,-4.73197931948863));
#36299=CARTESIAN_POINT('Ctrl Pts',(-0.138351662392057,1.24808378903057,
-4.7172051080251));
#36300=CARTESIAN_POINT('Ctrl Pts',(-0.265779189758412,1.2280555759047,-4.70990241740329));
#36301=CARTESIAN_POINT('Ctrl Pts',(-0.511890143544524,1.147781009971,-4.69478191057141));
#36302=CARTESIAN_POINT('Ctrl Pts',(-0.628863836674227,1.08723957239584,
-4.68733470794919));
#36303=CARTESIAN_POINT('Ctrl Pts',(-0.733904641412792,1.01085195669132,
-4.6799679321611));
#36304=CARTESIAN_POINT('',(-0.569874894399988,0.784947385849281,-4.51836716849296));
#36305=CARTESIAN_POINT('',(-0.5698749570781,0.784947471679,-4.518367177796));
#36306=CARTESIAN_POINT('Ctrl Pts',(-0.569529321306653,0.784474167360507,
-4.51835139123805));
#36307=CARTESIAN_POINT('Ctrl Pts',(-0.484636911634744,0.846338237939427,
-4.52610754601023));
#36308=CARTESIAN_POINT('Ctrl Pts',(-0.37498449428145,0.906078691512917,
-4.53516183966203));
#36309=CARTESIAN_POINT('Ctrl Pts',(-0.11318517611704,0.971160390418818,
-4.5551013019754));
#36310=CARTESIAN_POINT('Ctrl Pts',(0.0168632307072555,0.977315047570584,
-4.56452200100877));
#36311=CARTESIAN_POINT('Ctrl Pts',(0.269797863995055,0.940369046501477,
-4.58339652560156));
#36312=CARTESIAN_POINT('Ctrl Pts',(0.389640305530924,0.897489900285439,
-4.59263102988726));
#36313=CARTESIAN_POINT('Ctrl Pts',(0.606900163119466,0.766016505526524,
-4.61138512010795));
#36314=CARTESIAN_POINT('Ctrl Pts',(0.702014304273948,0.680148659476006,
-4.6206625687854));
#36315=CARTESIAN_POINT('Ctrl Pts',(0.865323843694871,0.462565672761053,
-4.64076409343374));
#36316=CARTESIAN_POINT('Ctrl Pts',(0.913111224941757,0.343586895448389,
-4.65004679378182));
#36317=CARTESIAN_POINT('Ctrl Pts',(0.969666070452139,0.119032334142445,
-4.6671393777151));
#36318=CARTESIAN_POINT('Ctrl Pts',(0.977445580061419,-0.00647510823700896,
-4.67625300982894));
#36319=CARTESIAN_POINT('Ctrl Pts',(0.941692548896792,-0.277924360370873,
-4.69649415275001));
#36320=CARTESIAN_POINT('Ctrl Pts',(0.889895690185106,-0.398128861572077,
-4.7059533614874));
#36321=CARTESIAN_POINT('Ctrl Pts',(0.776609403954005,-0.592378633632003,
-4.72254754475627));
#36322=CARTESIAN_POINT('Ctrl Pts',(0.696444599699847,-0.685910391350884,
-4.73148682756529));
#36323=CARTESIAN_POINT('Ctrl Pts',(0.500258893832878,-0.841037207495618,
-4.74998070656194));
#36324=CARTESIAN_POINT('Ctrl Pts',(0.382468956290842,-0.89979700188057,
-4.75950982131112));
#36325=CARTESIAN_POINT('Ctrl Pts',(0.1595943127922,-0.961644353830413,-4.77657890872045));
#36326=CARTESIAN_POINT('Ctrl Pts',(0.0346117104224662,-0.980352509949183,
-4.78572750551008));
#36327=CARTESIAN_POINT('Ctrl Pts',(-0.236343379195985,-0.949058136150452,
-4.80589095990238));
#36328=CARTESIAN_POINT('Ctrl Pts',(-0.360775378580037,-0.908544798855134,
-4.81536040775067));
#36329=CARTESIAN_POINT('Ctrl Pts',(-0.584818511226714,-0.784081692722731,
-4.8342806041015));
#36330=CARTESIAN_POINT('Ctrl Pts',(-0.680375181353441,-0.703150803980066,
-4.8433639480822));
#36331=CARTESIAN_POINT('Ctrl Pts',(-0.837749469773749,-0.503691778064571,
-4.862133732898));
#36332=CARTESIAN_POINT('Ctrl Pts',(-0.896825536918335,-0.388763017720261,
-4.87148647057693));
#36333=CARTESIAN_POINT('Ctrl Pts',(-0.975938218374797,-0.116044677743486,
-4.89246152203582));
#36334=CARTESIAN_POINT('Ctrl Pts',(-0.974268306023393,0.0140308472029995,
-4.9018631625549));
#36335=CARTESIAN_POINT('Ctrl Pts',(-0.949101604663953,0.232235392643118,
-4.91808010593055));
#36336=CARTESIAN_POINT('Ctrl Pts',(-0.911294498982234,0.353494057958645,
-4.92728027117415));
#36337=CARTESIAN_POINT('Ctrl Pts',(-0.781891247636173,0.593234259224568,
-4.9474159245693));
#36338=CARTESIAN_POINT('Ctrl Pts',(-0.692498942409303,0.686771888047523,
-4.95677625159203));
#36339=CARTESIAN_POINT('Ctrl Pts',(-0.514446522986004,0.830392602557005,
-4.97365876339911));
#36340=CARTESIAN_POINT('Ctrl Pts',(-0.404935910777075,0.889665186064197,
-4.98268887214038));
#36341=CARTESIAN_POINT('Ctrl Pts',(-0.134905330150612,0.974113150346353,
-5.00360829629978));
#36342=CARTESIAN_POINT('Ctrl Pts',(0.00160707428446136,0.973750359822927,
-5.01344692669361));
#36343=CARTESIAN_POINT('Ctrl Pts',(0.17456279736015,0.956837613378721,-5.02627079832319));
#36344=CARTESIAN_POINT('Ctrl Pts',(0.302975074330211,0.935375752863385,
-5.03565670525779));
#36345=CARTESIAN_POINT('Ctrl Pts',(0.558866320705606,0.80294190751462,-5.05696065861763));
#36346=CARTESIAN_POINT('Ctrl Pts',(0.660953880687902,0.720339425358643,
-5.06646449149907));
#36347=CARTESIAN_POINT('Ctrl Pts',(0.812076348801616,0.540264139141331,
-5.08381570987471));
#36348=CARTESIAN_POINT('Ctrl Pts',(0.880061774681646,0.433274456521516,
-5.09299651323606));
#36349=CARTESIAN_POINT('Ctrl Pts',(0.962132946141087,0.174042975000017,
-5.11309102803108));
#36350=CARTESIAN_POINT('Ctrl Pts',(0.976467507927318,0.0447635547179919,
-5.12250356332691));
#36351=CARTESIAN_POINT('Ctrl Pts',(0.955533483765514,-0.210117273055868,
-5.14138848855896));
#36352=CARTESIAN_POINT('Ctrl Pts',(0.920176570954098,-0.332501531122724,
-5.15063049292185));
#36353=CARTESIAN_POINT('Ctrl Pts',(0.802602751105272,-0.557551995693596,
-5.1693816063406));
#36354=CARTESIAN_POINT('Ctrl Pts',(0.72299050396223,-0.657793652245647,
-5.17865010803458));
#36355=CARTESIAN_POINT('Ctrl Pts',(0.516180264657057,-0.834477351286836,
-5.19874926601507));
#36356=CARTESIAN_POINT('Ctrl Pts',(0.400332533119837,-0.889665217872399,
-5.20803902810765));
#36357=CARTESIAN_POINT('Ctrl Pts',(0.180035963144122,-0.960200187879757,
-5.22511252501343));
#36358=CARTESIAN_POINT('Ctrl Pts',(0.0554083971430044,-0.975898242544961,
-5.23421679733565));
#36359=CARTESIAN_POINT('Ctrl Pts',(-0.217938297569029,-0.957398080705504,
-5.25447138247956));
#36360=CARTESIAN_POINT('Ctrl Pts',(-0.341312967821625,-0.913148629947773,
-5.2639425011692));
#36361=CARTESIAN_POINT('Ctrl Pts',(-0.541952151862903,-0.81259304074293,
-5.28050388996625));
#36362=CARTESIAN_POINT('Ctrl Pts',(-0.640272812359039,-0.738621444203258,
-5.2894333283859));
#36363=CARTESIAN_POINT('Ctrl Pts',(-0.801962028794448,-0.558898753313217,
-5.30730944492977));
#36364=CARTESIAN_POINT('Ctrl Pts',(-0.865164262002853,-0.453332531951947,
-5.31623888334945));
#36365=CARTESIAN_POINT('Ctrl Pts',(-0.94402364854212,-0.24321659764972,
-5.33280027214652));
#36366=CARTESIAN_POINT('Ctrl Pts',(-0.975029766934588,-0.115866906741197,
-5.34227139083619));
#36367=CARTESIAN_POINT('Ctrl Pts',(-0.964630825541228,0.157907696748253,
-5.36252597598007));
#36368=CARTESIAN_POINT('Ctrl Pts',(-0.935891024457683,0.280188042516797,
-5.37163024830224));
#36369=CARTESIAN_POINT('Ctrl Pts',(-0.842541035141802,0.491828162134418,
-5.38870374520798));
#36370=CARTESIAN_POINT('Ctrl Pts',(-0.775456087044577,0.601217408678344,
-5.39799350730056));
#36371=CARTESIAN_POINT('Ctrl Pts',(-0.577968766812459,0.788263827879977,
-5.41809266528101));
#36372=CARTESIAN_POINT('Ctrl Pts',(-0.469898014985202,0.856872954117074,
-5.42736116697496));
#36373=CARTESIAN_POINT('Ctrl Pts',(-0.233713821582721,0.950084227599802,
-5.44611228039366));
#36374=CARTESIAN_POINT('Ctrl Pts',(-0.108285830905306,0.972351626655509,
-5.45535428475652));
#36375=CARTESIAN_POINT('Ctrl Pts',(0.147382057119426,0.966318321832296,
-5.47423920998856));
#36376=CARTESIAN_POINT('Ctrl Pts',(0.274432011617768,0.938444369260617,
-5.48365174528442));
#36377=CARTESIAN_POINT('Ctrl Pts',(0.523575091539715,0.829520708270321,
-5.50374626007947));
#36378=CARTESIAN_POINT('Ctrl Pts',(0.622807399176721,0.750642577966373,
-5.51292706344084));
#36379=CARTESIAN_POINT('Ctrl Pts',(0.785960420543068,0.581390692617458,
-5.5302782818165));
#36380=CARTESIAN_POINT('Ctrl Pts',(0.857348683054851,0.471169297520886,
-5.53978211469793));
#36381=CARTESIAN_POINT('Ctrl Pts',(0.962088321082959,0.202750480014222,
-5.56108606805791));
#36382=CARTESIAN_POINT('Ctrl Pts',(0.969902954400321,0.0727918102781827,
-5.57047197499261));
#36383=CARTESIAN_POINT('Ctrl Pts',(0.968501283832613,-0.100983212255705,
-5.58329584662227));
#36384=CARTESIAN_POINT('Ctrl Pts',(0.954480930335872,-0.236774220313617,
-5.59313447701619));
#36385=CARTESIAN_POINT('Ctrl Pts',(0.842056053068111,-0.496405921220234,
-5.6140539011755));
#36386=CARTESIAN_POINT('Ctrl Pts',(0.771576711542555,-0.599062999690933,
-5.62308400991669));
#36387=CARTESIAN_POINT('Ctrl Pts',(0.609997938988816,-0.760994695040378,
-5.63996652172369));
#36388=CARTESIAN_POINT('Ctrl Pts',(0.507563614314365,-0.840035705712443,
-5.64932684874635));
#36389=CARTESIAN_POINT('Ctrl Pts',(0.255525233332945,-0.943463071888587,
-5.66946250214136));
#36390=CARTESIAN_POINT('Ctrl Pts',(0.130958452487746,-0.968285607294544,
-5.67866266738487));
#36391=CARTESIAN_POINT('Ctrl Pts',(-0.0886831345802765,-0.970325150882858,
-5.69487961076042));
#36392=CARTESIAN_POINT('Ctrl Pts',(-0.218210781695994,-0.95828274954155,
-5.70428125127945));
#36393=CARTESIAN_POINT('Ctrl Pts',(-0.481077340281045,-0.850880320776053,
-5.72525630273845));
#36394=CARTESIAN_POINT('Ctrl Pts',(-0.589143120265961,-0.780025618322459,
-5.73460904041748));
#36395=CARTESIAN_POINT('Ctrl Pts',(-0.770913413302387,-0.602514688393457,
-5.75337882523339));
#36396=CARTESIAN_POINT('Ctrl Pts',(-0.841327391289039,-0.498963939181004,
-5.76246216921414));
#36397=CARTESIAN_POINT('Ctrl Pts',(-0.941495735081668,-0.263055709192838,
-5.78138236556507));
#36398=CARTESIAN_POINT('Ctrl Pts',(-0.968675143304467,-0.135048159656995,
-5.79085181341341));
#36399=CARTESIAN_POINT('Ctrl Pts',(-0.971251168838686,0.137695974128068,
-5.81101526780577));
#36400=CARTESIAN_POINT('Ctrl Pts',(-0.939480613937675,0.260012276564834,
-5.82016386459539));
#36401=CARTESIAN_POINT('Ctrl Pts',(-0.854498309521635,0.475131335678766,
-5.83723295200468));
#36402=CARTESIAN_POINT('Ctrl Pts',(-0.783656704497048,0.586075690288896,
-5.84676206675381));
#36403=CARTESIAN_POINT('Ctrl Pts',(-0.608725574238593,0.76482764115973,
-5.86525594575038));
#36404=CARTESIAN_POINT('Ctrl Pts',(-0.5072691743685,0.834693115239862,-5.87419522855934));
#36405=CARTESIAN_POINT('Ctrl Pts',(-0.302165962186486,0.926885462785104,
-5.89078941182814));
#36406=CARTESIAN_POINT('Ctrl Pts',(-0.177173705923729,0.965730958737603,
-5.90024862056551));
#36407=CARTESIAN_POINT('Ctrl Pts',(0.0965315452820945,0.97268877333576,
-5.9204897634866));
#36408=CARTESIAN_POINT('Ctrl Pts',(0.220521063650604,0.951730763001616,
-5.9296033956005));
#36409=CARTESIAN_POINT('Ctrl Pts',(0.437868240623847,0.871834541464922,
-5.94669597953381));
#36410=CARTESIAN_POINT('Ctrl Pts',(0.551150726807566,0.811779053944625,
-5.95597867988191));
#36411=CARTESIAN_POINT('Ctrl Pts',(0.750318872098352,0.626456600703946,
-5.97608020453024));
#36412=CARTESIAN_POINT('Ctrl Pts',(0.825688954935265,0.52282582609488,-5.98535765320768));
#36413=CARTESIAN_POINT('Ctrl Pts',(0.93354317436394,0.292924615571315,-6.00411174342834));
#36414=CARTESIAN_POINT('Ctrl Pts',(0.963558721675803,0.169231855504197,
-6.01334624771403));
#36415=CARTESIAN_POINT('Ctrl Pts',(0.973653321148666,-0.0861874757391061,
-6.03222077230681));
#36416=CARTESIAN_POINT('Ctrl Pts',(0.953832746458542,-0.214863863398643,
-6.04164147134018));
#36417=CARTESIAN_POINT('Ctrl Pts',(0.861533526071293,-0.46835022618067,
-6.06158092977344));
#36418=CARTESIAN_POINT('Ctrl Pts',(0.79057401337535,-0.571099005449627,
-6.07063522055322));
#36419=CARTESIAN_POINT('Ctrl Pts',(0.720111076156533,-0.649001853220507,
-6.07839137349091));
#36420=CARTESIAN_POINT('Ctrl Pts',(-1.105278461367,0.6141815276661,-4.190476523559));
#36421=CARTESIAN_POINT('Ctrl Pts',(-0.9603501763984,0.8749938520419,-4.207376614751));
#36422=CARTESIAN_POINT('Ctrl Pts',(-0.4787735230248,1.288332360285,-4.241176797135));
#36423=CARTESIAN_POINT('Ctrl Pts',(0.4742177865421,1.290216115133,-4.291877070711));
#36424=CARTESIAN_POINT('Ctrl Pts',(1.199174499476,0.6718161671883,-4.342577344287));
#36425=CARTESIAN_POINT('Ctrl Pts',(1.347902496231,-0.2693567424601,-4.393277617863));
#36426=CARTESIAN_POINT('Ctrl Pts',(0.8488798849356,-1.081108206051,-4.443977891439));
#36427=CARTESIAN_POINT('Ctrl Pts',(-0.05807257686962,-1.373323620236,-4.494678165015));
#36428=CARTESIAN_POINT('Ctrl Pts',(-0.9371187847959,-1.005584144552,-4.545378438591));
#36429=CARTESIAN_POINT('Ctrl Pts',(-1.365828542296,-0.154606748404,-4.596078712167));
#36430=CARTESIAN_POINT('Ctrl Pts',(-1.138183888149,0.7706674519685,-4.646778985743));
#36431=CARTESIAN_POINT('Ctrl Pts',(-0.3635803184984,1.325594297268,-4.697479259319));
#36432=CARTESIAN_POINT('Ctrl Pts',(0.585743249395,1.243501399596,-4.748179532895));
#36433=CARTESIAN_POINT('Ctrl Pts',(1.253585515332,0.563838844052,-4.798879806471));
#36434=CARTESIAN_POINT('Ctrl Pts',(1.319012158361,-0.386778763844,-4.849580080047));
#36435=CARTESIAN_POINT('Ctrl Pts',(0.7505821391841,-1.151528262098,-4.900280353623));
#36436=CARTESIAN_POINT('Ctrl Pts',(-0.1785431825506,-1.362906166268,-4.950980627199));
#36437=CARTESIAN_POINT('Ctrl Pts',(-1.021868851071,-0.9193339639592,-5.001680900775));
#36438=CARTESIAN_POINT('Ctrl Pts',(-1.374131283277,-0.03397208274731,-5.052381174351));
#36439=CARTESIAN_POINT('Ctrl Pts',(-1.066049333328,0.8677152211312,-5.103081447927));
#36440=CARTESIAN_POINT('Ctrl Pts',(-0.245673036495,1.352418443088,-5.153781721503));
#36441=CARTESIAN_POINT('Ctrl Pts',(0.6927624382813,1.187211476704,-5.204481995079));
#36442=CARTESIAN_POINT('Ctrl Pts',(1.298288102635,0.4514852019331,-5.255182268655));
#36443=CARTESIAN_POINT('Ctrl Pts',(1.27991613604,-0.501204123739,-5.305882542231));
#36444=CARTESIAN_POINT('Ctrl Pts',(0.64647525243,-1.213037770542,-5.356582815807));
#36445=CARTESIAN_POINT('Ctrl Pts',(-0.2976319177969,-1.341941166785,-5.407283089383));
#36446=CARTESIAN_POINT('Ctrl Pts',(-1.098710961602,-0.8259693162864,-5.457983362959));
#36447=CARTESIAN_POINT('Ctrl Pts',(-1.371799594503,0.08692561536059,-5.508683636535));
#36448=CARTESIAN_POINT('Ctrl Pts',(-0.9856657866942,0.9580474775185,-5.559383910111));
#36449=CARTESIAN_POINT('Ctrl Pts',(-0.1258609024748,1.368778005114,-5.610084183687));
#36450=CARTESIAN_POINT('Ctrl Pts',(0.7944069094692,1.121728177802,-5.660784457263));
#36451=CARTESIAN_POINT('Ctrl Pts',(1.332994042363,0.3356590768148,-5.711484730839));
#36452=CARTESIAN_POINT('Ctrl Pts',(1.23072632201,-0.6118309220856,-5.762185004415));
#36453=CARTESIAN_POINT('Ctrl Pts',(0.7689553212985,-1.047184041258,-5.795985186799));
#36454=CARTESIAN_POINT('Ctrl Pts',(0.4943265614066,-1.16383017523,-5.812885277991));
#36455=CARTESIAN_POINT('Ctrl Pts',(-1.015268264933,0.5641646297676,-4.249928256187));
#36456=CARTESIAN_POINT('Ctrl Pts',(-0.882142456765,0.8037372671594,-4.266828347379));
#36457=CARTESIAN_POINT('Ctrl Pts',(-0.4397838020076,1.183414864038,-4.300628529763));
#36458=CARTESIAN_POINT('Ctrl Pts',(0.4355990695298,1.185145212166,-4.351328803339));
#36459=CARTESIAN_POINT('Ctrl Pts',(1.101517722446,0.6171056962164,-4.402029076915));
#36460=CARTESIAN_POINT('Ctrl Pts',(1.238133806529,-0.2474212265271,-4.452729350491));
#36461=CARTESIAN_POINT('Ctrl Pts',(0.7797499345539,-0.9930663547032,-4.503429624067));
#36462=CARTESIAN_POINT('Ctrl Pts',(-0.05334333963738,-1.261484718868,-4.554129897643));
#36463=CARTESIAN_POINT('Ctrl Pts',(-0.8608029523155,-0.9236927212173,-4.604830171219));
#36464=CARTESIAN_POINT('Ctrl Pts',(-1.254600015111,-0.1420160897778,-4.655530444795));
#36465=CARTESIAN_POINT('Ctrl Pts',(-1.045493983358,0.7079068616178,-4.706230718371));
#36466=CARTESIAN_POINT('Ctrl Pts',(-0.3339715483725,1.217642312985,-4.756930991947));
#36467=CARTESIAN_POINT('Ctrl Pts',(0.5380422701567,1.142234787465,-4.807631265523));
#36468=CARTESIAN_POINT('Ctrl Pts',(1.151497686404,0.5179216866258,-4.858331539099));
#36469=CARTESIAN_POINT('Ctrl Pts',(1.211596201547,-0.3552807895985,-4.909031812675));
#36470=CARTESIAN_POINT('Ctrl Pts',(0.6894572298064,-1.05775163594,-4.959732086251));
#36471=CARTESIAN_POINT('Ctrl Pts',(-0.164003220455,-1.251915627652,-5.010432359827));
#36472=CARTESIAN_POINT('Ctrl Pts',(-0.9386512554787,-0.8444664680501,-5.061132633403));
#36473=CARTESIAN_POINT('Ctrl Pts',(-1.262226608521,-0.03120550948252,-5.111832906979));
#36474=CARTESIAN_POINT('Ctrl Pts',(-0.9792338264167,0.7970513837064,-5.162533180555));
#36475=CARTESIAN_POINT('Ctrl Pts',(-0.2256662426901,1.242281989715,-5.213233454131));
#36476=CARTESIAN_POINT('Ctrl Pts',(0.6363461727594,1.090528928403,-5.263933727707));
#36477=CARTESIAN_POINT('Ctrl Pts',(1.192559843892,0.4147177508937,-5.314634001283));
#36478=CARTESIAN_POINT('Ctrl Pts',(1.175684029063,-0.4603877293114,-5.365334274859));
#36479=CARTESIAN_POINT('Ctrl Pts',(0.5938284611506,-1.114252014892,-5.416034548435));
#36480=CARTESIAN_POINT('Ctrl Pts',(-0.2733937657633,-1.232657947897,-5.466734822011));
#36481=CARTESIAN_POINT('Ctrl Pts',(-1.009235600474,-0.758705126305,-5.517435095587));
#36482=CARTESIAN_POINT('Ctrl Pts',(-1.260084804714,0.07984668277729,-5.568135369163));
#36483=CARTESIAN_POINT('Ctrl Pts',(-0.9053964480795,0.8800272820121,-5.618835642739));
#36484=CARTESIAN_POINT('Ctrl Pts',(-0.1156112097945,1.2573092835,-5.669535916315));
#36485=CARTESIAN_POINT('Ctrl Pts',(0.729713056771,1.030378371252,-5.720236189891));
#36486=CARTESIAN_POINT('Ctrl Pts',(1.224439447487,0.3083241196116,-5.770936463467));
#36487=CARTESIAN_POINT('Ctrl Pts',(1.130500069646,-0.5620054496762,-5.821636737043));
#36488=CARTESIAN_POINT('Ctrl Pts',(0.7063341611668,-0.9619048608968,-5.855436919427));
#36489=CARTESIAN_POINT('Ctrl Pts',(0.4540702527476,-1.069051722243,-5.872337010619));
#36490=CARTESIAN_POINT('Ctrl Pts',(-0.9252580684986,0.5141477318691,-4.309379988816));
#36491=CARTESIAN_POINT('Ctrl Pts',(-0.8039347371316,0.7324806822769,-4.326280080008));
#36492=CARTESIAN_POINT('Ctrl Pts',(-0.4007940809904,1.078497367792,-4.360080262392));
#36493=CARTESIAN_POINT('Ctrl Pts',(0.3969803525175,1.080074309199,-4.410780535968));
#36494=CARTESIAN_POINT('Ctrl Pts',(1.003860945417,0.5623952252446,-4.461480809544));
#36495=CARTESIAN_POINT('Ctrl Pts',(1.128365116827,-0.225485710594,-4.51218108312));
#36496=CARTESIAN_POINT('Ctrl Pts',(0.7106199841722,-0.9050245033555,-4.562881356696));
#36497=CARTESIAN_POINT('Ctrl Pts',(-0.04861410240515,-1.1496458175,-4.613581630272));
#36498=CARTESIAN_POINT('Ctrl Pts',(-0.7844871198351,-0.8418012978826,-4.664281903848));
#36499=CARTESIAN_POINT('Ctrl Pts',(-1.143371487925,-0.1294254311517,-4.714982177424));
#36500=CARTESIAN_POINT('Ctrl Pts',(-0.9528040785683,0.6451462712671,-4.765682451));
#36501=CARTESIAN_POINT('Ctrl Pts',(-0.3043627782466,1.109690328703,-4.816382724576));
#36502=CARTESIAN_POINT('Ctrl Pts',(0.4903412909185,1.040968175334,-4.867082998152));
#36503=CARTESIAN_POINT('Ctrl Pts',(1.049409857475,0.4720045291995,-4.917783271728));
#36504=CARTESIAN_POINT('Ctrl Pts',(1.104180244733,-0.323782815353,-4.968483545304));
#36505=CARTESIAN_POINT('Ctrl Pts',(0.6283323204288,-0.9639750097833,-5.01918381888));
#36506=CARTESIAN_POINT('Ctrl Pts',(-0.1494632583593,-1.140925089037,-5.069884092456));
#36507=CARTESIAN_POINT('Ctrl Pts',(-0.8554336598862,-0.7695989721411,-5.120584366032));
#36508=CARTESIAN_POINT('Ctrl Pts',(-1.150321933764,-0.02843893621772,-5.171284639608));
#36509=CARTESIAN_POINT('Ctrl Pts',(-0.8924183195055,0.7263875462816,-5.221984913184));
#36510=CARTESIAN_POINT('Ctrl Pts',(-0.2056594488852,1.132145536343,-5.27268518676));
#36511=CARTESIAN_POINT('Ctrl Pts',(0.5799299072375,0.9938463801022,-5.323385460336));
#36512=CARTESIAN_POINT('Ctrl Pts',(1.086831585149,0.3779502998543,-5.374085733912));
#36513=CARTESIAN_POINT('Ctrl Pts',(1.071451922086,-0.4195713348838,-5.424786007488));
#36514=CARTESIAN_POINT('Ctrl Pts',(0.5411816698712,-1.015466259243,-5.475486281064));
#36515=CARTESIAN_POINT('Ctrl Pts',(-0.2491556137298,-1.123374729009,-5.52618655464));
#36516=CARTESIAN_POINT('Ctrl Pts',(-0.919760239345,-0.6914409363236,-5.576886828216));
#36517=CARTESIAN_POINT('Ctrl Pts',(-1.148370014925,0.072767750194,-5.627587101792));
#36518=CARTESIAN_POINT('Ctrl Pts',(-0.8251271094647,0.8020070865056,-5.678287375368));
#36519=CARTESIAN_POINT('Ctrl Pts',(-0.1053615171142,1.145840561887,-5.728987648944));
#36520=CARTESIAN_POINT('Ctrl Pts',(0.6650192040728,0.9390285647018,-5.77968792252));
#36521=CARTESIAN_POINT('Ctrl Pts',(1.115884852611,0.2809891624084,-5.830388196096));
#36522=CARTESIAN_POINT('Ctrl Pts',(1.030273817282,-0.5121799772668,-5.881088469672));
#36523=CARTESIAN_POINT('Ctrl Pts',(0.6437130010352,-0.8766256805353,-5.914888652056));
#36524=CARTESIAN_POINT('Ctrl Pts',(0.4138139440886,-0.9742732692555,-5.931788743248));
#36525=CARTESIAN_POINT('Ctrl Pts',(-0.8352478720641,0.4641308339706,-4.368831721444));
#36526=CARTESIAN_POINT('Ctrl Pts',(-0.7257270174981,0.6612240973944,-4.385731812636));
#36527=CARTESIAN_POINT('Ctrl Pts',(-0.3618043599731,0.973579871545,-4.41953199502));
#36528=CARTESIAN_POINT('Ctrl Pts',(0.3583616355052,0.9750034062319,-4.470232268596));
#36529=CARTESIAN_POINT('Ctrl Pts',(0.9062041683879,0.5076847542727,-4.520932542172));
#36530=CARTESIAN_POINT('Ctrl Pts',(1.018596427125,-0.203550194661,-4.571632815748));
#36531=CARTESIAN_POINT('Ctrl Pts',(0.6414900337905,-0.8169826520078,-4.622333089324));
#36532=CARTESIAN_POINT('Ctrl Pts',(-0.04388486517291,-1.037806916131,-4.6730333629));
#36533=CARTESIAN_POINT('Ctrl Pts',(-0.7081712873547,-0.759909874548,-4.723733636476));
#36534=CARTESIAN_POINT('Ctrl Pts',(-1.032142960739,-0.1168347725255,-4.774433910052));
#36535=CARTESIAN_POINT('Ctrl Pts',(-0.8601141737781,0.5823856809165,-4.825134183628));
#36536=CARTESIAN_POINT('Ctrl Pts',(-0.2747540081207,1.00173834442,-4.875834457204));
#36537=CARTESIAN_POINT('Ctrl Pts',(0.4426403116802,0.9397015632025,-4.92653473078));
#36538=CARTESIAN_POINT('Ctrl Pts',(0.9473220285466,0.4260873717732,-4.977235004356));
#36539=CARTESIAN_POINT('Ctrl Pts',(0.9967642879194,-0.2922848411075,-5.027935277932));
#36540=CARTESIAN_POINT('Ctrl Pts',(0.5672074110512,-0.8701983836261,-5.078635551508));
#36541=CARTESIAN_POINT('Ctrl Pts',(-0.1349232962637,-1.029934550421,-5.129335825084));
#36542=CARTESIAN_POINT('Ctrl Pts',(-0.7722160642937,-0.694731476232,-5.18003609866));
#36543=CARTESIAN_POINT('Ctrl Pts',(-1.038417259008,-0.02567236295293,-5.230736372236));
#36544=CARTESIAN_POINT('Ctrl Pts',(-0.8056028125943,0.6557237088569,-5.281436645812));
#36545=CARTESIAN_POINT('Ctrl Pts',(-0.1856526550803,1.022009082971,-5.332136919388));
#36546=CARTESIAN_POINT('Ctrl Pts',(0.5235136417157,0.897163831801,-5.382837192964));
#36547=CARTESIAN_POINT('Ctrl Pts',(0.9811033264056,0.3411828488149,-5.43353746654));
#36548=CARTESIAN_POINT('Ctrl Pts',(0.9672198151093,-0.3787549404562,-5.484237740116));
#36549=CARTESIAN_POINT('Ctrl Pts',(0.4885348785918,-0.9166805035943,-5.534938013692));
#36550=CARTESIAN_POINT('Ctrl Pts',(-0.2249174616962,-1.014091510121,-5.585638287268));
#36551=CARTESIAN_POINT('Ctrl Pts',(-0.8302848782164,-0.6241767463422,-5.636338560844));
#36552=CARTESIAN_POINT('Ctrl Pts',(-1.036655225136,0.0656888176107,-5.68703883442));
#36553=CARTESIAN_POINT('Ctrl Pts',(-0.74485777085,0.7239868909991,-5.737739107996));
#36554=CARTESIAN_POINT('Ctrl Pts',(-0.09511182443393,1.034371840274,-5.788439381572));
#36555=CARTESIAN_POINT('Ctrl Pts',(0.6003253513746,0.8476787581516,-5.839139655148));
#36556=CARTESIAN_POINT('Ctrl Pts',(1.007330257735,0.2536542052052,-5.889839928724));
#36557=CARTESIAN_POINT('Ctrl Pts',(0.9300475649187,-0.4623545048573,-5.9405402023));
#36558=CARTESIAN_POINT('Ctrl Pts',(0.5810918409035,-0.7913465001737,-5.974340384684));
#36559=CARTESIAN_POINT('Ctrl Pts',(0.3735576354296,-0.8794948162679,-5.991240475876));
#36560=CARTESIAN_POINT('',(-0.733992715443622,1.01100376667461,-4.23040083151671));
#36561=CARTESIAN_POINT('Ctrl Pts',(-0.733858249660088,1.01085165460594,
-4.23006677329136));
#36562=CARTESIAN_POINT('Ctrl Pts',(-0.656624184784989,1.06704092143774,
-4.23558293594093));
#36563=CARTESIAN_POINT('Ctrl Pts',(-0.573048085765063,1.11459061696366,
-4.24108426906003));
#36564=CARTESIAN_POINT('Ctrl Pts',(-0.397055758914472,1.18918176106475,
-4.25195538849777));
#36565=CARTESIAN_POINT('Ctrl Pts',(-0.305762422032486,1.21563445447107,
-4.25725691531341));
#36566=CARTESIAN_POINT('Ctrl Pts',(-0.0531416665414995,1.25829397068379,
-4.27193030467578));
#36567=CARTESIAN_POINT('Ctrl Pts',(0.111123233468843,1.25441685178384,-4.28132801175063));
#36568=CARTESIAN_POINT('Ctrl Pts',(0.460594426391743,1.17866367040215,-4.30187191226297));
#36569=CARTESIAN_POINT('Ctrl Pts',(0.607960344748149,1.09991175854457,-4.31103977577589));
#36570=CARTESIAN_POINT('Ctrl Pts',(0.847486150103628,0.931203796797836,
-4.3279104257407));
#36571=CARTESIAN_POINT('Ctrl Pts',(0.961057414879083,0.814115725342219,
-4.33722749733213));
#36572=CARTESIAN_POINT('Ctrl Pts',(1.08901672234342,0.618045849386044,-4.3505869949951));
#36573=CARTESIAN_POINT('Ctrl Pts',(1.12361536676105,0.552784443534289,-4.35472027078159));
#36574=CARTESIAN_POINT('Ctrl Pts',(1.21477335836627,0.334472710659284,-4.36818280141384));
#36575=CARTESIAN_POINT('Ctrl Pts',(1.24755694627055,0.172180252671676,-4.37763258313196));
#36576=CARTESIAN_POINT('Ctrl Pts',(1.25087080107157,-0.150696375148907,
-4.39624596226418));
#36577=CARTESIAN_POINT('Ctrl Pts',(1.22275531302733,-0.305267334806458,
-4.40490395817152));
#36578=CARTESIAN_POINT('Ctrl Pts',(1.13388572849473,-0.531217437947803,
-4.41880417367254));
#36579=CARTESIAN_POINT('Ctrl Pts',(1.09568502554916,-0.605568589361117,
-4.42360727682551));
#36580=CARTESIAN_POINT('Ctrl Pts',(0.974278367896043,-0.794239096200339,
-4.43657050998369));
#36581=CARTESIAN_POINT('Ctrl Pts',(0.869783750705368,-0.913412171771251,
-4.44557250988085));
#36582=CARTESIAN_POINT('Ctrl Pts',(0.596567590420889,-1.11131409615458,
-4.46464303751621));
#36583=CARTESIAN_POINT('Ctrl Pts',(0.449841362804258,-1.17396421545565,
-4.47370678657374));
#36584=CARTESIAN_POINT('Ctrl Pts',(0.230696328844762,-1.23046801237028,
-4.48678250348742));
#36585=CARTESIAN_POINT('Ctrl Pts',(0.148087128506761,-1.24338760407243,
-4.49158580711337));
#36586=CARTESIAN_POINT('Ctrl Pts',(-0.0149243810933619,-1.25237940005118,
-4.50092857601243));
#36587=CARTESIAN_POINT('Ctrl Pts',(-0.0948562697134099,-1.2490356489232,
-4.50541104605373));
#36588=CARTESIAN_POINT('Ctrl Pts',(-0.319602267413793,-1.21692007737163,
-4.51830918900455));
#36589=CARTESIAN_POINT('Ctrl Pts',(-0.461052665580677,-1.169955946995,-4.52682047729437));
#36590=CARTESIAN_POINT('Ctrl Pts',(-0.662743299830164,-1.06213194850692,
-4.54002721971129));
#36591=CARTESIAN_POINT('Ctrl Pts',(-0.731406571816841,-1.01645316128059,
-4.5447559342723));
#36592=CARTESIAN_POINT('Ctrl Pts',(-0.855854786351091,-0.914449669496606,
-4.5539350964962));
#36593=CARTESIAN_POINT('Ctrl Pts',(-0.911397890189387,-0.859134433280608,
-4.55831634526413));
#36594=CARTESIAN_POINT('Ctrl Pts',(-1.06306225128544,-0.67548686397915,
-4.57188984157829));
#36595=CARTESIAN_POINT('Ctrl Pts',(-1.14070195689524,-0.532848962125197,
-4.58116298367123));
#36596=CARTESIAN_POINT('Ctrl Pts',(-1.2408543648333,-0.222972138419077,
-4.5999283034156));
#36597=CARTESIAN_POINT('Ctrl Pts',(-1.25922712849244,-0.0621179230072517,
-4.60883218350856));
#36598=CARTESIAN_POINT('Ctrl Pts',(-1.23199809975094,0.260794349941966,
-4.62742590355341));
#36599=CARTESIAN_POINT('Ctrl Pts',(-1.18777147826677,0.418227500329566,
-4.63678069006497));
#36600=CARTESIAN_POINT('Ctrl Pts',(-1.07195006124452,0.650201057523823,
-4.65165382848055));
#36601=CARTESIAN_POINT('Ctrl Pts',(-1.0174876518875,0.733036893765051,-4.657189771762));
#36602=CARTESIAN_POINT('Ctrl Pts',(-0.888289399775233,0.88459835520095,
-4.66850449009343));
#36603=CARTESIAN_POINT('Ctrl Pts',(-0.814482997793992,0.952439727927399,
-4.67423593308293));
#36604=CARTESIAN_POINT('Ctrl Pts',(-0.733889624077889,1.01082887649925,
-4.6799837403912));
#36605=CARTESIAN_POINT('',(-0.569874894277251,0.784947385717,-4.39168333211734));
#36606=CARTESIAN_POINT('Ctrl Pts',(-0.569529227319458,0.784474235852257,
-4.39166755057106));
#36607=CARTESIAN_POINT('Ctrl Pts',(-0.484636830506631,0.846338281756473,
-4.39942370350874));
#36608=CARTESIAN_POINT('Ctrl Pts',(-0.374984443336166,0.906078704177597,
-4.4084779942885));
#36609=CARTESIAN_POINT('Ctrl Pts',(-0.113185176117061,0.971160390418816,
-4.42841745272176));
#36610=CARTESIAN_POINT('Ctrl Pts',(0.0168632307072354,0.977315047570584,
-4.43783815175513));
#36611=CARTESIAN_POINT('Ctrl Pts',(0.269797863995035,0.940369046501483,
-4.45671267634792));
#36612=CARTESIAN_POINT('Ctrl Pts',(0.389640305530905,0.897489900285447,
-4.46594718063363));
#36613=CARTESIAN_POINT('Ctrl Pts',(0.606900163119448,0.766016505526538,
-4.4847012708543));
#36614=CARTESIAN_POINT('Ctrl Pts',(0.702014304273932,0.680148659476022,
-4.49397871953176));
#36615=CARTESIAN_POINT('Ctrl Pts',(0.865323843694858,0.462565672761075,
-4.51408024418007));
#36616=CARTESIAN_POINT('Ctrl Pts',(0.913111224941747,0.343586895448416,
-4.52336294452809));
#36617=CARTESIAN_POINT('Ctrl Pts',(0.969666070452136,0.119032334142472,
-4.54045552846132));
#36618=CARTESIAN_POINT('Ctrl Pts',(0.977445580061419,-0.00647510823698313,
-4.54956916057514));
#36619=CARTESIAN_POINT('Ctrl Pts',(0.9416925488968,-0.277924360370847,-4.5698103034962));
#36620=CARTESIAN_POINT('Ctrl Pts',(0.889895690185117,-0.398128861572051,
-4.57926951223364));
#36621=CARTESIAN_POINT('Ctrl Pts',(0.776609403954023,-0.59237863363198,
-4.59586369550252));
#36622=CARTESIAN_POINT('Ctrl Pts',(0.696444599699867,-0.685910391350863,
-4.60480297831157));
#36623=CARTESIAN_POINT('Ctrl Pts',(0.500258893832906,-0.841037207495601,
-4.62329685730815));
#36624=CARTESIAN_POINT('Ctrl Pts',(0.382468956290877,-0.899797001880555,
-4.6328259720572));
#36625=CARTESIAN_POINT('Ctrl Pts',(0.15959431279224,-0.961644353830406,
-4.64989505946642));
#36626=CARTESIAN_POINT('Ctrl Pts',(0.0346117104225062,-0.980352509949182,
-4.65904365625598));
#36627=CARTESIAN_POINT('Ctrl Pts',(-0.236343379195953,-0.949058136150462,
-4.67920711064833));
#36628=CARTESIAN_POINT('Ctrl Pts',(-0.360775378580012,-0.908544798855145,
-4.68867655849675));
#36629=CARTESIAN_POINT('Ctrl Pts',(-0.584818511226693,-0.784081692722746,
-4.70759675484773));
#36630=CARTESIAN_POINT('Ctrl Pts',(-0.680375181353425,-0.703150803980083,
-4.7166800988285));
#36631=CARTESIAN_POINT('Ctrl Pts',(-0.837749469773741,-0.503691778064584,
-4.73544988364439));
#36632=CARTESIAN_POINT('Ctrl Pts',(-0.89682553691833,-0.388763017720274,
-4.74480262132333));
#36633=CARTESIAN_POINT('Ctrl Pts',(-0.975938218374794,-0.116044677743505,
-4.76577767278224));
#36634=CARTESIAN_POINT('Ctrl Pts',(-0.974268306023395,0.0140308472029775,
-4.77517931330129));
#36635=CARTESIAN_POINT('Ctrl Pts',(-0.949101604663957,0.232235392643103,
-4.79139625667692));
#36636=CARTESIAN_POINT('Ctrl Pts',(-0.91129449898224,0.35349405795863,-4.80059642192052));
#36637=CARTESIAN_POINT('Ctrl Pts',(-0.781891247636186,0.59323425922455,
-4.82073207531561));
#36638=CARTESIAN_POINT('Ctrl Pts',(-0.692498942409321,0.686771888047504,
-4.83009240233825));
#36639=CARTESIAN_POINT('Ctrl Pts',(-0.514446522986027,0.83039260255699,
-4.8469749141452));
#36640=CARTESIAN_POINT('Ctrl Pts',(-0.404935910777101,0.889665186064185,
-4.85600502288631));
#36641=CARTESIAN_POINT('Ctrl Pts',(-0.134905330150572,0.974113150346371,
-4.87692444704566));
#36642=CARTESIAN_POINT('Ctrl Pts',(0.00160707428452082,0.97375035982292,
-4.88676307743964));
#36643=CARTESIAN_POINT('Ctrl Pts',(0.174562797360105,0.956837613378726,
-4.89958694906931));
#36644=CARTESIAN_POINT('Ctrl Pts',(0.302975074330177,0.935375752863402,
-4.90897285600405));
#36645=CARTESIAN_POINT('Ctrl Pts',(0.558866320705603,0.802941907514622,
-4.93027680936402));
#36646=CARTESIAN_POINT('Ctrl Pts',(0.660953880687901,0.720339425358645,
-4.93978064224544));
#36647=CARTESIAN_POINT('Ctrl Pts',(0.812076348801619,0.540264139141327,
-4.95713186062111));
#36648=CARTESIAN_POINT('Ctrl Pts',(0.88006177468165,0.433274456521509,-4.96631266398249));
#36649=CARTESIAN_POINT('Ctrl Pts',(0.962132946141089,0.174042975000006,
-4.98640717877759));
#36650=CARTESIAN_POINT('Ctrl Pts',(0.976467507927319,0.044763554717978,
-4.99581971407352));
#36651=CARTESIAN_POINT('Ctrl Pts',(0.955533483765511,-0.21011727305588,
-5.01470463930562));
#36652=CARTESIAN_POINT('Ctrl Pts',(0.920176570954095,-0.332501531122732,
-5.02394664366846));
#36653=CARTESIAN_POINT('Ctrl Pts',(0.802602751105269,-0.5575519956936,-5.04269775708713));
#36654=CARTESIAN_POINT('Ctrl Pts',(0.722990503962228,-0.657793652245648,
-5.05196625878101));
#36655=CARTESIAN_POINT('Ctrl Pts',(0.516180264657058,-0.834477351286836,
-5.07206541676142));
#36656=CARTESIAN_POINT('Ctrl Pts',(0.400332533119837,-0.889665217872399,
-5.08135517885404));
#36657=CARTESIAN_POINT('Ctrl Pts',(0.180035963144124,-0.960200187879756,
-5.09842867575985));
#36658=CARTESIAN_POINT('Ctrl Pts',(0.0554083971430053,-0.975898242544961,
-5.10753294808212));
#36659=CARTESIAN_POINT('Ctrl Pts',(-0.217938297569027,-0.957398080705504,
-5.12778753322606));
#36660=CARTESIAN_POINT('Ctrl Pts',(-0.341312967821623,-0.913148629947774,
-5.13725865191567));
#36661=CARTESIAN_POINT('Ctrl Pts',(-0.541952151862897,-0.812593040742933,
-5.15382004071268));
#36662=CARTESIAN_POINT('Ctrl Pts',(-0.640272812359031,-0.738621444203264,
-5.16274947913229));
#36663=CARTESIAN_POINT('Ctrl Pts',(-0.801962028794439,-0.55889875331323,
-5.18062559567604));
#36664=CARTESIAN_POINT('Ctrl Pts',(-0.865164262002844,-0.453332531951965,
-5.18955503409562));
#36665=CARTESIAN_POINT('Ctrl Pts',(-0.944023648542113,-0.243216597649746,
-5.20611642289259));
#36666=CARTESIAN_POINT('Ctrl Pts',(-0.975029766934585,-0.115866906741222,
-5.21558754158214));
#36667=CARTESIAN_POINT('Ctrl Pts',(-0.964630825541233,0.157907696748229,
-5.23584212672606));
#36668=CARTESIAN_POINT('Ctrl Pts',(-0.935891024457689,0.280188042516773,
-5.24494639904833));
#36669=CARTESIAN_POINT('Ctrl Pts',(-0.842541035141814,0.491828162134398,
-5.26201989595419));
#36670=CARTESIAN_POINT('Ctrl Pts',(-0.77545608704459,0.601217408678329,
-5.27130965804686));
#36671=CARTESIAN_POINT('Ctrl Pts',(-0.577968766812469,0.788263827879969,
-5.29140881602737));
#36672=CARTESIAN_POINT('Ctrl Pts',(-0.469898014985213,0.856872954117068,
-5.30067731772131));
#36673=CARTESIAN_POINT('Ctrl Pts',(-0.23371382158273,0.9500842275998,-5.31942843114003));
#36674=CARTESIAN_POINT('Ctrl Pts',(-0.108285830905315,0.972351626655508,
-5.32867043550288));
#36675=CARTESIAN_POINT('Ctrl Pts',(0.147382057119419,0.966318321832297,
-5.34755536073492));
#36676=CARTESIAN_POINT('Ctrl Pts',(0.274432011617761,0.938444369260619,
-5.35696789603077));
#36677=CARTESIAN_POINT('Ctrl Pts',(0.523575091539709,0.829520708270325,
-5.37706241082583));
#36678=CARTESIAN_POINT('Ctrl Pts',(0.622807399176715,0.750642577966378,
-5.38624321418721));
#36679=CARTESIAN_POINT('Ctrl Pts',(0.785960420543063,0.581390692617465,
-5.40359443256289));
#36680=CARTESIAN_POINT('Ctrl Pts',(0.857348683054847,0.471169297520893,
-5.41309826544433));
#36681=CARTESIAN_POINT('Ctrl Pts',(0.962088321082967,0.202750480014205,
-5.43440221880429));
#36682=CARTESIAN_POINT('Ctrl Pts',(0.96990295440032,0.0727918102781609,
-5.44378812573895));
#36683=CARTESIAN_POINT('Ctrl Pts',(0.968501283832614,-0.100983212255705,
-5.45661199736858));
#36684=CARTESIAN_POINT('Ctrl Pts',(0.954480930335871,-0.236774220313613,
-5.46645062776246));
#36685=CARTESIAN_POINT('Ctrl Pts',(0.842056053068118,-0.496405921220222,
-5.48737005192177));
#36686=CARTESIAN_POINT('Ctrl Pts',(0.771576711542563,-0.599062999690922,
-5.49640016066297));
#36687=CARTESIAN_POINT('Ctrl Pts',(0.609997938988823,-0.760994695040373,
-5.51328267247002));
#36688=CARTESIAN_POINT('Ctrl Pts',(0.507563614314368,-0.840035705712442,
-5.52264299949269));
#36689=CARTESIAN_POINT('Ctrl Pts',(0.25552523333294,-0.943463071888589,
-5.54277865288789));
#36690=CARTESIAN_POINT('Ctrl Pts',(0.130958452487734,-0.968285607294546,
-5.55197881813158));
#36691=CARTESIAN_POINT('Ctrl Pts',(-0.0886831345803024,-0.970325150882856,
-5.56819576150725));
#36692=CARTESIAN_POINT('Ctrl Pts',(-0.218210781696016,-0.958282749541544,
-5.57759740202637));
#36693=CARTESIAN_POINT('Ctrl Pts',(-0.481077340281054,-0.850880320776047,
-5.59857245348522));
#36694=CARTESIAN_POINT('Ctrl Pts',(-0.589143120265966,-0.780025618322455,
-5.60792519116405));
#36695=CARTESIAN_POINT('Ctrl Pts',(-0.770913413302382,-0.602514688393461,
-5.62669497597979));
#36696=CARTESIAN_POINT('Ctrl Pts',(-0.841327391289032,-0.498963939181014,
-5.63577831996048));
#36697=CARTESIAN_POINT('Ctrl Pts',(-0.941495735081663,-0.263055709192854,
-5.65469851631137));
#36698=CARTESIAN_POINT('Ctrl Pts',(-0.968675143304464,-0.135048159657013,
-5.66416796415975));
#36699=CARTESIAN_POINT('Ctrl Pts',(-0.971251168838689,0.13769597412805,
-5.68433141855208));
#36700=CARTESIAN_POINT('Ctrl Pts',(-0.93948061393768,0.260012276564817,
-5.69348001534169));
#36701=CARTESIAN_POINT('Ctrl Pts',(-0.854498309521642,0.475131335678752,
-5.71054910275097));
#36702=CARTESIAN_POINT('Ctrl Pts',(-0.783656704497057,0.586075690288882,
-5.72007821750008));
#36703=CARTESIAN_POINT('Ctrl Pts',(-0.608725574238606,0.76482764115972,
-5.73857209649671));
#36704=CARTESIAN_POINT('Ctrl Pts',(-0.507269174368512,0.834693115239855,
-5.74751137930577));
#36705=CARTESIAN_POINT('Ctrl Pts',(-0.302165962186496,0.926885462785101,
-5.7641055625747));
#36706=CARTESIAN_POINT('Ctrl Pts',(-0.177173705923737,0.965730958737602,
-5.77356477131219));
#36707=CARTESIAN_POINT('Ctrl Pts',(0.0965315452820904,0.972688773335761,
-5.79380591423329));
#36708=CARTESIAN_POINT('Ctrl Pts',(0.2205210636506,0.951730763001617,-5.80291954634709));
#36709=CARTESIAN_POINT('Ctrl Pts',(0.437868240623845,0.871834541464923,
-5.82001213028032));
#36710=CARTESIAN_POINT('Ctrl Pts',(0.551150726807563,0.811779053944627,
-5.82929483062832));
#36711=CARTESIAN_POINT('Ctrl Pts',(0.750318872098348,0.626456600703951,
-5.84939635527662));
#36712=CARTESIAN_POINT('Ctrl Pts',(0.825688954935261,0.522825826094886,
-5.85867380395408));
#36713=CARTESIAN_POINT('Ctrl Pts',(0.933543174363937,0.292924615571325,
-5.87742789417475));
#36714=CARTESIAN_POINT('Ctrl Pts',(0.963558721675801,0.169231855504208,
-5.88666239846044));
#36715=CARTESIAN_POINT('Ctrl Pts',(0.973653321148666,-0.0861874757390947,
-5.9055369230532));
#36716=CARTESIAN_POINT('Ctrl Pts',(0.953832746458545,-0.214863863398631,
-5.91495762208655));
#36717=CARTESIAN_POINT('Ctrl Pts',(0.861533508110168,-0.46835027550829,
-5.93489708439995));
#36718=CARTESIAN_POINT('Ctrl Pts',(0.790573961255546,-0.571099081510327,
-5.94395137805178));
#36719=CARTESIAN_POINT('Ctrl Pts',(0.720110998144666,-0.649001939469338,
-5.95170753282398));
#36720=CARTESIAN_POINT('',(-0.7343749446882,1.011530247009,-4.230025253169));
#36721=CARTESIAN_POINT('Ctrl Pts',(0.7205712401658,-0.6275615720196,-2.918810030463));
#36722=CARTESIAN_POINT('Ctrl Pts',(0.5724856689652,-0.7975946149087,-2.935710121655));
#36723=CARTESIAN_POINT('Ctrl Pts',(0.1516001974293,-1.027510360684,-2.969510304039));
#36724=CARTESIAN_POINT('Ctrl Pts',(-0.5531418425703,-0.879254687769,-3.020210577615));
#36725=CARTESIAN_POINT('Ctrl Pts',(-0.9919188003728,-0.3082967693496,-3.070910851191));
#36726=CARTESIAN_POINT('Ctrl Pts',(-0.9540654718091,0.4107681080609,-3.121611124767));
#36727=CARTESIAN_POINT('Ctrl Pts',(-0.4577212901491,0.9324491072861,-3.172311398343));
#36728=CARTESIAN_POINT('Ctrl Pts',(0.2585798251871,1.006034567282,-3.223011671919));
#36729=CARTESIAN_POINT('Ctrl Pts',(0.8506201287607,0.5961669113734,-3.273711945495));
#36730=CARTESIAN_POINT('Ctrl Pts',(1.033891258762,-0.1001914194485,-3.324412219071));
#36731=CARTESIAN_POINT('Ctrl Pts',(0.7203217911921,-0.7484022918219,-3.375112492647));
#36732=CARTESIAN_POINT('Ctrl Pts',(0.06059873957321,-1.03696541332,-3.425812766223));
#36733=CARTESIAN_POINT('Ctrl Pts',(-0.6282452790402,-0.8272105794617,-3.476513039799));
#36734=CARTESIAN_POINT('Ctrl Pts',(-1.015183472352,-0.2199363353731,-3.527213313375));
#36735=CARTESIAN_POINT('Ctrl Pts',(-0.914271115017,0.4930292103498,-3.577913586951));
#36736=CARTESIAN_POINT('Ctrl Pts',(-0.3740020515216,0.969067561873,-3.628613860527));
#36737=CARTESIAN_POINT('Ctrl Pts',(0.3459952203822,0.9794165515745,-3.679314134103));
#36738=CARTESIAN_POINT('Ctrl Pts',(0.8997230806097,0.5191029302932,-3.730014407679));
#36739=CARTESIAN_POINT('Ctrl Pts',(1.021085351762,-0.1906677173599,-3.780714681255));
#36740=CARTESIAN_POINT('Ctrl Pts',(0.6517609003688,-0.8088122172466,-3.831414954831));
#36741=CARTESIAN_POINT('Ctrl Pts',(-0.03076990492567,-1.038278713527,-3.882115228407));
#36742=CARTESIAN_POINT('Ctrl Pts',(-0.6985141072616,-0.7687961473049,-3.932815501983));
#36743=CARTESIAN_POINT('Ctrl Pts',(-1.030584511335,-0.1298654627114,-3.983515775559));
#36744=CARTESIAN_POINT('Ctrl Pts',(-0.8674033346712,0.5714725983469,-4.034216049135));
#36745=CARTESIAN_POINT('Ctrl Pts',(-0.287387948432,0.9981871770197,-4.084916322711));
#36746=CARTESIAN_POINT('Ctrl Pts',(0.4307328640486,0.9452188399008,-4.135616596287));
#36747=CARTESIAN_POINT('Ctrl Pts',(0.9418633284912,0.4380217575791,-4.186316869863));
#36748=CARTESIAN_POINT('Ctrl Pts',(1.000377225472,-0.2796685240019,-4.237017143439));
#36749=CARTESIAN_POINT('Ctrl Pts',(0.5781569339062,-0.8629627320519,-4.287717417015));
#36750=CARTESIAN_POINT('Ctrl Pts',(-0.1219033535594,-1.031557528929,-4.338417690591));
#36751=CARTESIAN_POINT('Ctrl Pts',(-0.7633663370709,-0.7044300106834,-4.389117964167));
#36752=CARTESIAN_POINT('Ctrl Pts',(-1.038050796595,-0.03879752124175,-4.439818237743));
#36753=CARTESIAN_POINT('Ctrl Pts',(-0.813670763595,0.6455230821929,-4.490518511319));
#36754=CARTESIAN_POINT('Ctrl Pts',(-0.4039685755409,0.8948219939615,-4.524318693703));
#36755=CARTESIAN_POINT('Ctrl Pts',(-0.1826474890299,0.9379212832541,-4.541218784895));
#36756=CARTESIAN_POINT('Ctrl Pts',(0.7982233492482,-0.6951905265629,-2.978261763091));
#36757=CARTESIAN_POINT('Ctrl Pts',(0.6341793879712,-0.8835471211815,-2.995161854283));
#36758=CARTESIAN_POINT('Ctrl Pts',(0.1679373399789,-1.138239657336,-3.028962036667));
#36759=CARTESIAN_POINT('Ctrl Pts',(-0.6127509808526,-0.9740072633923,-3.079662310243));
#36760=CARTESIAN_POINT('Ctrl Pts',(-1.098812584906,-0.3415202634732,-3.130362583819));
#36761=CARTESIAN_POINT('Ctrl Pts',(-1.056880005555,0.4550343903613,-3.181062857395));
#36762=CARTESIAN_POINT('Ctrl Pts',(-0.5070474657869,1.032934161028,-3.231763130971));
#36763=CARTESIAN_POINT('Ctrl Pts',(0.2864455901145,1.114449532528,-3.282463404547));
#36764=CARTESIAN_POINT('Ctrl Pts',(0.9422869110915,0.6604126312312,-3.333163678123));
#36765=CARTESIAN_POINT('Ctrl Pts',(1.145308190676,-0.1109885129189,-3.383863951699));
#36766=CARTESIAN_POINT('Ctrl Pts',(0.7979470184926,-0.8290536045064,-3.434564225275));
#36767=CARTESIAN_POINT('Ctrl Pts',(0.06712914166712,-1.148713630431,-3.485264498851));
#36768=CARTESIAN_POINT('Ctrl Pts',(-0.6959479130327,-0.9163546398542,-3.535964772427));
#36769=CARTESIAN_POINT('Ctrl Pts',(-1.12458436617,-0.2436376980609,-3.586665046003));
#36770=CARTESIAN_POINT('Ctrl Pts',(-1.012797223744,0.546160331728,-3.637365319579));
#36771=CARTESIAN_POINT('Ctrl Pts',(-0.4143062525262,1.073498790637,-3.688065593155));
#36772=CARTESIAN_POINT('Ctrl Pts',(0.3832812749699,1.084963035615,-3.738765866731));
#36773=CARTESIAN_POINT('Ctrl Pts',(0.9966814254686,0.5750438770327,-3.789466140307));
#36774=CARTESIAN_POINT('Ctrl Pts',(1.131122259562,-0.2112149576071,-3.840166413883));
#36775=CARTESIAN_POINT('Ctrl Pts',(0.7219976871151,-0.8959735845339,-3.890866687459));
#36776=CARTESIAN_POINT('Ctrl Pts',(-0.03408581302824,-1.150168457978,-3.941566961035));
#36777=CARTESIAN_POINT('Ctrl Pts',(-0.773789237088,-0.8516451967325,-3.992267234611));
#36778=CARTESIAN_POINT('Ctrl Pts',(-1.141645092763,-0.1438603691333,-4.042967508187));
#36779=CARTESIAN_POINT('Ctrl Pts',(-0.9608787533499,0.63305714415,-4.093667781763));
#36780=CARTESIAN_POINT('Ctrl Pts',(-0.3183582107415,1.105756470983,-4.144368055339));
#36781=CARTESIAN_POINT('Ctrl Pts',(0.4771506413343,1.047080019436,-4.195068328915));
#36782=CARTESIAN_POINT('Ctrl Pts',(1.043362902507,0.485225019941,-4.245768602491));
#36783=CARTESIAN_POINT('Ctrl Pts',(1.108182529245,-0.3098069052225,-4.296468876067));
#36784=CARTESIAN_POINT('Ctrl Pts',(0.6404618148061,-0.9559596107337,-4.347169149643));
#36785=CARTESIAN_POINT('Ctrl Pts',(-0.1350402260578,-1.142722967259,-4.397869423219));
#36786=CARTESIAN_POINT('Ctrl Pts',(-0.8456302448871,-0.7803426657845,-4.448569696795));
#36787=CARTESIAN_POINT('Ctrl Pts',(-1.149915979657,-0.04297852262462,-4.499269970371));
#36788=CARTESIAN_POINT('Ctrl Pts',(-0.9013557104398,0.715087652633,-4.549970243947));
#36789=CARTESIAN_POINT('Ctrl Pts',(-0.4475021085842,0.9912521749224,-4.583770426331));
#36790=CARTESIAN_POINT('Ctrl Pts',(-0.2023304321606,1.038996044136,-4.600670517523));
#36791=CARTESIAN_POINT('Ctrl Pts',(0.8758754583306,-0.7628194811062,-3.037713495719));
#36792=CARTESIAN_POINT('Ctrl Pts',(0.6958731069771,-0.9694996274544,-3.054613586911));
#36793=CARTESIAN_POINT('Ctrl Pts',(0.1842744825284,-1.248968953987,-3.088413769295));
#36794=CARTESIAN_POINT('Ctrl Pts',(-0.6723601191349,-1.068759839016,-3.139114042871));
#36795=CARTESIAN_POINT('Ctrl Pts',(-1.20570636944,-0.3747437575968,-3.189814316447));
#36796=CARTESIAN_POINT('Ctrl Pts',(-1.159694539302,0.4993006726617,-3.240514590023));
#36797=CARTESIAN_POINT('Ctrl Pts',(-0.5563736414247,1.133419214769,-3.291214863599));
#36798=CARTESIAN_POINT('Ctrl Pts',(0.314311355042,1.222864497773,-3.341915137175));
#36799=CARTESIAN_POINT('Ctrl Pts',(1.033953693422,0.7246583510889,-3.392615410751));
#36800=CARTESIAN_POINT('Ctrl Pts',(1.256725122589,-0.1217856063893,-3.443315684327));
#36801=CARTESIAN_POINT('Ctrl Pts',(0.8755722457931,-0.9097049171909,-3.494015957903));
#36802=CARTESIAN_POINT('Ctrl Pts',(0.07365954376103,-1.260461847542,-3.544716231479));
#36803=CARTESIAN_POINT('Ctrl Pts',(-0.7636505470253,-1.005498700247,-3.595416505055));
#36804=CARTESIAN_POINT('Ctrl Pts',(-1.233985259988,-0.2673390607487,-3.646116778631));
#36805=CARTESIAN_POINT('Ctrl Pts',(-1.111323332471,0.5992914531062,-3.696817052207));
#36806=CARTESIAN_POINT('Ctrl Pts',(-0.4546104535308,1.177930019402,-3.747517325783));
#36807=CARTESIAN_POINT('Ctrl Pts',(0.4205673295575,1.190509519655,-3.798217599359));
#36808=CARTESIAN_POINT('Ctrl Pts',(1.093639770328,0.6309848237721,-3.848917872935));
#36809=CARTESIAN_POINT('Ctrl Pts',(1.241159167361,-0.2317621978543,-3.899618146511));
#36810=CARTESIAN_POINT('Ctrl Pts',(0.7922344738614,-0.9831349518212,-3.950318420088));
#36811=CARTESIAN_POINT('Ctrl Pts',(-0.03740172113081,-1.262058202429,-4.001018693664));
#36812=CARTESIAN_POINT('Ctrl Pts',(-0.8490643669144,-0.9344942461601,-4.05171896724));
#36813=CARTESIAN_POINT('Ctrl Pts',(-1.252705674191,-0.1578552755553,-4.102419240816));
#36814=CARTESIAN_POINT('Ctrl Pts',(-1.054354172029,0.6946416899531,-4.153119514392));
#36815=CARTESIAN_POINT('Ctrl Pts',(-0.3493284730509,1.213325764945,-4.203819787968));
#36816=CARTESIAN_POINT('Ctrl Pts',(0.5235684186199,1.148941198972,-4.254520061544));
#36817=CARTESIAN_POINT('Ctrl Pts',(1.144862476522,0.5324282823029,-4.30522033512));
#36818=CARTESIAN_POINT('Ctrl Pts',(1.215987833017,-0.3399452864431,-4.355920608696));
#36819=CARTESIAN_POINT('Ctrl Pts',(0.702766695706,-1.048956489416,-4.406620882272));
#36820=CARTESIAN_POINT('Ctrl Pts',(-0.1481770985562,-1.253888405589,-4.457321155848));
#36821=CARTESIAN_POINT('Ctrl Pts',(-0.9278941527034,-0.8562553208856,-4.508021429424));
#36822=CARTESIAN_POINT('Ctrl Pts',(-1.261781162719,-0.04715952400749,-4.558721703));
#36823=CARTESIAN_POINT('Ctrl Pts',(-0.9890406572845,0.7846522230731,-4.609421976576));
#36824=CARTESIAN_POINT('Ctrl Pts',(-0.4910356416274,1.087682355883,-4.64322215896));
#36825=CARTESIAN_POINT('Ctrl Pts',(-0.2220133752913,1.140070805017,-4.660122250152));
#36826=CARTESIAN_POINT('Ctrl Pts',(0.9535275674129,-0.8304484356495,-3.097165228348));
#36827=CARTESIAN_POINT('Ctrl Pts',(0.7575668259831,-1.055452133727,-3.11406531954));
#36828=CARTESIAN_POINT('Ctrl Pts',(0.200611625078,-1.359698250639,-3.147865501924));
#36829=CARTESIAN_POINT('Ctrl Pts',(-0.7319692574172,-1.163512414639,-3.1985657755));
#36830=CARTESIAN_POINT('Ctrl Pts',(-1.312600153974,-0.4079672517203,-3.249266049076));
#36831=CARTESIAN_POINT('Ctrl Pts',(-1.262509073048,0.543566954962,-3.299966322652));
#36832=CARTESIAN_POINT('Ctrl Pts',(-0.6056998170625,1.233904268511,-3.350666596228));
#36833=CARTESIAN_POINT('Ctrl Pts',(0.3421771199694,1.331279463018,-3.401366869804));
#36834=CARTESIAN_POINT('Ctrl Pts',(1.125620475753,0.7889040709467,-3.45206714338));
#36835=CARTESIAN_POINT('Ctrl Pts',(1.368142054503,-0.1325826998597,-3.502767416956));
#36836=CARTESIAN_POINT('Ctrl Pts',(0.9531974730936,-0.9903562298753,-3.553467690532));
#36837=CARTESIAN_POINT('Ctrl Pts',(0.08018994585494,-1.372210064652,-3.604167964108));
#36838=CARTESIAN_POINT('Ctrl Pts',(-0.8313531810178,-1.094642760639,-3.654868237684));
#36839=CARTESIAN_POINT('Ctrl Pts',(-1.343386153806,-0.2910404234365,-3.70556851126));
#36840=CARTESIAN_POINT('Ctrl Pts',(-1.209849441198,0.6524225744844,-3.756268784836));
#36841=CARTESIAN_POINT('Ctrl Pts',(-0.4949146545354,1.282361248166,-3.806969058412));
#36842=CARTESIAN_POINT('Ctrl Pts',(0.4578533841451,1.296056003695,-3.857669331988));
#36843=CARTESIAN_POINT('Ctrl Pts',(1.190598115186,0.6869257705116,-3.908369605564));
#36844=CARTESIAN_POINT('Ctrl Pts',(1.351196075161,-0.2523094381015,-3.95906987914));
#36845=CARTESIAN_POINT('Ctrl Pts',(0.8624712606077,-1.070296319109,-4.009770152716));
#36846=CARTESIAN_POINT('Ctrl Pts',(-0.04071762923338,-1.373947946879,-4.060470426292));
#36847=CARTESIAN_POINT('Ctrl Pts',(-0.9243394967408,-1.017343295588,-4.111170699868));
#36848=CARTESIAN_POINT('Ctrl Pts',(-1.363766255618,-0.1718501819773,-4.161870973444));
#36849=CARTESIAN_POINT('Ctrl Pts',(-1.147829590707,0.7562262357563,-4.21257124702));
#36850=CARTESIAN_POINT('Ctrl Pts',(-0.3802987353604,1.320895058908,-4.263271520596));
#36851=CARTESIAN_POINT('Ctrl Pts',(0.5699861959056,1.250802378507,-4.313971794172));
#36852=CARTESIAN_POINT('Ctrl Pts',(1.246362050538,0.5796315446648,-4.364672067748));
#36853=CARTESIAN_POINT('Ctrl Pts',(1.32379313679,-0.3700836676636,-4.415372341324));
#36854=CARTESIAN_POINT('Ctrl Pts',(0.7650715766059,-1.141953368097,-4.4660726149));
#36855=CARTESIAN_POINT('Ctrl Pts',(-0.1613139710547,-1.365053843919,-4.516772888476));
#36856=CARTESIAN_POINT('Ctrl Pts',(-1.01015806052,-0.9321679759867,-4.567473162052));
#36857=CARTESIAN_POINT('Ctrl Pts',(-1.37364634578,-0.05134052539036,-4.618173435628));
#36858=CARTESIAN_POINT('Ctrl Pts',(-1.076725604129,0.8542167935132,-4.668873709204));
#36859=CARTESIAN_POINT('Ctrl Pts',(-0.5345691746706,1.184112536844,-4.702673891588));
#36860=CARTESIAN_POINT('Ctrl Pts',(-0.2416963184219,1.241145565899,-4.71957398278));
#36861=CARTESIAN_POINT('',(0.507887877650121,-1.14145688760839,-3.11964125711469));
#36862=CARTESIAN_POINT('Ctrl Pts',(-0.733875647329055,1.01087300651023,
-4.23008257417792));
#36863=CARTESIAN_POINT('Ctrl Pts',(-0.825987121271145,0.94411145872215,
-4.22363001656661));
#36864=CARTESIAN_POINT('Ctrl Pts',(-0.928569855441707,0.851140106664914,
-4.21583740331039));
#36865=CARTESIAN_POINT('Ctrl Pts',(-1.09492055138801,0.617000415853516,
-4.19906379556599));
#36866=CARTESIAN_POINT('Ctrl Pts',(-1.15319261062486,0.49772291024227,-4.1915815901967));
#36867=CARTESIAN_POINT('Ctrl Pts',(-1.23189231323316,0.245489451432284,
-4.17660903244399));
#36868=CARTESIAN_POINT('Ctrl Pts',(-1.25171978917578,0.111810504704931,
-4.16906604902943));
#36869=CARTESIAN_POINT('Ctrl Pts',(-1.24852928233844,-0.096715149384668,
-4.15698096414954));
#36870=CARTESIAN_POINT('Ctrl Pts',(-1.24042793192133,-0.171145972738229,
-4.15260661067975));
#36871=CARTESIAN_POINT('Ctrl Pts',(-1.20903242612985,-0.326144503860473,
-4.14350186866899));
#36872=CARTESIAN_POINT('Ctrl Pts',(-1.18434831837205,-0.405891266492904,
-4.13877985127521));
#36873=CARTESIAN_POINT('Ctrl Pts',(-1.09931321063353,-0.608469106103288,
-4.12632324246702));
#36874=CARTESIAN_POINT('Ctrl Pts',(-1.02613933958735,-0.726105546047824,
-4.11859175537242));
#36875=CARTESIAN_POINT('Ctrl Pts',(-0.889031840281174,-0.881536851166071,
-4.10657357976713));
#36876=CARTESIAN_POINT('Ctrl Pts',(-0.838070882863559,-0.93003158188435,
-4.10245889965596));
#36877=CARTESIAN_POINT('Ctrl Pts',(-0.71804471629122,-1.02598281535047,
-4.09359767136651));
#36878=CARTESIAN_POINT('Ctrl Pts',(-0.647920116788861,-1.07130370486005,
-4.08887034149716));
#36879=CARTESIAN_POINT('Ctrl Pts',(-0.451607190563765,-1.17261984972335,
-4.07634288194066));
#36880=CARTESIAN_POINT('Ctrl Pts',(-0.318735404546458,-1.21605862648864,
-4.06855248872333));
#36881=CARTESIAN_POINT('Ctrl Pts',(-0.116566973731751,-1.24631682178166,
-4.05671455059356));
#36882=CARTESIAN_POINT('Ctrl Pts',(-0.0503947385544985,-1.25072100020528,
-4.0528319962753));
#36883=CARTESIAN_POINT('Ctrl Pts',(0.177200110844515,-1.24723779942647,
-4.03967510971017));
#36884=CARTESIAN_POINT('Ctrl Pts',(0.337818864680723,-1.21310245611501,
-4.03061613897922));
#36885=CARTESIAN_POINT('Ctrl Pts',(0.627325461026085,-1.09155867140617,
-4.01274824690792));
#36886=CARTESIAN_POINT('Ctrl Pts',(0.751113999919971,-1.01028915862942,
-4.0041824455675));
#36887=CARTESIAN_POINT('Ctrl Pts',(0.918980844614885,-0.850590818913521,
-3.99085360498138));
#36888=CARTESIAN_POINT('Ctrl Pts',(0.973415257658214,-0.787286509795003,
-3.98613405120972));
#36889=CARTESIAN_POINT('Ctrl Pts',(1.09889105453754,-0.608894755549359,
-3.97377157854704));
#36890=CARTESIAN_POINT('Ctrl Pts',(1.15913819005378,-0.486012614431139,
-3.96612861225493));
#36891=CARTESIAN_POINT('Ctrl Pts',(1.21926945032107,-0.285379499728559,
-3.95397856946806));
#36892=CARTESIAN_POINT('Ctrl Pts',(1.23392516157266,-0.212698818790114,
-3.94964661234106));
#36893=CARTESIAN_POINT('Ctrl Pts',(1.25097407343862,-0.0562022111640335,
-3.94058370371999));
#36894=CARTESIAN_POINT('Ctrl Pts',(1.25166086109128,0.0272909789852731,
-3.93586148317175));
#36895=CARTESIAN_POINT('Ctrl Pts',(1.23219006522341,0.245418179734663,-3.92344681075619));
#36896=CARTESIAN_POINT('Ctrl Pts',(1.19847382539114,0.379013246675096,-3.9157572839109));
#36897=CARTESIAN_POINT('Ctrl Pts',(1.11540449196199,0.568718283946679,-3.90375051671024));
#36898=CARTESIAN_POINT('Ctrl Pts',(1.08136457923424,0.630911587796264,-3.89960405334492));
#36899=CARTESIAN_POINT('Ctrl Pts',(0.995866667981166,0.759255627291935,
-3.89071275004434));
#36900=CARTESIAN_POINT('Ctrl Pts',(0.94283254918456,0.823743151752923,-3.88598591056034));
#36901=CARTESIAN_POINT('Ctrl Pts',(0.786673071735048,0.979851467190434,
-3.87346473923337));
#36902=CARTESIAN_POINT('Ctrl Pts',(0.673389570842327,1.06156566729279,-3.86567943453108));
#36903=CARTESIAN_POINT('Ctrl Pts',(0.489746229335454,1.15199765544022,-3.85382352758708));
#36904=CARTESIAN_POINT('Ctrl Pts',(0.427675323548356,1.17642765668122,-3.84991855320174));
#36905=CARTESIAN_POINT('Ctrl Pts',(0.209385353179634,1.24222689073648,-3.83674361154985));
#36906=CARTESIAN_POINT('Ctrl Pts',(0.0459967194180074,1.2584201992733,-3.82768643928908));
#36907=CARTESIAN_POINT('Ctrl Pts',(-0.264125856239754,1.23064739634467,
-3.80996546352936));
#36908=CARTESIAN_POINT('Ctrl Pts',(-0.404568568651727,1.19185916584351,
-3.80153535902006));
#36909=CARTESIAN_POINT('Ctrl Pts',(-0.6115300780727,1.09275004242686,-3.78832831044393));
#36910=CARTESIAN_POINT('Ctrl Pts',(-0.682848754794305,1.04933401051589,
-3.78360702519108));
#36911=CARTESIAN_POINT('Ctrl Pts',(-0.857708853406781,0.918031373235897,
-3.77121134160043));
#36912=CARTESIAN_POINT('Ctrl Pts',(-0.953282912340471,0.819253189261027,
-3.76353878693458));
#36913=CARTESIAN_POINT('Ctrl Pts',(-1.07125640891817,0.648176685622839,
-3.75148822550272));
#36914=CARTESIAN_POINT('Ctrl Pts',(-1.10664532108669,0.585546807113655,
-3.74728237147825));
#36915=CARTESIAN_POINT('Ctrl Pts',(-1.17083993611844,0.44419810319016,-3.73833619083301));
#36916=CARTESIAN_POINT('Ctrl Pts',(-1.19756547092642,0.365094147117043,
-3.73361081846715));
#36917=CARTESIAN_POINT('Ctrl Pts',(-1.24744717470402,0.150623842050563,
-3.72112571182027));
#36918=CARTESIAN_POINT('Ctrl Pts',(-1.25702073797125,0.0119166161975678,
-3.71337291257023));
#36919=CARTESIAN_POINT('Ctrl Pts',(-1.23983357350552,-0.163266891536038,
-3.70317452631609));
#36920=CARTESIAN_POINT('Ctrl Pts',(-1.23420088928342,-0.201636096563702,
-3.70091049128662));
#36921=CARTESIAN_POINT('Ctrl Pts',(-1.19602087654215,-0.396264459324683,
-3.68935075162125));
#36922=CARTESIAN_POINT('Ctrl Pts',(-1.13438572831812,-0.546182761234717,
-3.68035352269049));
#36923=CARTESIAN_POINT('Ctrl Pts',(-1.00347591375521,-0.748602659195634,
-3.66668241530662));
#36924=CARTESIAN_POINT('Ctrl Pts',(-0.952126672075524,-0.813359570715913,
-3.66200205495338));
#36925=CARTESIAN_POINT('Ctrl Pts',(-0.844070250943292,-0.924785227570656,
-3.65305173108173));
#36926=CARTESIAN_POINT('Ctrl Pts',(-0.789002477788614,-0.972269596887259,
-3.64879779712052));
#36927=CARTESIAN_POINT('Ctrl Pts',(-0.624132091077882,-1.09030372751535,
-3.63705110011354));
#36928=CARTESIAN_POINT('Ctrl Pts',(-0.506629078599337,-1.14902801670687,
-3.62970604262753));
#36929=CARTESIAN_POINT('Ctrl Pts',(-0.304011928651628,-1.21446751650945,
-3.61763778112587));
#36930=CARTESIAN_POINT('Ctrl Pts',(-0.222329568483162,-1.23230954292719,
-3.61291280107117));
#36931=CARTESIAN_POINT('Ctrl Pts',(0.0120443509726828,-1.25935018450633,
-3.59934542048976));
#36932=CARTESIAN_POINT('Ctrl Pts',(0.16353090081991,-1.24872899180732,-3.59056887251069));
#36933=CARTESIAN_POINT('Ctrl Pts',(0.47078982918158,-1.16796950043995,-3.57249718230263));
#36934=CARTESIAN_POINT('Ctrl Pts',(0.61917907071545,-1.09716798788213,-3.56342436605197));
#36935=CARTESIAN_POINT('Ctrl Pts',(0.803253762053073,-0.960147658502963,
-3.55014885951359));
#36936=CARTESIAN_POINT('Ctrl Pts',(0.854156106363377,-0.915153330275588,
-3.54617101977603));
#36937=CARTESIAN_POINT('Ctrl Pts',(0.994107305067958,-0.768798171891316,
-3.53446084760397));
#36938=CARTESIAN_POINT('Ctrl Pts',(1.07098938598973,-0.656508753343506,
-3.5268721498646));
#36939=CARTESIAN_POINT('Ctrl Pts',(1.16398616596849,-0.460982468107929,
-3.5145932231718));
#36940=CARTESIAN_POINT('Ctrl Pts',(1.1921384149349,-0.383279648853243,-3.50991290675987));
#36941=CARTESIAN_POINT('Ctrl Pts',(1.23024443209663,-0.232777514142283,
-3.50096071108599));
#36942=CARTESIAN_POINT('Ctrl Pts',(1.24174709866166,-0.160943484599564,
-3.49670472743925));
#36943=CARTESIAN_POINT('Ctrl Pts',(1.2556222927149,0.0413592225819834,-3.48495724321245));
#36944=CARTESIAN_POINT('Ctrl Pts',(1.24390126337967,0.17216988600908,-3.47761349197787));
#36945=CARTESIAN_POINT('Ctrl Pts',(1.19321167061787,0.378945395780619,-3.46554665252736));
#36946=CARTESIAN_POINT('Ctrl Pts',(1.16550737804734,0.457830075032333,-3.46082173077236));
#36947=CARTESIAN_POINT('Ctrl Pts',(1.06543134020746,0.671552931208405,-3.44725088042344));
#36948=CARTESIAN_POINT('Ctrl Pts',(0.976799012979039,0.794958674899222,
-3.4384698933436));
#36949=CARTESIAN_POINT('Ctrl Pts',(0.746627562182523,1.01407250609846,-3.42039294242618));
#36950=CARTESIAN_POINT('Ctrl Pts',(0.608440156904095,1.10315982006909,-3.41132009370902));
#36951=CARTESIAN_POINT('Ctrl Pts',(0.395171729154963,1.18782900119653,-3.39804520758731));
#36952=CARTESIAN_POINT('Ctrl Pts',(0.330160405457533,1.2075100217443,-3.39406810295473));
#36953=CARTESIAN_POINT('Ctrl Pts',(0.1321133813571,1.24973963688798,-3.38235795609272));
#36954=CARTESIAN_POINT('Ctrl Pts',(-0.00383399948244982,1.25618895580989,
-3.37476855565622));
#36955=CARTESIAN_POINT('Ctrl Pts',(-0.219075835306222,1.23262930230883,
-3.36248892666366));
#36956=CARTESIAN_POINT('Ctrl Pts',(-0.299983891499242,1.21577450743834,
-3.35780862343938));
#36957=CARTESIAN_POINT('Ctrl Pts',(-0.448065444823204,1.16915519181047,
-3.34885667158477));
#36958=CARTESIAN_POINT('Ctrl Pts',(-0.515231046729565,1.14121643349784,
-3.34460095198795));
#36959=CARTESIAN_POINT('Ctrl Pts',(-0.694686251822005,1.0467633452116,-3.33285263762908));
#36960=CARTESIAN_POINT('Ctrl Pts',(-0.799861433024963,0.968069776518021,
-3.3255077792573));
#36961=CARTESIAN_POINT('Ctrl Pts',(-0.949205482109416,0.816310659286032,
-3.31343970118704));
#36962=CARTESIAN_POINT('Ctrl Pts',(-1.00178021403193,0.75130095133304,-3.30871470497829));
#36963=CARTESIAN_POINT('Ctrl Pts',(-1.13109745576878,0.553855845839041,
-3.29514185041406));
#36964=CARTESIAN_POINT('Ctrl Pts',(-1.18954659813618,0.413603650031076,
-3.2863606214834));
#36965=CARTESIAN_POINT('Ctrl Pts',(-1.25508746532298,0.102680880205581,
-3.26828620334525));
#36966=CARTESIAN_POINT('Ctrl Pts',(-1.25831131853314,-0.0616836932186077,
-3.25921473718692));
#36967=CARTESIAN_POINT('Ctrl Pts',(-1.21839565445701,-0.287349150006394,
-3.24595615898599));
#36968=CARTESIAN_POINT('Ctrl Pts',(-1.20108917791892,-0.352751485571006,
-3.24199464006113));
#36969=CARTESIAN_POINT('Ctrl Pts',(-1.13307736316836,-0.543662137018506,
-3.23027245184088));
#36970=CARTESIAN_POINT('Ctrl Pts',(-1.06695580974336,-0.663144382443532,
-3.22265656378173));
#36971=CARTESIAN_POINT('Ctrl Pts',(-0.933540585090504,-0.834199642533942,
-3.21035259237703));
#36972=CARTESIAN_POINT('Ctrl Pts',(-0.876705080832201,-0.894150450270504,
-3.20567407636957));
#36973=CARTESIAN_POINT('Ctrl Pts',(-0.758456158600062,-0.996296398557068,
-3.19666510759818));
#36974=CARTESIAN_POINT('Ctrl Pts',(-0.698494311599007,-1.03928012010615,
-3.19235006994326));
#36975=CARTESIAN_POINT('Ctrl Pts',(-0.523367366197831,-1.14197893838959,
-3.18060044677048));
#36976=CARTESIAN_POINT('Ctrl Pts',(-0.401869693488511,-1.18960829308796,
-3.17330940046633));
#36977=CARTESIAN_POINT('Ctrl Pts',(-0.147861403149484,-1.24735560422784,
-3.15854913541049));
#36978=CARTESIAN_POINT('Ctrl Pts',(-0.0146749456347816,-1.25678959869051,
-3.15102599048014));
#36979=CARTESIAN_POINT('Ctrl Pts',(0.272063010777239,-1.22990832794888,
-3.1342070007271));
#36980=CARTESIAN_POINT('Ctrl Pts',(0.403920008211813,-1.18762497665319,
-3.12641288451799));
#36981=CARTESIAN_POINT('Ctrl Pts',(0.507833268109246,-1.14129009144715,
-3.11995951443803));
#36982=CARTESIAN_POINT('',(0.394326187196951,-0.886231714570047,-2.95835875076991));
#36983=CARTESIAN_POINT('',(0.3943262306718,-0.8862318115506,-2.958358760073));
#36984=CARTESIAN_POINT('Ctrl Pts',(0.394086490514282,-0.885697016523154,
-2.95834297351496));
#36985=CARTESIAN_POINT('Ctrl Pts',(0.298191958553152,-0.928570355423577,
-2.96609912828714));
#36986=CARTESIAN_POINT('Ctrl Pts',(0.178519160258169,-0.964221383078607,
-2.97515342193901));
#36987=CARTESIAN_POINT('Ctrl Pts',(-0.0910893742334601,-0.973481439942689,
-2.99509288425242));
#36988=CARTESIAN_POINT('Ctrl Pts',(-0.219578006005614,-0.952478120502751,
-3.00451358328581));
#36989=CARTESIAN_POINT('Ctrl Pts',(-0.459314331859836,-0.863779587384766,
-3.02338810787862));
#36990=CARTESIAN_POINT('Ctrl Pts',(-0.567630710127548,-0.796933539091375,
-3.03262261216431));
#36991=CARTESIAN_POINT('Ctrl Pts',(-0.752828485440924,-0.623184054868312,
-3.05137670238496));
#36992=CARTESIAN_POINT('Ctrl Pts',(-0.828023420909123,-0.519426122579509,
-3.06065415106238));
#36993=CARTESIAN_POINT('Ctrl Pts',(-0.94255521282042,-0.272657343323878,
-3.08075567571069));
#36994=CARTESIAN_POINT('Ctrl Pts',(-0.964576092397812,-0.146345569842894,
-3.09003837605877));
#36995=CARTESIAN_POINT('Ctrl Pts',(-0.973234758229752,0.085059333000687,
-3.10713095999206));
#36996=CARTESIAN_POINT('Ctrl Pts',(-0.954764421553844,0.20944375937905,
-3.11624459210594));
#36997=CARTESIAN_POINT('Ctrl Pts',(-0.863385541083935,0.46753846278374,
-3.13648573502703));
#36998=CARTESIAN_POINT('Ctrl Pts',(-0.787741201038068,0.574355926245695,
-3.14594494376442));
#36999=CARTESIAN_POINT('Ctrl Pts',(-0.636563258090311,0.740825101047974,
-3.16253912703327));
#37000=CARTESIAN_POINT('Ctrl Pts',(-0.538712695870463,0.815657266700886,
-3.17147840984227));
#37001=CARTESIAN_POINT('Ctrl Pts',(-0.314574481362823,0.926631232436044,
-3.18997228883889));
#37002=CARTESIAN_POINT('Ctrl Pts',(-0.187145566187846,0.959632056663,-3.19950140358805));
#37003=CARTESIAN_POINT('Ctrl Pts',(0.0437158535439797,0.973816785682933,
-3.21657049099738));
#37004=CARTESIAN_POINT('Ctrl Pts',(0.169857833048983,0.966145605389418,
-3.22571908778702));
#37005=CARTESIAN_POINT('Ctrl Pts',(0.428395654897745,0.879230744200447,
-3.24588254217937));
#37006=CARTESIAN_POINT('Ctrl Pts',(0.541693017629161,0.813745168936603,
-3.25535199002771));
#37007=CARTESIAN_POINT('Ctrl Pts',(0.734982717893058,0.645443410637272,
-3.27427218637866));
#37008=CARTESIAN_POINT('Ctrl Pts',(0.811636406380411,0.546422715832138,
-3.28335553035938));
#37009=CARTESIAN_POINT('Ctrl Pts',(0.924128601451263,0.318615613830104,
-3.30212531517517));
#37010=CARTESIAN_POINT('Ctrl Pts',(0.958033338094726,0.193919701721441,
-3.3114780528541));
#37011=CARTESIAN_POINT('Ctrl Pts',(0.978749172687539,-0.0892851067193594,
-3.33245310431301));
#37012=CARTESIAN_POINT('Ctrl Pts',(0.950086443151063,-0.216174344769085,
-3.34185474483205));
#37013=CARTESIAN_POINT('Ctrl Pts',(0.88012689003466,-0.424386369963139,
-3.35807168820761));
#37014=CARTESIAN_POINT('Ctrl Pts',(0.817947883267627,-0.535142012129366,
-3.36727185345121));
#37015=CARTESIAN_POINT('Ctrl Pts',(0.641552013655261,-0.742759599885964,
-3.38740750684635));
#37016=CARTESIAN_POINT('Ctrl Pts',(0.534674148075231,-0.815680064014305,
-3.39676783386907));
#37017=CARTESIAN_POINT('Ctrl Pts',(0.330664337416998,-0.919167120470599,
-3.41365034567614));
#37018=CARTESIAN_POINT('Ctrl Pts',(0.211227470815188,-0.954389957357228,
-3.42268045441736));
#37019=CARTESIAN_POINT('Ctrl Pts',(-0.0704569008974092,-0.980883123973585,
-3.44359987857669));
#37020=CARTESIAN_POINT('Ctrl Pts',(-0.203914130061244,-0.952161421978621,
-3.45343850897055));
#37021=CARTESIAN_POINT('Ctrl Pts',(-0.36958016759548,-0.899678213762177,
-3.46626238060016));
#37022=CARTESIAN_POINT('Ctrl Pts',(-0.490729761001405,-0.85200117158237,
-3.4756482875348));
#37023=CARTESIAN_POINT('Ctrl Pts',(-0.713516101842884,-0.669284725414487,
-3.49695224089473));
#37024=CARTESIAN_POINT('Ctrl Pts',(-0.796210772486554,-0.567271827168219,
-3.50645607377617));
#37025=CARTESIAN_POINT('Ctrl Pts',(-0.906615489405553,-0.359724464965967,
-3.52380729215184));
#37026=CARTESIAN_POINT('Ctrl Pts',(-0.950884825918708,-0.240943001075831,
-3.53298809551321));
#37027=CARTESIAN_POINT('Ctrl Pts',(-0.977297097691617,0.0296841041748267,
-3.55308261030826));
#37028=CARTESIAN_POINT('Ctrl Pts',(-0.964454925062392,0.159120292206585,
-3.56249514560412));
#37029=CARTESIAN_POINT('Ctrl Pts',(-0.891014447070674,0.40408756742219,
-3.58138007083618));
#37030=CARTESIAN_POINT('Ctrl Pts',(-0.830998255952594,0.516453374987395,
-3.59062207519904));
#37031=CARTESIAN_POINT('Ctrl Pts',(-0.669226084533194,0.712159990286071,
-3.60937318861775));
#37032=CARTESIAN_POINT('Ctrl Pts',(-0.570521723227346,0.793670410863386,
-3.61864169031169));
#37033=CARTESIAN_POINT('Ctrl Pts',(-0.331511437622609,0.923522973270035,
-3.63874084829215));
#37034=CARTESIAN_POINT('Ctrl Pts',(-0.206724568934881,0.953433421673881,
-3.64803061038475));
#37035=CARTESIAN_POINT('Ctrl Pts',(0.0234203099571745,0.976651850922853,
-3.66510410729054));
#37036=CARTESIAN_POINT('Ctrl Pts',(0.148589513594781,0.966110048972658,
-3.67420837961276));
#37037=CARTESIAN_POINT('Ctrl Pts',(0.412125331987649,0.891213160371829,
-3.69446296475668));
#37038=CARTESIAN_POINT('Ctrl Pts',(0.523612092796829,0.822292732945887,
-3.70393408344633));
#37039=CARTESIAN_POINT('Ctrl Pts',(0.698976608829793,0.682239902879797,
-3.72049547224334));
#37040=CARTESIAN_POINT('Ctrl Pts',(0.77978007351188,0.589452244916243,-3.72942491066296));
#37041=CARTESIAN_POINT('Ctrl Pts',(0.900594156247188,0.380054045915021,
-3.7473010272067));
#37042=CARTESIAN_POINT('Ctrl Pts',(0.940480498058542,0.263658903783144,
-3.75623046562625));
#37043=CARTESIAN_POINT('Ctrl Pts',(0.973957141473117,0.041742651474511,
-3.77279185442322));
#37044=CARTESIAN_POINT('Ctrl Pts',(0.977823610664811,-0.0892702241076244,
-3.7822629731128));
#37045=CARTESIAN_POINT('Ctrl Pts',(0.910762191275745,-0.354908017969238,
-3.80251755825678));
#37046=CARTESIAN_POINT('Ctrl Pts',(0.857240266408211,-0.468547195571489,
-3.8116218305791));
#37047=CARTESIAN_POINT('Ctrl Pts',(0.721949794241172,-0.656169819148452,
-3.82869532748499));
#37048=CARTESIAN_POINT('Ctrl Pts',(0.633598447246363,-0.74923128810756,
-3.83798508957765));
#37049=CARTESIAN_POINT('Ctrl Pts',(0.401554241019619,-0.891157645578996,
-3.85808424755821));
#37050=CARTESIAN_POINT('Ctrl Pts',(0.281585702576723,-0.935812425696929,
-3.86735274925221));
#37051=CARTESIAN_POINT('Ctrl Pts',(0.0311879332374879,-0.97791078465937,
-3.88610386267095));
#37052=CARTESIAN_POINT('Ctrl Pts',(-0.0961293116754427,-0.973628606025544,
-3.89534586703381));
#37053=CARTESIAN_POINT('Ctrl Pts',(-0.344962787881534,-0.914600046384474,
-3.91423079226578));
#37054=CARTESIAN_POINT('Ctrl Pts',(-0.463447383824371,-0.860933961244311,
-3.92364332756156));
#37055=CARTESIAN_POINT('Ctrl Pts',(-0.684518196277557,-0.702616766733428,
-3.94373784235656));
#37056=CARTESIAN_POINT('Ctrl Pts',(-0.765193847051333,-0.60484023738499,
-3.95291864571793));
#37057=CARTESIAN_POINT('Ctrl Pts',(-0.889615581919422,-0.405380113632132,
-3.97026986409359));
#37058=CARTESIAN_POINT('Ctrl Pts',(-0.936541938784192,-0.282730380681453,
-3.97977369697504));
#37059=CARTESIAN_POINT('Ctrl Pts',(-0.983218772209112,0.00159395276037342,
-4.00107765033499));
#37060=CARTESIAN_POINT('Ctrl Pts',(-0.963857842098935,0.13033974383224,
-4.01046355726967));
#37061=CARTESIAN_POINT('Ctrl Pts',(-0.926376886725788,0.300030347936233,
-4.02328742889928));
#37062=CARTESIAN_POINT('Ctrl Pts',(-0.884445642428363,0.429943930495125,
-4.03312605929319));
#37063=CARTESIAN_POINT('Ctrl Pts',(-0.720524154999485,0.660546877362451,
-4.05404548345253));
#37064=CARTESIAN_POINT('Ctrl Pts',(-0.63025142976455,0.746317783972133,
-4.06307559219369));
#37065=CARTESIAN_POINT('Ctrl Pts',(-0.438550717880826,0.87113929959349,
-4.07995810400068));
#37066=CARTESIAN_POINT('Ctrl Pts',(-0.32192786341835,0.92716948839055,-4.08931843102333));
#37067=CARTESIAN_POINT('Ctrl Pts',(-0.053899100625622,0.975966495244121,
-4.10945408441848));
#37068=CARTESIAN_POINT('Ctrl Pts',(0.0731066818806321,0.974362636104428,
-4.11865424966214));
#37069=CARTESIAN_POINT('Ctrl Pts',(0.288377749580686,0.930716858309793,
-4.13487119303781));
#37070=CARTESIAN_POINT('Ctrl Pts',(0.412575699626238,0.892021897374435,
-4.14427283355689));
#37071=CARTESIAN_POINT('Ctrl Pts',(0.647386542142391,0.732341035767536,
-4.16524788501576));
#37072=CARTESIAN_POINT('Ctrl Pts',(0.738370090523778,0.640577232514665,
-4.17460062269466));
#37073=CARTESIAN_POINT('Ctrl Pts',(0.879286517416562,0.429169734287967,
-4.19337040751045));
#37074=CARTESIAN_POINT('Ctrl Pts',(0.926645994771919,0.313247493699817,
-4.20245375149114));
#37075=CARTESIAN_POINT('Ctrl Pts',(0.975606909619788,0.0616740076335012,
-4.22137394784201));
#37076=CARTESIAN_POINT('Ctrl Pts',(0.975593497086551,-0.0691871890201323,
-4.23084339569034));
#37077=CARTESIAN_POINT('Ctrl Pts',(0.921437955672763,-0.336513161862343,
-4.2510068500827));
#37078=CARTESIAN_POINT('Ctrl Pts',(0.864943960511507,-0.449557730556668,
-4.26015544687236));
#37079=CARTESIAN_POINT('Ctrl Pts',(0.737115611443266,-0.642322132956235,
-4.27722453428169));
#37080=CARTESIAN_POINT('Ctrl Pts',(0.644766461351629,-0.736124144126932,
-4.28675364903085));
#37081=CARTESIAN_POINT('Ctrl Pts',(0.436509652621514,-0.874624187055261,
-4.30524752802741));
#37082=CARTESIAN_POINT('Ctrl Pts',(0.322750023297326,-0.921882332163208,
-4.31418681083635));
#37083=CARTESIAN_POINT('Ctrl Pts',(0.102966529943006,-0.969442532354417,
-4.33078099410514));
#37084=CARTESIAN_POINT('Ctrl Pts',(-0.0273693659811713,-0.981467128609303,
-4.34024020284249));
#37085=CARTESIAN_POINT('Ctrl Pts',(-0.296545998415826,-0.931398013650124,
-4.36048134576363));
#37086=CARTESIAN_POINT('Ctrl Pts',(-0.413474071476687,-0.885132858374172,
-4.36959497787757));
#37087=CARTESIAN_POINT('Ctrl Pts',(-0.609474827808156,-0.761816577731484,
-4.38668756181092));
#37088=CARTESIAN_POINT('Ctrl Pts',(-0.707805253771892,-0.679532250019475,
-4.39597026215903));
#37089=CARTESIAN_POINT('Ctrl Pts',(-0.864116564177007,-0.45686852146669,
-4.41607178680735));
#37090=CARTESIAN_POINT('Ctrl Pts',(-0.91630733566222,-0.339838139921241,
-4.42534923548476));
#37091=CARTESIAN_POINT('Ctrl Pts',(-0.974034598054683,-0.0925434525026679,
-4.44410332570542));
#37092=CARTESIAN_POINT('Ctrl Pts',(-0.977692016570372,0.0346864781869573,
-4.45333782999112));
#37093=CARTESIAN_POINT('Ctrl Pts',(-0.934490971108565,0.286628148782353,
-4.47221235458392));
#37094=CARTESIAN_POINT('Ctrl Pts',(-0.888364507480827,0.40837714169557,
-4.48163305361731));
#37095=CARTESIAN_POINT('Ctrl Pts',(-0.745406355841484,0.637150936261831,
-4.50157251205056));
#37096=CARTESIAN_POINT('Ctrl Pts',(-0.654644885472509,0.722911764031138,
-4.51062680283025));
#37097=CARTESIAN_POINT('Ctrl Pts',(-0.569532054520997,0.784472183292758,
-4.51838295576791));
#37098=CARTESIAN_POINT('Ctrl Pts',(0.9535275674129,-0.8304484356495,-2.630468105836));
#37099=CARTESIAN_POINT('Ctrl Pts',(0.7575668259831,-1.055452133727,-2.647368197028));
#37100=CARTESIAN_POINT('Ctrl Pts',(0.200611625078,-1.359698250639,-2.681168379412));
#37101=CARTESIAN_POINT('Ctrl Pts',(-0.7319692574172,-1.163512414639,-2.731868652988));
#37102=CARTESIAN_POINT('Ctrl Pts',(-1.312600153974,-0.4079672517203,-2.782568926564));
#37103=CARTESIAN_POINT('Ctrl Pts',(-1.262509073048,0.543566954962,-2.83326920014));
#37104=CARTESIAN_POINT('Ctrl Pts',(-0.6056998170625,1.233904268511,-2.883969473716));
#37105=CARTESIAN_POINT('Ctrl Pts',(0.3421771199694,1.331279463018,-2.934669747292));
#37106=CARTESIAN_POINT('Ctrl Pts',(1.125620475753,0.7889040709467,-2.985370020868));
#37107=CARTESIAN_POINT('Ctrl Pts',(1.368142054503,-0.1325826998597,-3.036070294444));
#37108=CARTESIAN_POINT('Ctrl Pts',(0.9531974730936,-0.9903562298753,-3.08677056802));
#37109=CARTESIAN_POINT('Ctrl Pts',(0.08018994585494,-1.372210064652,-3.137470841596));
#37110=CARTESIAN_POINT('Ctrl Pts',(-0.8313531810178,-1.094642760639,-3.188171115172));
#37111=CARTESIAN_POINT('Ctrl Pts',(-1.343386153806,-0.2910404234365,-3.238871388748));
#37112=CARTESIAN_POINT('Ctrl Pts',(-1.209849441198,0.6524225744844,-3.289571662324));
#37113=CARTESIAN_POINT('Ctrl Pts',(-0.4949146545354,1.282361248166,-3.3402719359));
#37114=CARTESIAN_POINT('Ctrl Pts',(0.4578533841451,1.296056003695,-3.390972209476));
#37115=CARTESIAN_POINT('Ctrl Pts',(1.190598115186,0.6869257705116,-3.441672483052));
#37116=CARTESIAN_POINT('Ctrl Pts',(1.351196075161,-0.2523094381015,-3.492372756628));
#37117=CARTESIAN_POINT('Ctrl Pts',(0.8624712606077,-1.070296319109,-3.543073030204));
#37118=CARTESIAN_POINT('Ctrl Pts',(-0.04071762923338,-1.373947946879,-3.59377330378));
#37119=CARTESIAN_POINT('Ctrl Pts',(-0.9243394967408,-1.017343295588,-3.644473577356));
#37120=CARTESIAN_POINT('Ctrl Pts',(-1.363766255618,-0.1718501819773,-3.695173850932));
#37121=CARTESIAN_POINT('Ctrl Pts',(-1.147829590707,0.7562262357563,-3.745874124508));
#37122=CARTESIAN_POINT('Ctrl Pts',(-0.3802987353604,1.320895058908,-3.796574398084));
#37123=CARTESIAN_POINT('Ctrl Pts',(0.5699861959056,1.250802378507,-3.84727467166));
#37124=CARTESIAN_POINT('Ctrl Pts',(1.246362050538,0.5796315446648,-3.897974945236));
#37125=CARTESIAN_POINT('Ctrl Pts',(1.32379313679,-0.3700836676636,-3.948675218812));
#37126=CARTESIAN_POINT('Ctrl Pts',(0.7650715766059,-1.141953368097,-3.999375492388));
#37127=CARTESIAN_POINT('Ctrl Pts',(-0.1613139710547,-1.365053843919,-4.050075765964));
#37128=CARTESIAN_POINT('Ctrl Pts',(-1.01015806052,-0.9321679759867,-4.10077603954));
#37129=CARTESIAN_POINT('Ctrl Pts',(-1.37364634578,-0.05134052539036,-4.151476313116));
#37130=CARTESIAN_POINT('Ctrl Pts',(-1.076725604129,0.8542167935132,-4.202176586692));
#37131=CARTESIAN_POINT('Ctrl Pts',(-0.5345691746706,1.184112536844,-4.235976769076));
#37132=CARTESIAN_POINT('Ctrl Pts',(-0.2416963184219,1.241145565899,-4.252876860268));
#37133=CARTESIAN_POINT('Ctrl Pts',(0.8758754583306,-0.7628194811062,-2.689919838464));
#37134=CARTESIAN_POINT('Ctrl Pts',(0.6958731069771,-0.9694996274544,-2.706819929656));
#37135=CARTESIAN_POINT('Ctrl Pts',(0.1842744825284,-1.248968953987,-2.74062011204));
#37136=CARTESIAN_POINT('Ctrl Pts',(-0.6723601191349,-1.068759839016,-2.791320385616));
#37137=CARTESIAN_POINT('Ctrl Pts',(-1.20570636944,-0.3747437575968,-2.842020659192));
#37138=CARTESIAN_POINT('Ctrl Pts',(-1.159694539302,0.4993006726617,-2.892720932768));
#37139=CARTESIAN_POINT('Ctrl Pts',(-0.5563736414247,1.133419214769,-2.943421206344));
#37140=CARTESIAN_POINT('Ctrl Pts',(0.314311355042,1.222864497773,-2.99412147992));
#37141=CARTESIAN_POINT('Ctrl Pts',(1.033953693422,0.7246583510889,-3.044821753496));
#37142=CARTESIAN_POINT('Ctrl Pts',(1.256725122589,-0.1217856063893,-3.095522027072));
#37143=CARTESIAN_POINT('Ctrl Pts',(0.8755722457931,-0.9097049171909,-3.146222300648));
#37144=CARTESIAN_POINT('Ctrl Pts',(0.07365954376103,-1.260461847542,-3.196922574224));
#37145=CARTESIAN_POINT('Ctrl Pts',(-0.7636505470253,-1.005498700247,-3.2476228478));
#37146=CARTESIAN_POINT('Ctrl Pts',(-1.233985259988,-0.2673390607487,-3.298323121376));
#37147=CARTESIAN_POINT('Ctrl Pts',(-1.111323332471,0.5992914531062,-3.349023394952));
#37148=CARTESIAN_POINT('Ctrl Pts',(-0.4546104535308,1.177930019402,-3.399723668528));
#37149=CARTESIAN_POINT('Ctrl Pts',(0.4205673295575,1.190509519655,-3.450423942104));
#37150=CARTESIAN_POINT('Ctrl Pts',(1.093639770328,0.6309848237721,-3.50112421568));
#37151=CARTESIAN_POINT('Ctrl Pts',(1.241159167361,-0.2317621978543,-3.551824489256));
#37152=CARTESIAN_POINT('Ctrl Pts',(0.7922344738614,-0.9831349518212,-3.602524762832));
#37153=CARTESIAN_POINT('Ctrl Pts',(-0.03740172113081,-1.262058202429,-3.653225036408));
#37154=CARTESIAN_POINT('Ctrl Pts',(-0.8490643669144,-0.9344942461601,-3.703925309984));
#37155=CARTESIAN_POINT('Ctrl Pts',(-1.252705674191,-0.1578552755553,-3.75462558356));
#37156=CARTESIAN_POINT('Ctrl Pts',(-1.054354172029,0.6946416899531,-3.805325857136));
#37157=CARTESIAN_POINT('Ctrl Pts',(-0.3493284730509,1.213325764945,-3.856026130712));
#37158=CARTESIAN_POINT('Ctrl Pts',(0.5235684186199,1.148941198972,-3.906726404288));
#37159=CARTESIAN_POINT('Ctrl Pts',(1.144862476522,0.5324282823029,-3.957426677864));
#37160=CARTESIAN_POINT('Ctrl Pts',(1.215987833017,-0.3399452864431,-4.00812695144));
#37161=CARTESIAN_POINT('Ctrl Pts',(0.702766695706,-1.048956489416,-4.058827225016));
#37162=CARTESIAN_POINT('Ctrl Pts',(-0.1481770985562,-1.253888405589,-4.109527498592));
#37163=CARTESIAN_POINT('Ctrl Pts',(-0.9278941527034,-0.8562553208856,-4.160227772168));
#37164=CARTESIAN_POINT('Ctrl Pts',(-1.261781162719,-0.04715952400749,-4.210928045744));
#37165=CARTESIAN_POINT('Ctrl Pts',(-0.9890406572845,0.7846522230731,-4.26162831932));
#37166=CARTESIAN_POINT('Ctrl Pts',(-0.4910356416274,1.087682355883,-4.295428501704));
#37167=CARTESIAN_POINT('Ctrl Pts',(-0.2220133752913,1.140070805017,-4.312328592896));
#37168=CARTESIAN_POINT('Ctrl Pts',(0.7982233492482,-0.6951905265629,-2.749371571093));
#37169=CARTESIAN_POINT('Ctrl Pts',(0.6341793879712,-0.8835471211815,-2.766271662285));
#37170=CARTESIAN_POINT('Ctrl Pts',(0.1679373399789,-1.138239657336,-2.800071844669));
#37171=CARTESIAN_POINT('Ctrl Pts',(-0.6127509808526,-0.9740072633923,-2.850772118245));
#37172=CARTESIAN_POINT('Ctrl Pts',(-1.098812584906,-0.3415202634732,-2.901472391821));
#37173=CARTESIAN_POINT('Ctrl Pts',(-1.056880005555,0.4550343903613,-2.952172665397));
#37174=CARTESIAN_POINT('Ctrl Pts',(-0.5070474657869,1.032934161028,-3.002872938973));
#37175=CARTESIAN_POINT('Ctrl Pts',(0.2864455901145,1.114449532528,-3.053573212549));
#37176=CARTESIAN_POINT('Ctrl Pts',(0.9422869110915,0.6604126312312,-3.104273486125));
#37177=CARTESIAN_POINT('Ctrl Pts',(1.145308190676,-0.1109885129189,-3.154973759701));
#37178=CARTESIAN_POINT('Ctrl Pts',(0.7979470184926,-0.8290536045064,-3.205674033277));
#37179=CARTESIAN_POINT('Ctrl Pts',(0.06712914166712,-1.148713630431,-3.256374306853));
#37180=CARTESIAN_POINT('Ctrl Pts',(-0.6959479130327,-0.9163546398542,-3.307074580429));
#37181=CARTESIAN_POINT('Ctrl Pts',(-1.12458436617,-0.2436376980609,-3.357774854005));
#37182=CARTESIAN_POINT('Ctrl Pts',(-1.012797223744,0.546160331728,-3.408475127581));
#37183=CARTESIAN_POINT('Ctrl Pts',(-0.4143062525262,1.073498790637,-3.459175401157));
#37184=CARTESIAN_POINT('Ctrl Pts',(0.3832812749699,1.084963035615,-3.509875674733));
#37185=CARTESIAN_POINT('Ctrl Pts',(0.9966814254686,0.5750438770327,-3.560575948309));
#37186=CARTESIAN_POINT('Ctrl Pts',(1.131122259562,-0.2112149576071,-3.611276221885));
#37187=CARTESIAN_POINT('Ctrl Pts',(0.7219976871151,-0.8959735845339,-3.661976495461));
#37188=CARTESIAN_POINT('Ctrl Pts',(-0.03408581302824,-1.150168457978,-3.712676769037));
#37189=CARTESIAN_POINT('Ctrl Pts',(-0.773789237088,-0.8516451967325,-3.763377042613));
#37190=CARTESIAN_POINT('Ctrl Pts',(-1.141645092763,-0.1438603691333,-3.814077316189));
#37191=CARTESIAN_POINT('Ctrl Pts',(-0.9608787533499,0.63305714415,-3.864777589765));
#37192=CARTESIAN_POINT('Ctrl Pts',(-0.3183582107415,1.105756470983,-3.915477863341));
#37193=CARTESIAN_POINT('Ctrl Pts',(0.4771506413343,1.047080019436,-3.966178136917));
#37194=CARTESIAN_POINT('Ctrl Pts',(1.043362902507,0.485225019941,-4.016878410493));
#37195=CARTESIAN_POINT('Ctrl Pts',(1.108182529245,-0.3098069052225,-4.067578684069));
#37196=CARTESIAN_POINT('Ctrl Pts',(0.6404618148061,-0.9559596107337,-4.118278957645));
#37197=CARTESIAN_POINT('Ctrl Pts',(-0.1350402260578,-1.142722967259,-4.168979231221));
#37198=CARTESIAN_POINT('Ctrl Pts',(-0.8456302448871,-0.7803426657845,-4.219679504797));
#37199=CARTESIAN_POINT('Ctrl Pts',(-1.149915979657,-0.04297852262462,-4.270379778373));
#37200=CARTESIAN_POINT('Ctrl Pts',(-0.9013557104398,0.715087652633,-4.321080051949));
#37201=CARTESIAN_POINT('Ctrl Pts',(-0.4475021085842,0.9912521749224,-4.354880234333));
#37202=CARTESIAN_POINT('Ctrl Pts',(-0.2023304321606,1.038996044136,-4.371780325525));
#37203=CARTESIAN_POINT('Ctrl Pts',(0.7205712401658,-0.6275615720196,-2.808823303721));
#37204=CARTESIAN_POINT('Ctrl Pts',(0.5724856689652,-0.7975946149087,-2.825723394913));
#37205=CARTESIAN_POINT('Ctrl Pts',(0.1516001974293,-1.027510360684,-2.859523577297));
#37206=CARTESIAN_POINT('Ctrl Pts',(-0.5531418425703,-0.879254687769,-2.910223850873));
#37207=CARTESIAN_POINT('Ctrl Pts',(-0.9919188003728,-0.3082967693496,-2.960924124449));
#37208=CARTESIAN_POINT('Ctrl Pts',(-0.9540654718091,0.4107681080609,-3.011624398025));
#37209=CARTESIAN_POINT('Ctrl Pts',(-0.4577212901491,0.9324491072861,-3.062324671601));
#37210=CARTESIAN_POINT('Ctrl Pts',(0.2585798251871,1.006034567282,-3.113024945177));
#37211=CARTESIAN_POINT('Ctrl Pts',(0.8506201287607,0.5961669113734,-3.163725218753));
#37212=CARTESIAN_POINT('Ctrl Pts',(1.033891258762,-0.1001914194485,-3.214425492329));
#37213=CARTESIAN_POINT('Ctrl Pts',(0.7203217911921,-0.7484022918219,-3.265125765905));
#37214=CARTESIAN_POINT('Ctrl Pts',(0.06059873957321,-1.03696541332,-3.315826039481));
#37215=CARTESIAN_POINT('Ctrl Pts',(-0.6282452790402,-0.8272105794617,-3.366526313057));
#37216=CARTESIAN_POINT('Ctrl Pts',(-1.015183472352,-0.2199363353731,-3.417226586633));
#37217=CARTESIAN_POINT('Ctrl Pts',(-0.914271115017,0.4930292103498,-3.467926860209));
#37218=CARTESIAN_POINT('Ctrl Pts',(-0.3740020515216,0.969067561873,-3.518627133785));
#37219=CARTESIAN_POINT('Ctrl Pts',(0.3459952203822,0.9794165515745,-3.569327407361));
#37220=CARTESIAN_POINT('Ctrl Pts',(0.8997230806097,0.5191029302932,-3.620027680937));
#37221=CARTESIAN_POINT('Ctrl Pts',(1.021085351762,-0.1906677173599,-3.670727954513));
#37222=CARTESIAN_POINT('Ctrl Pts',(0.6517609003688,-0.8088122172466,-3.721428228089));
#37223=CARTESIAN_POINT('Ctrl Pts',(-0.03076990492567,-1.038278713527,-3.772128501665));
#37224=CARTESIAN_POINT('Ctrl Pts',(-0.6985141072616,-0.7687961473049,-3.822828775241));
#37225=CARTESIAN_POINT('Ctrl Pts',(-1.030584511335,-0.1298654627114,-3.873529048817));
#37226=CARTESIAN_POINT('Ctrl Pts',(-0.8674033346712,0.5714725983469,-3.924229322393));
#37227=CARTESIAN_POINT('Ctrl Pts',(-0.287387948432,0.9981871770197,-3.974929595969));
#37228=CARTESIAN_POINT('Ctrl Pts',(0.4307328640486,0.9452188399008,-4.025629869545));
#37229=CARTESIAN_POINT('Ctrl Pts',(0.9418633284912,0.4380217575791,-4.076330143121));
#37230=CARTESIAN_POINT('Ctrl Pts',(1.000377225472,-0.2796685240019,-4.127030416697));
#37231=CARTESIAN_POINT('Ctrl Pts',(0.5781569339062,-0.8629627320519,-4.177730690273));
#37232=CARTESIAN_POINT('Ctrl Pts',(-0.1219033535594,-1.031557528929,-4.228430963849));
#37233=CARTESIAN_POINT('Ctrl Pts',(-0.7633663370709,-0.7044300106834,-4.279131237425));
#37234=CARTESIAN_POINT('Ctrl Pts',(-1.038050796595,-0.03879752124175,-4.329831511001));
#37235=CARTESIAN_POINT('Ctrl Pts',(-0.813670763595,0.6455230821929,-4.380531784577));
#37236=CARTESIAN_POINT('Ctrl Pts',(-0.4039685755409,0.8948219939615,-4.414331966961));
#37237=CARTESIAN_POINT('Ctrl Pts',(-0.1826474890299,0.9379212832541,-4.431232058153));
#37238=CARTESIAN_POINT('',(0.507887874041584,-1.14145688922471,-2.67039241379527));
#37239=CARTESIAN_POINT('Ctrl Pts',(0.507787909469119,-1.14128017477199,
-2.6700583582432));
#37240=CARTESIAN_POINT('Ctrl Pts',(0.430345474071355,-1.17582998645329,
-2.67495591326481));
#37241=CARTESIAN_POINT('Ctrl Pts',(0.349428371731934,-1.20267898189871,
-2.67984218562302));
#37242=CARTESIAN_POINT('Ctrl Pts',(0.184938905475354,-1.23906261135245,
-2.68944881298632));
#37243=CARTESIAN_POINT('Ctrl Pts',(0.102310644116143,-1.24862692557046,
-2.69408879403421));
#37244=CARTESIAN_POINT('Ctrl Pts',(-0.0377210139794821,-1.25032976147046,
-2.7020683174102));
#37245=CARTESIAN_POINT('Ctrl Pts',(-0.094059933784565,-1.24715139756305,
-2.70529937078892));
#37246=CARTESIAN_POINT('Ctrl Pts',(-0.308267034047177,-1.22069996486095,
-2.71773100546558));
#37247=CARTESIAN_POINT('Ctrl Pts',(-0.46323804104122,-1.17121720337973,
-2.72703107911372));
#37248=CARTESIAN_POINT('Ctrl Pts',(-0.672084377225763,-1.05687339674042,
-2.74061849897817));
#37249=CARTESIAN_POINT('Ctrl Pts',(-0.736631740802832,-1.0129562977045,
-2.74498450329827));
#37250=CARTESIAN_POINT('Ctrl Pts',(-0.860062651533776,-0.910226860245701,
-2.75414203962238));
#37251=CARTESIAN_POINT('Ctrl Pts',(-0.917846632144435,-0.851459146178509,
-2.75886595102978));
#37252=CARTESIAN_POINT('Ctrl Pts',(-1.06655239892433,-0.667895772520611,
-2.77250428977867));
#37253=CARTESIAN_POINT('Ctrl Pts',(-1.14207490333669,-0.530236824079974,
-2.78145769204167));
#37254=CARTESIAN_POINT('Ctrl Pts',(-1.21457005475945,-0.306572310540857,
-2.79479482811465));
#37255=CARTESIAN_POINT('Ctrl Pts',(-1.23157071309401,-0.227763492778128,
-2.79932084856198));
#37256=CARTESIAN_POINT('Ctrl Pts',(-1.25941838893502,0.0125005131581018,
-2.81317763140942));
#37257=CARTESIAN_POINT('Ctrl Pts',(-1.24693178471565,0.176576540746456,
-2.82258473910004));
#37258=CARTESIAN_POINT('Ctrl Pts',(-1.1841615241506,0.406933361119969,-2.8362949159062));
#37259=CARTESIAN_POINT('Ctrl Pts',(-1.15687979077424,0.479766542899355,
-2.84069774142107));
#37260=CARTESIAN_POINT('Ctrl Pts',(-1.04698062949429,0.704023621238008,
-2.85481790222142));
#37261=CARTESIAN_POINT('Ctrl Pts',(-0.942854924895815,0.833437644084537,
-2.86426235362398));
#37262=CARTESIAN_POINT('Ctrl Pts',(-0.766217344968764,0.99004602720095,
-2.87789669534409));
#37263=CARTESIAN_POINT('Ctrl Pts',(-0.699515492219252,1.03860857285202,
-2.8826304404166));
#37264=CARTESIAN_POINT('Ctrl Pts',(-0.560312387087706,1.12016176874203,
-2.89184314967875));
#37265=CARTESIAN_POINT('Ctrl Pts',(-0.488709702220395,1.15327292383292,
-2.89625397165448));
#37266=CARTESIAN_POINT('Ctrl Pts',(-0.267376405963998,1.23032185121952,
-2.90959982294864));
#37267=CARTESIAN_POINT('Ctrl Pts',(-0.111255966138179,1.25355040542599,
-2.91861580960043));
#37268=CARTESIAN_POINT('Ctrl Pts',(0.207811766416421,1.2430813478547,-2.93702646035043));
#37269=CARTESIAN_POINT('Ctrl Pts',(0.365890893482803,1.20689167074436,-2.94595727210507));
#37270=CARTESIAN_POINT('Ctrl Pts',(0.66246547575248,1.07105294148954,-2.96463369266693));
#37271=CARTESIAN_POINT('Ctrl Pts',(0.795390494780788,0.976179148988214,
-2.97397058103383));
#37272=CARTESIAN_POINT('Ctrl Pts',(1.01906706662552,0.742059658066752,-2.99257707154));
#37273=CARTESIAN_POINT('Ctrl Pts',(1.10593290745587,0.604765495264961,-3.00150243713672));
#37274=CARTESIAN_POINT('Ctrl Pts',(1.22268749271409,0.301608920291551,-3.02018667806096));
#37275=CARTESIAN_POINT('Ctrl Pts',(1.25191342090965,0.139437458052851,-3.02960093321319));
#37276=CARTESIAN_POINT('Ctrl Pts',(1.24721623296255,-0.179028670469711,
-3.04780586454829));
#37277=CARTESIAN_POINT('Ctrl Pts',(1.21539049696997,-0.330706345188818,
-3.05637607013176));
#37278=CARTESIAN_POINT('Ctrl Pts',(1.09215941669519,-0.62701970757549,-3.07489627414963));
#37279=CARTESIAN_POINT('Ctrl Pts',(1.00108185129908,-0.765207162330717,
-3.08433677338233));
#37280=CARTESIAN_POINT('Ctrl Pts',(0.833365504294956,-0.934835618383368,
-3.09787786040257));
#37281=CARTESIAN_POINT('Ctrl Pts',(0.775086564049311,-0.983541309444154,
-3.1021282893586));
#37282=CARTESIAN_POINT('Ctrl Pts',(0.648015857718714,-1.07117841812588,
-3.11094391137086));
#37283=CARTESIAN_POINT('Ctrl Pts',(0.579365773160173,-1.10951676907334,
-3.11545488387097));
#37284=CARTESIAN_POINT('Ctrl Pts',(0.507823374560588,-1.14126439449584,
-3.11997532266811));
#37285=CARTESIAN_POINT('',(0.394326187104466,-0.886231714415119,-2.83167491439397));
#37286=CARTESIAN_POINT('Ctrl Pts',(0.394086384346302,-0.885697063989625,
-2.83165913284815));
#37287=CARTESIAN_POINT('Ctrl Pts',(0.298191870090869,-0.928570381426029,
-2.83941528578584));
#37288=CARTESIAN_POINT('Ctrl Pts',(0.178519107793232,-0.964221384880582,
-2.84846957656523));
#37289=CARTESIAN_POINT('Ctrl Pts',(-0.0910893742334462,-0.97348143994269,
-2.86840903499846));
#37290=CARTESIAN_POINT('Ctrl Pts',(-0.219578006005599,-0.952478120502755,
-2.87782973403179));
#37291=CARTESIAN_POINT('Ctrl Pts',(-0.459314331859824,-0.863779587384772,
-2.89670425862456));
#37292=CARTESIAN_POINT('Ctrl Pts',(-0.567630710127538,-0.796933539091381,
-2.90593876291026));
#37293=CARTESIAN_POINT('Ctrl Pts',(-0.752828485440917,-0.623184054868321,
-2.92469285313095));
#37294=CARTESIAN_POINT('Ctrl Pts',(-0.828023420909118,-0.519426122579518,
-2.93397030180843));
#37295=CARTESIAN_POINT('Ctrl Pts',(-0.942555212820417,-0.272657343323888,
-2.95407182645678));
#37296=CARTESIAN_POINT('Ctrl Pts',(-0.964576092397811,-0.146345569842905,
-2.96335452680482));
#37297=CARTESIAN_POINT('Ctrl Pts',(-0.973234758229753,0.085059333000677,
-2.98044711073806));
#37298=CARTESIAN_POINT('Ctrl Pts',(-0.954764421553846,0.209443759379039,
-2.98956074285187));
#37299=CARTESIAN_POINT('Ctrl Pts',(-0.863385541083941,0.467538462783729,
-3.00980188577291));
#37300=CARTESIAN_POINT('Ctrl Pts',(-0.787741201038076,0.574355926245684,
-3.01926109451035));
#37301=CARTESIAN_POINT('Ctrl Pts',(-0.636563258090323,0.740825101047964,
-3.03585527777922));
#37302=CARTESIAN_POINT('Ctrl Pts',(-0.538712695870475,0.815657266700878,
-3.04479456058827));
#37303=CARTESIAN_POINT('Ctrl Pts',(-0.314574481362839,0.926631232436039,
-3.06328843958487));
#37304=CARTESIAN_POINT('Ctrl Pts',(-0.187145566187865,0.959632056662996,
-3.07281755433396));
#37305=CARTESIAN_POINT('Ctrl Pts',(0.0437158535439579,0.973816785682934,
-3.08988664174321));
#37306=CARTESIAN_POINT('Ctrl Pts',(0.169857833048961,0.966145605389422,
-3.09903523853281));
#37307=CARTESIAN_POINT('Ctrl Pts',(0.428395654897726,0.879230744200456,
-3.11919869292516));
#37308=CARTESIAN_POINT('Ctrl Pts',(0.541693017629146,0.813745168936613,
-3.12866814077356));
#37309=CARTESIAN_POINT('Ctrl Pts',(0.734982717893037,0.645443410637293,
-3.14758833712456));
#37310=CARTESIAN_POINT('Ctrl Pts',(0.811636406380394,0.546422715832165,
-3.1566716811053));
#37311=CARTESIAN_POINT('Ctrl Pts',(0.924128601451255,0.318615613830126,
-3.17544146592106));
#37312=CARTESIAN_POINT('Ctrl Pts',(0.958033338094721,0.193919701721466,
-3.18479420359993));
#37313=CARTESIAN_POINT('Ctrl Pts',(0.97874917268754,-0.089285106719314,
-3.20576925505879));
#37314=CARTESIAN_POINT('Ctrl Pts',(0.950086443151077,-0.216174344769035,
-3.21517089557785));
#37315=CARTESIAN_POINT('Ctrl Pts',(0.880126890034671,-0.424386369963116,
-3.23138783895344));
#37316=CARTESIAN_POINT('Ctrl Pts',(0.81794788326764,-0.535142012129345,
-3.24058800419709));
#37317=CARTESIAN_POINT('Ctrl Pts',(0.641552013655281,-0.742759599885946,
-3.26072365759223));
#37318=CARTESIAN_POINT('Ctrl Pts',(0.534674148075254,-0.81568006401429,
-3.27008398461488));
#37319=CARTESIAN_POINT('Ctrl Pts',(0.330664337417023,-0.91916712047059,
-3.28696649642188));
#37320=CARTESIAN_POINT('Ctrl Pts',(0.211227470815213,-0.954389957357222,
-3.29599660516303));
#37321=CARTESIAN_POINT('Ctrl Pts',(-0.070456900897414,-0.98088312397359,
-3.31691602932236));
#37322=CARTESIAN_POINT('Ctrl Pts',(-0.203914130061255,-0.952161421978616,
-3.32675465971631));
#37323=CARTESIAN_POINT('Ctrl Pts',(-0.369580167595495,-0.899678213762173,
-3.33957853134598));
#37324=CARTESIAN_POINT('Ctrl Pts',(-0.490729761001413,-0.852001171582361,
-3.34896443828069));
#37325=CARTESIAN_POINT('Ctrl Pts',(-0.713516101842874,-0.669284725414497,
-3.37026839164066));
#37326=CARTESIAN_POINT('Ctrl Pts',(-0.796210772486546,-0.567271827168231,
-3.37977222452207));
#37327=CARTESIAN_POINT('Ctrl Pts',(-0.906615489405549,-0.359724464965979,
-3.39712344289772));
#37328=CARTESIAN_POINT('Ctrl Pts',(-0.950884825918705,-0.240943001075843,
-3.4063042462591));
#37329=CARTESIAN_POINT('Ctrl Pts',(-0.977297097691617,0.0296841041748129,
-3.42639876105417));
#37330=CARTESIAN_POINT('Ctrl Pts',(-0.964454925062395,0.159120292206572,
-3.43581129635004));
#37331=CARTESIAN_POINT('Ctrl Pts',(-0.891014447070679,0.404087567422178,
-3.45469622158211));
#37332=CARTESIAN_POINT('Ctrl Pts',(-0.830998255952601,0.516453374987384,
-3.46393822594497));
#37333=CARTESIAN_POINT('Ctrl Pts',(-0.669226084533204,0.712159990286062,
-3.48268933936367));
#37334=CARTESIAN_POINT('Ctrl Pts',(-0.570521723227356,0.793670410863379,
-3.49195784105761));
#37335=CARTESIAN_POINT('Ctrl Pts',(-0.331511437622619,0.923522973270032,
-3.51205699903807));
#37336=CARTESIAN_POINT('Ctrl Pts',(-0.20672456893489,0.953433421673878,
-3.52134676113068));
#37337=CARTESIAN_POINT('Ctrl Pts',(0.0234203099571636,0.976651850922853,
-3.5384202580365));
#37338=CARTESIAN_POINT('Ctrl Pts',(0.148589513594771,0.96611004897266,-3.54752453035876));
#37339=CARTESIAN_POINT('Ctrl Pts',(0.412125331987641,0.891213160371833,
-3.56777911550269));
#37340=CARTESIAN_POINT('Ctrl Pts',(0.523612092796821,0.822292732945892,
-3.57725023419229));
#37341=CARTESIAN_POINT('Ctrl Pts',(0.69897660882979,0.682239902879801,-3.5938116229893));
#37342=CARTESIAN_POINT('Ctrl Pts',(0.77978007351188,0.589452244916244,-3.60274106140891));
#37343=CARTESIAN_POINT('Ctrl Pts',(0.90059415624719,0.380054045915018,-3.62061717795275));
#37344=CARTESIAN_POINT('Ctrl Pts',(0.940480498058544,0.263658903783137,
-3.62954661637244));
#37345=CARTESIAN_POINT('Ctrl Pts',(0.973957141473118,0.0417426514745017,
-3.64610800516952));
#37346=CARTESIAN_POINT('Ctrl Pts',(0.97782361066481,-0.0892702241076332,
-3.65557912385921));
#37347=CARTESIAN_POINT('Ctrl Pts',(0.910762191275743,-0.354908017969242,
-3.67583370900311));
#37348=CARTESIAN_POINT('Ctrl Pts',(0.857240266408209,-0.468547195571491,
-3.68493798132528));
#37349=CARTESIAN_POINT('Ctrl Pts',(0.721949794241174,-0.65616981914845,
-3.70201147823101));
#37350=CARTESIAN_POINT('Ctrl Pts',(0.633598447246369,-0.749231288107553,
-3.71130124032356));
#37351=CARTESIAN_POINT('Ctrl Pts',(0.401554241019639,-0.891157645578987,
-3.73140039830393));
#37352=CARTESIAN_POINT('Ctrl Pts',(0.28158570257675,-0.93581242569692,-3.74066889999782));
#37353=CARTESIAN_POINT('Ctrl Pts',(0.031187933237524,-0.977910784659368,
-3.75942001341647));
#37354=CARTESIAN_POINT('Ctrl Pts',(-0.0961293116754024,-0.973628606025547,
-3.7686620177793));
#37355=CARTESIAN_POINT('Ctrl Pts',(-0.344962787881492,-0.914600046384491,
-3.7875469430114));
#37356=CARTESIAN_POINT('Ctrl Pts',(-0.463447383824335,-0.860933961244331,
-3.79695947830734));
#37357=CARTESIAN_POINT('Ctrl Pts',(-0.684518196277534,-0.702616766733451,
-3.81705399310246));
#37358=CARTESIAN_POINT('Ctrl Pts',(-0.765193847051316,-0.604840237385012,
-3.82623479646385));
#37359=CARTESIAN_POINT('Ctrl Pts',(-0.889615581919413,-0.405380113632151,
-3.84358601483951));
#37360=CARTESIAN_POINT('Ctrl Pts',(-0.936541938784186,-0.282730380681472,
-3.85308984772092));
#37361=CARTESIAN_POINT('Ctrl Pts',(-0.983218772209115,0.00159395276037214,
-3.87439380108085));
#37362=CARTESIAN_POINT('Ctrl Pts',(-0.963857842098933,0.13033974383224,
-3.88377970801553));
#37363=CARTESIAN_POINT('Ctrl Pts',(-0.926376886725791,0.30003034793623,
-3.89660357964515));
#37364=CARTESIAN_POINT('Ctrl Pts',(-0.884445642428363,0.429943930495119,
-3.90644221003906));
#37365=CARTESIAN_POINT('Ctrl Pts',(-0.720524154999497,0.660546877362438,
-3.92736163419847));
#37366=CARTESIAN_POINT('Ctrl Pts',(-0.630251429764562,0.746317783972123,
-3.9363917429397));
#37367=CARTESIAN_POINT('Ctrl Pts',(-0.43855071788084,0.871139299593482,
-3.95327425474676));
#37368=CARTESIAN_POINT('Ctrl Pts',(-0.321927863418365,0.927169488390545,
-3.96263458176947));
#37369=CARTESIAN_POINT('Ctrl Pts',(-0.0538991006256375,0.97596649524412,
-3.98277023516459));
#37370=CARTESIAN_POINT('Ctrl Pts',(0.0731066818806159,0.974362636104429,
-3.99197040040816));
#37371=CARTESIAN_POINT('Ctrl Pts',(0.288377749580642,0.930716858309803,
-4.00818734378377));
#37372=CARTESIAN_POINT('Ctrl Pts',(0.412575699626203,0.892021897374454,
-4.01758898430277));
#37373=CARTESIAN_POINT('Ctrl Pts',(0.647386542142373,0.732341035767552,
-4.03856403576163));
#37374=CARTESIAN_POINT('Ctrl Pts',(0.738370090523761,0.640577232514683,
-4.04791677344056));
#37375=CARTESIAN_POINT('Ctrl Pts',(0.879286517416555,0.429169734287984,
-4.0666865582564));
#37376=CARTESIAN_POINT('Ctrl Pts',(0.926645994771913,0.313247493699832,
-4.07576990223715));
#37377=CARTESIAN_POINT('Ctrl Pts',(0.975606909619787,0.0616740076335164,
-4.09469009858811));
#37378=CARTESIAN_POINT('Ctrl Pts',(0.975593497086552,-0.0691871890201205,
-4.10415954643651));
#37379=CARTESIAN_POINT('Ctrl Pts',(0.921437955672765,-0.336513161862337,
-4.12432300082888));
#37380=CARTESIAN_POINT('Ctrl Pts',(0.86494396051151,-0.449557730556663,
-4.13347159761848));
#37381=CARTESIAN_POINT('Ctrl Pts',(0.737115611443269,-0.642322132956231,
-4.15054068502775));
#37382=CARTESIAN_POINT('Ctrl Pts',(0.644766461351634,-0.736124144126927,
-4.16006979977683));
#37383=CARTESIAN_POINT('Ctrl Pts',(0.436509652621522,-0.874624187055258,
-4.17856367877346));
#37384=CARTESIAN_POINT('Ctrl Pts',(0.322750023297333,-0.921882332163206,
-4.18750296158255));
#37385=CARTESIAN_POINT('Ctrl Pts',(0.102966529943014,-0.969442532354416,
-4.20409714485148));
#37386=CARTESIAN_POINT('Ctrl Pts',(-0.0273693659811663,-0.981467128609304,
-4.21355635358899));
#37387=CARTESIAN_POINT('Ctrl Pts',(-0.296545998415822,-0.931398013650125,
-4.23379749651006));
#37388=CARTESIAN_POINT('Ctrl Pts',(-0.413474071476682,-0.885132858374174,
-4.24291112862382));
#37389=CARTESIAN_POINT('Ctrl Pts',(-0.609474827808149,-0.761816577731489,
-4.26000371255701));
#37390=CARTESIAN_POINT('Ctrl Pts',(-0.707805253771882,-0.679532250019484,
-4.26928641290498));
#37391=CARTESIAN_POINT('Ctrl Pts',(-0.864116564176997,-0.45686852146671,
-4.28938793755327));
#37392=CARTESIAN_POINT('Ctrl Pts',(-0.916307335662212,-0.339838139921263,
-4.29866538623074));
#37393=CARTESIAN_POINT('Ctrl Pts',(-0.974034598054681,-0.0925434525026932,
-4.31741947645142));
#37394=CARTESIAN_POINT('Ctrl Pts',(-0.977692016570374,0.0346864781869331,
-4.32665398073712));
#37395=CARTESIAN_POINT('Ctrl Pts',(-0.934490971108571,0.286628148782332,
-4.3455285053299));
#37396=CARTESIAN_POINT('Ctrl Pts',(-0.888364507480836,0.40837714169555,
-4.35494920436324));
#37397=CARTESIAN_POINT('Ctrl Pts',(-0.745406328022297,0.637150980780467,
-4.3748886666766));
#37398=CARTESIAN_POINT('Ctrl Pts',(-0.654644818685211,0.722911827601264,
-4.38394296032879));
#37399=CARTESIAN_POINT('Ctrl Pts',(-0.569531960289745,0.784472251448342,
-4.39169911510096));
#37400=CARTESIAN_POINT('',(0.5081523591131,-1.142051303545,-2.670016835446));
#37401=CARTESIAN_POINT('Ctrl Pts',(-0.5744373942835,0.7635955204679,-1.35880161274));
#37402=CARTESIAN_POINT('Ctrl Pts',(-0.3942519210863,0.8991453907025,-1.375701703932));
#37403=CARTESIAN_POINT('Ctrl Pts',(0.06522221406019,1.036583920368,-1.409501886316));
#37404=CARTESIAN_POINT('Ctrl Pts',(0.7237741231913,0.74512128044,-1.460202159892));
#37405=CARTESIAN_POINT('Ctrl Pts',(1.034330285883,0.09544979952193,-1.510902433468));
#37406=CARTESIAN_POINT('Ctrl Pts',(0.8478838926151,-0.6000535540617,-1.561602707044));
#37407=CARTESIAN_POINT('Ctrl Pts',(0.2539702938632,-1.007208621374,-1.61230298062));
#37408=CARTESIAN_POINT('Ctrl Pts',(-0.46198624017,-0.9303428349025,-1.663003254196));
#37409=CARTESIAN_POINT('Ctrl Pts',(-0.955934349857,-0.4063977219828,-1.713703527772));
#37410=CARTESIAN_POINT('Ctrl Pts',(-0.9905040632336,0.3128436609437,-1.764403801348));
#37411=CARTESIAN_POINT('Ctrl Pts',(-0.5490830845512,0.8817466980546,-1.815104074924));
#37412=CARTESIAN_POINT('Ctrl Pts',(0.1562020238423,1.026922783566,-1.8658043485));
#37413=CARTESIAN_POINT('Ctrl Pts',(0.7864236089275,0.6786069412635,-1.916504622076));
#37414=CARTESIAN_POINT('Ctrl Pts',(1.038726128586,0.004183771769307,-1.967204895652));
#37415=CARTESIAN_POINT('Ctrl Pts',(0.7918645782425,-0.6722499265432,-2.017905169228));
#37416=CARTESIAN_POINT('Ctrl Pts',(0.1644692813081,-1.025631185916,-2.068605442804));
#37417=CARTESIAN_POINT('Ctrl Pts',(-0.541962398324,-0.8861412036624,-2.11930571638));
#37418=CARTESIAN_POINT('Ctrl Pts',(-0.9879518411537,-0.3208124585826,-2.170005989956));
#37419=CARTESIAN_POINT('Ctrl Pts',(-0.9591770048575,0.3986840194666,-2.220706263532));
#37420=CARTESIAN_POINT('Ctrl Pts',(-0.4694657541443,0.9265912689544,-2.271406537108));
#37421=CARTESIAN_POINT('Ctrl Pts',(0.2458491758444,1.009221312076,-2.322106810684));
#37422=CARTESIAN_POINT('Ctrl Pts',(0.8430202836683,0.6068659452285,-2.37280708426));
#37423=CARTESIAN_POINT('Ctrl Pts',(1.035074561878,-0.08712132208854,-2.423507357836));
#37424=CARTESIAN_POINT('Ctrl Pts',(0.7297195473129,-0.7392420834405,-2.474207631412));
#37425=CARTESIAN_POINT('Ctrl Pts',(0.07369482757466,-1.036117052103,-2.524907904988));
#37426=CARTESIAN_POINT('Ctrl Pts',(-0.6177442188356,-0.8350817538242,-2.575608178564));
#37427=CARTESIAN_POINT('Ctrl Pts',(-1.01232385091,-0.2327445177605,-2.62630845214));
#37428=CARTESIAN_POINT('Ctrl Pts',(-0.9204268188452,0.4814390384163,-2.677008725716));
#37429=CARTESIAN_POINT('Ctrl Pts',(-0.3862161132211,0.9642651248607,-2.727708999292));
#37430=CARTESIAN_POINT('Ctrl Pts',(0.3335967262064,0.9837096051999,-2.778409272868));
#37431=CARTESIAN_POINT('Ctrl Pts',(0.8930818486504,0.5304287097581,-2.829109546444));
#37432=CARTESIAN_POINT('Ctrl Pts',(1.023454253376,-0.1777529049358,-2.87980982002));
#37433=CARTESIAN_POINT('Ctrl Pts',(0.6617724011872,-0.8005107433383,-2.930510093596));
#37434=CARTESIAN_POINT('Ctrl Pts',(0.209209682755,-0.9592331935163,-2.96431027598));
#37435=CARTESIAN_POINT('Ctrl Pts',(-0.01623630497839,-0.9554019160702,-2.981210367172));
#37436=CARTESIAN_POINT('Ctrl Pts',(-0.6363414402896,0.8458841261532,-1.418253345368));
#37437=CARTESIAN_POINT('Ctrl Pts',(-0.4367383422416,0.9960414810095,-1.43515343656));
#37438=CARTESIAN_POINT('Ctrl Pts',(0.07225086327415,1.148291026024,-1.468953618944));
#37439=CARTESIAN_POINT('Ctrl Pts',(0.8017713898489,0.825419016074,-1.51965389252));
#37440=CARTESIAN_POINT('Ctrl Pts',(1.145794529402,0.10573591397,-1.570354166096));
#37441=CARTESIAN_POINT('Ctrl Pts',(0.9392558054095,-0.664718116617,-1.621054439672));
#37442=CARTESIAN_POINT('Ctrl Pts',(0.2813393142507,-1.11575010815,-1.671754713248));
#37443=CARTESIAN_POINT('Ctrl Pts',(-0.5117720266635,-1.030600906933,-1.722454986824));
#37444=CARTESIAN_POINT('Ctrl Pts',(-1.058950282596,-0.4501930311474,-1.7731552604));
#37445=CARTESIAN_POINT('Ctrl Pts',(-1.097245389111,0.3465571492585,-1.823855533976));
#37446=CARTESIAN_POINT('Ctrl Pts',(-0.6082548321872,0.9767678242997,-1.874555807552));
#37447=CARTESIAN_POINT('Ctrl Pts',(0.1730350806147,1.137588760174,-1.925256081128));
#37448=CARTESIAN_POINT('Ctrl Pts',(0.8711722756261,0.7517367822698,-1.975956354704));
#37449=CARTESIAN_POINT('Ctrl Pts',(1.150664088565,0.004634634478914,-2.02665662828));
#37450=CARTESIAN_POINT('Ctrl Pts',(0.877199589107,-0.7446947060692,-2.077356901856));
#37451=CARTESIAN_POINT('Ctrl Pts',(0.1821932562059,-1.136157973952,-2.128057175432));
#37452=CARTESIAN_POINT('Ctrl Pts',(-0.6003667876853,-0.9816359022759,-2.178757449008));
#37453=CARTESIAN_POINT('Ctrl Pts',(-1.094418127707,-0.3553847016034,-2.229457722584));
#37454=CARTESIAN_POINT('Ctrl Pts',(-1.062542381185,0.4416480641625,-2.28015799616));
#37455=CARTESIAN_POINT('Ctrl Pts',(-0.5200575678599,1.026445054786,-2.330858269736));
#37456=CARTESIAN_POINT('Ctrl Pts',(0.2723430267731,1.117979695766,-2.381558543312));
#37457=CARTESIAN_POINT('Ctrl Pts',(0.933868071336,0.6722646427485,-2.432258816888));
#37458=CARTESIAN_POINT('Ctrl Pts',(1.146619012041,-0.09650992106268,-2.482959090464));
#37459=CARTESIAN_POINT('Ctrl Pts',(0.8083575205332,-0.8189062494547,-2.53365936404));
#37460=CARTESIAN_POINT('Ctrl Pts',(0.08163652503724,-1.147773845863,-2.584359637616));
#37461=CARTESIAN_POINT('Ctrl Pts',(-0.6843152097275,-0.9250740485843,-2.635059911192));
#37462=CARTESIAN_POINT('Ctrl Pts',(-1.121416578618,-0.2578261497687,-2.685760184768));
#37463=CARTESIAN_POINT('Ctrl Pts',(-1.019616294854,0.5333211489471,-2.736460458344));
#37464=CARTESIAN_POINT('Ctrl Pts',(-0.4278365583367,1.068178820671,-2.78716073192));
#37465=CARTESIAN_POINT('Ctrl Pts',(0.3695466613813,1.089718728671,-2.837861005496));
#37466=CARTESIAN_POINT('Ctrl Pts',(0.9893245034571,0.5875901751825,-2.888561279072));
#37467=CARTESIAN_POINT('Ctrl Pts',(1.133746445034,-0.1969083849139,-2.939261552648));
#37468=CARTESIAN_POINT('Ctrl Pts',(0.7330880738372,-0.8867775051772,-2.989961826224));
#37469=CARTESIAN_POINT('Ctrl Pts',(0.2317550914541,-1.062604624995,-3.023762008608));
#37470=CARTESIAN_POINT('Ctrl Pts',(-0.01798600473741,-1.058360471267,-3.0406620998));
#37471=CARTESIAN_POINT('Ctrl Pts',(-0.6982454862957,0.9281727318386,-1.477705077996));
#37472=CARTESIAN_POINT('Ctrl Pts',(-0.479224763397,1.092937571317,-1.494605169188));
#37473=CARTESIAN_POINT('Ctrl Pts',(0.07927951248811,1.259998131679,-1.528405351572));
#37474=CARTESIAN_POINT('Ctrl Pts',(0.8797686565066,0.905716751708,-1.579105625148));
#37475=CARTESIAN_POINT('Ctrl Pts',(1.257258772921,0.1160220284182,-1.629805898724));
#37476=CARTESIAN_POINT('Ctrl Pts',(1.030627718204,-0.7293826791723,-1.6805061723));
#37477=CARTESIAN_POINT('Ctrl Pts',(0.3087083346382,-1.224291594926,-1.731206445876));
#37478=CARTESIAN_POINT('Ctrl Pts',(-0.561557813157,-1.130858978964,-1.781906719452));
#37479=CARTESIAN_POINT('Ctrl Pts',(-1.161966215335,-0.4939883403121,-1.832606993028));
#37480=CARTESIAN_POINT('Ctrl Pts',(-1.203986714989,0.3802706375734,-1.883307266604));
#37481=CARTESIAN_POINT('Ctrl Pts',(-0.6674265798232,1.071788950545,-1.93400754018));
#37482=CARTESIAN_POINT('Ctrl Pts',(0.1898681373872,1.248254736783,-1.984707813756));
#37483=CARTESIAN_POINT('Ctrl Pts',(0.9559209423246,0.8248666232761,-2.035408087332));
#37484=CARTESIAN_POINT('Ctrl Pts',(1.262602048544,0.005085497188518,-2.086108360908));
#37485=CARTESIAN_POINT('Ctrl Pts',(0.9625345999714,-0.8171394855951,-2.136808634484));
#37486=CARTESIAN_POINT('Ctrl Pts',(0.1999172311038,-1.246684761989,-2.18750890806));
#37487=CARTESIAN_POINT('Ctrl Pts',(-0.6587711770466,-1.077130600889,-2.238209181636));
#37488=CARTESIAN_POINT('Ctrl Pts',(-1.20088441426,-0.3899569446243,-2.288909455212));
#37489=CARTESIAN_POINT('Ctrl Pts',(-1.165907757512,0.4846121088583,-2.339609728788));
#37490=CARTESIAN_POINT('Ctrl Pts',(-0.5706493815754,1.126298840617,-2.390310002364));
#37491=CARTESIAN_POINT('Ctrl Pts',(0.2988368777019,1.226738079456,-2.44101027594));
#37492=CARTESIAN_POINT('Ctrl Pts',(1.024715859004,0.7376633402686,-2.491710549516));
#37493=CARTESIAN_POINT('Ctrl Pts',(1.258163462203,-0.1058985200368,-2.542410823092));
#37494=CARTESIAN_POINT('Ctrl Pts',(0.8869954937535,-0.8985704154689,-2.593111096668));
#37495=CARTESIAN_POINT('Ctrl Pts',(0.08957822249982,-1.259430639622,-2.643811370244));
#37496=CARTESIAN_POINT('Ctrl Pts',(-0.7508862006194,-1.015066343344,-2.69451164382));
#37497=CARTESIAN_POINT('Ctrl Pts',(-1.230509306326,-0.2829077817768,-2.745211917396));
#37498=CARTESIAN_POINT('Ctrl Pts',(-1.118805770864,0.585203259478,-2.795912190972));
#37499=CARTESIAN_POINT('Ctrl Pts',(-0.4694570034523,1.172092516481,-2.846612464548));
#37500=CARTESIAN_POINT('Ctrl Pts',(0.4054965965563,1.195727852142,-2.897312738124));
#37501=CARTESIAN_POINT('Ctrl Pts',(1.085567158264,0.6447516406069,-2.9480130117));
#37502=CARTESIAN_POINT('Ctrl Pts',(1.244038636693,-0.216063864892,-2.998713285276));
#37503=CARTESIAN_POINT('Ctrl Pts',(0.8044037464872,-0.973044267016,-3.049413558852));
#37504=CARTESIAN_POINT('Ctrl Pts',(0.2543005001532,-1.165976056474,-3.083213741236));
#37505=CARTESIAN_POINT('Ctrl Pts',(-0.01973570449643,-1.161319026465,-3.100113832428));
#37506=CARTESIAN_POINT('Ctrl Pts',(-0.7601495323018,1.010461337524,-1.537156810625));
#37507=CARTESIAN_POINT('Ctrl Pts',(-0.5217111845523,1.189833661624,-1.554056901817));
#37508=CARTESIAN_POINT('Ctrl Pts',(0.08630816170208,1.371705237335,-1.587857084201));
#37509=CARTESIAN_POINT('Ctrl Pts',(0.9577659231642,0.986014487342,-1.638557357777));
#37510=CARTESIAN_POINT('Ctrl Pts',(1.36872301644,0.1263081428663,-1.689257631353));
#37511=CARTESIAN_POINT('Ctrl Pts',(1.121999630998,-0.7940472417276,-1.739957904929));
#37512=CARTESIAN_POINT('Ctrl Pts',(0.3360773550257,-1.332833081702,-1.790658178505));
#37513=CARTESIAN_POINT('Ctrl Pts',(-0.6113435996505,-1.231117050995,-1.841358452081));
#37514=CARTESIAN_POINT('Ctrl Pts',(-1.264982148074,-0.5377836494768,-1.892058725657));
#37515=CARTESIAN_POINT('Ctrl Pts',(-1.310728040867,0.4139841258882,-1.942758999233));
#37516=CARTESIAN_POINT('Ctrl Pts',(-0.7265983274592,1.16681007679,-1.993459272809));
#37517=CARTESIAN_POINT('Ctrl Pts',(0.2067011941596,1.358920713391,-2.044159546385));
#37518=CARTESIAN_POINT('Ctrl Pts',(1.040669609023,0.8979964642824,-2.094859819961));
#37519=CARTESIAN_POINT('Ctrl Pts',(1.374540008523,0.005536359898125,-2.145560093537));
#37520=CARTESIAN_POINT('Ctrl Pts',(1.047869610836,-0.8895842651211,-2.196260367113));
#37521=CARTESIAN_POINT('Ctrl Pts',(0.2176412060017,-1.357211550025,-2.246960640689));
#37522=CARTESIAN_POINT('Ctrl Pts',(-0.7171755664079,-1.172625299503,-2.297660914265));
#37523=CARTESIAN_POINT('Ctrl Pts',(-1.307350700813,-0.4245291876451,-2.348361187841));
#37524=CARTESIAN_POINT('Ctrl Pts',(-1.26927313384,0.5275761535541,-2.399061461417));
#37525=CARTESIAN_POINT('Ctrl Pts',(-0.621241195291,1.226152626448,-2.449761734993));
#37526=CARTESIAN_POINT('Ctrl Pts',(0.3253307286306,1.335496463145,-2.500462008569));
#37527=CARTESIAN_POINT('Ctrl Pts',(1.115563646671,0.8030620377886,-2.551162282145));
#37528=CARTESIAN_POINT('Ctrl Pts',(1.369707912366,-0.115287119011,-2.601862555721));
#37529=CARTESIAN_POINT('Ctrl Pts',(0.9656334669738,-0.978234581483,-2.652562829297));
#37530=CARTESIAN_POINT('Ctrl Pts',(0.0975199199624,-1.371087433381,-2.703263102873));
#37531=CARTESIAN_POINT('Ctrl Pts',(-0.8174571915112,-1.105058638105,-2.753963376449));
#37532=CARTESIAN_POINT('Ctrl Pts',(-1.339602034034,-0.3079894137849,-2.804663650025));
#37533=CARTESIAN_POINT('Ctrl Pts',(-1.217995246873,0.6370853700088,-2.855363923601));
#37534=CARTESIAN_POINT('Ctrl Pts',(-0.5110774485679,1.276006212291,-2.906064197177));
#37535=CARTESIAN_POINT('Ctrl Pts',(0.4414465317312,1.301736975613,-2.956764470753));
#37536=CARTESIAN_POINT('Ctrl Pts',(1.18180981307,0.7019131060313,-3.007464744329));
#37537=CARTESIAN_POINT('Ctrl Pts',(1.354330828351,-0.23521934487,-3.058165017905));
#37538=CARTESIAN_POINT('Ctrl Pts',(0.8757194191373,-1.059311028855,-3.108865291481));
#37539=CARTESIAN_POINT('Ctrl Pts',(0.2768459088523,-1.269347487952,-3.142665473865));
#37540=CARTESIAN_POINT('Ctrl Pts',(-0.02148540425545,-1.264277581662,-3.159565565057));
#37541=CARTESIAN_POINT('',(-0.259610714546449,1.22207863880594,-1.55963283939182));
#37542=CARTESIAN_POINT('Ctrl Pts',(0.507800078725617,-1.14130485853319,
-2.67007418463596));
#37543=CARTESIAN_POINT('Ctrl Pts',(0.612233666406878,-1.0949369024171,-2.66359308772046));
#37544=CARTESIAN_POINT('Ctrl Pts',(0.730114711952954,-1.02596491093318,
-2.65590451342733));
#37545=CARTESIAN_POINT('Ctrl Pts',(0.939047723037593,-0.835150961272447,
-2.6393783299617));
#37546=CARTESIAN_POINT('Ctrl Pts',(1.02060011568731,-0.731926231542939,
-2.63195399377308));
#37547=CARTESIAN_POINT('Ctrl Pts',(1.15133052288156,-0.502486024562013,
-2.61698799059436));
#37548=CARTESIAN_POINT('Ctrl Pts',(1.1994984257216,-0.375115822630611,-2.60939271858708));
#37549=CARTESIAN_POINT('Ctrl Pts',(1.24006231487454,-0.172945597679168,
-2.59745051292342));
#37550=CARTESIAN_POINT('Ctrl Pts',(1.24785745820879,-0.101838259601154,
-2.59326743352897));
#37551=CARTESIAN_POINT('Ctrl Pts',(1.25117970484064,0.0529687419467126,
-2.58433960981054));
#37552=CARTESIAN_POINT('Ctrl Pts',(1.24457703692924,0.136181129120054,-2.57961312073553));
#37553=CARTESIAN_POINT('Ctrl Pts',(1.20567920166832,0.354280324729834,-2.56704836928307));
#37554=CARTESIAN_POINT('Ctrl Pts',(1.15913703077502,0.48681205395866,-2.55921950127501));
#37555=CARTESIAN_POINT('Ctrl Pts',(1.05981281816954,0.666090081600009,-2.54734749584298));
#37556=CARTESIAN_POINT('Ctrl Pts',(1.02309201000238,0.721182755833519,-2.54347119827756));
#37557=CARTESIAN_POINT('Ctrl Pts',(0.881914044721003,0.899560322331259,
-2.53032283606007));
#37558=CARTESIAN_POINT('Ctrl Pts',(0.757112161818906,1.006236439173,-2.52126598676422));
#37559=CARTESIAN_POINT('Ctrl Pts',(0.485273028040564,1.161587970364,-2.50344835191949));
#37560=CARTESIAN_POINT('Ctrl Pts',(0.34622708590613,1.21028400666312,-2.49492562637545));
#37561=CARTESIAN_POINT('Ctrl Pts',(0.1180758092039,1.24663611655136,-2.48163302861913));
#37562=CARTESIAN_POINT('Ctrl Pts',(0.0347233483400104,1.25146309140558,
-2.47691284801568));
#37563=CARTESIAN_POINT('Ctrl Pts',(-0.183382111018931,1.242869499445,-2.46454018040272));
#37564=CARTESIAN_POINT('Ctrl Pts',(-0.317775396484216,1.21608479852621,
-2.45688827247895));
#37565=CARTESIAN_POINT('Ctrl Pts',(-0.513164682464846,1.1421950940086,-2.44477199616997));
#37566=CARTESIAN_POINT('Ctrl Pts',(-0.579179773460147,1.11007605609173,
-2.44048168561375));
#37567=CARTESIAN_POINT('Ctrl Pts',(-0.713385303800749,1.02917629167349,
-2.431457345549));
#37568=CARTESIAN_POINT('Ctrl Pts',(-0.78021602350588,0.979122799501168,
-2.42673408745597));
#37569=CARTESIAN_POINT('Ctrl Pts',(-0.942214698504906,0.831173369487071,
-2.4142961651556));
#37570=CARTESIAN_POINT('Ctrl Pts',(-1.02825443966183,0.723026175962959,
-2.40658569983318));
#37571=CARTESIAN_POINT('Ctrl Pts',(-1.12831490924974,0.54250411551147,-2.39462199127633));
#37572=CARTESIAN_POINT('Ctrl Pts',(-1.15674670073225,0.478748838097753,
-2.39053815767876));
#37573=CARTESIAN_POINT('Ctrl Pts',(-1.20692115391492,0.334074387634818,
-2.38170467512774));
#37574=CARTESIAN_POINT('Ctrl Pts',(-1.22620888847941,0.252843748251602,
-2.37697631382472));
#37575=CARTESIAN_POINT('Ctrl Pts',(-1.2561914452077,0.0334025692953118,
-2.36441535390944));
#37576=CARTESIAN_POINT('Ctrl Pts',(-1.25263171750077,-0.106940783976178,
-2.35659413774588));
#37577=CARTESIAN_POINT('Ctrl Pts',(-1.21339160002161,-0.307346916463829,
-2.34477087009704));
#37578=CARTESIAN_POINT('Ctrl Pts',(-1.19562718031006,-0.370440174551519,
-2.34093320722807));
#37579=CARTESIAN_POINT('Ctrl Pts',(-1.11669511647946,-0.583141614803438,
-2.3278132653876));
#37580=CARTESIAN_POINT('Ctrl Pts',(-1.03089836416202,-0.723181862464307,
-2.31875130601161));
#37581=CARTESIAN_POINT('Ctrl Pts',(-0.814183597922892,-0.961623796844712,
-2.30041965778142));
#37582=CARTESIAN_POINT('Ctrl Pts',(-0.688622940074993,-1.05517691514589,
-2.29136876480927));
#37583=CARTESIAN_POINT('Ctrl Pts',(-0.402020857708303,-1.19353931793331,
-2.27309719359508));
#37584=CARTESIAN_POINT('Ctrl Pts',(-0.243808191860089,-1.23545544282677,
-2.26408213986346));
#37585=CARTESIAN_POINT('Ctrl Pts',(0.0812534277319099,-1.25821680962395,
-2.24545715027443));
#37586=CARTESIAN_POINT('Ctrl Pts',(0.244148088549536,-1.2367630646173,-2.23594808814865));
#37587=CARTESIAN_POINT('Ctrl Pts',(0.547496572649703,-1.13330715703507,
-2.21767661682907));
#37588=CARTESIAN_POINT('Ctrl Pts',(0.685768765362047,-1.05573529789564,
-2.20892469455316));
#37589=CARTESIAN_POINT('Ctrl Pts',(0.932890934550272,-0.848759548429491,
-2.19037969795629));
#37590=CARTESIAN_POINT('Ctrl Pts',(1.03356532261343,-0.721010795095412,
-2.18102416631749));
#37591=CARTESIAN_POINT('Ctrl Pts',(1.17487291216457,-0.447522694588082,
-2.16354273775075));
#37592=CARTESIAN_POINT('Ctrl Pts',(1.21933694334434,-0.308252026913084,
-2.15542543471449));
#37593=CARTESIAN_POINT('Ctrl Pts',(1.24684374138559,-0.1063117898711,-2.14365527952404));
#37594=CARTESIAN_POINT('Ctrl Pts',(1.25054027644431,-0.046790781155218,
-2.14016870831578));
#37595=CARTESIAN_POINT('Ctrl Pts',(1.24885165159501,0.0949819512083569,
-2.13193169800581));
#37596=CARTESIAN_POINT('Ctrl Pts',(1.23957690789249,0.17684746522871,-2.12723897694521));
#37597=CARTESIAN_POINT('Ctrl Pts',(1.18899122454946,0.414872034867468,-2.11340296941449));
#37598=CARTESIAN_POINT('Ctrl Pts',(1.1253086931289,0.566545863998217,-2.10432200684995));
#37599=CARTESIAN_POINT('Ctrl Pts',(0.99772842630465,0.755973242928381,-2.09109665472807));
#37600=CARTESIAN_POINT('Ctrl Pts',(0.955975765769682,0.8080929264264,-2.08718705160299));
#37601=CARTESIAN_POINT('Ctrl Pts',(0.816508252869463,0.955501643623805,
-2.07545874339807));
#37602=CARTESIAN_POINT('Ctrl Pts',(0.706723827562254,1.03873387903179,-2.06778322435594));
#37603=CARTESIAN_POINT('Ctrl Pts',(0.514318875156416,1.14144932299447,-2.05541075057229));
#37604=CARTESIAN_POINT('Ctrl Pts',(0.438025563379678,1.17316462797112,-2.05072820289678));
#37605=CARTESIAN_POINT('Ctrl Pts',(0.291082021764648,1.21768121802146,-2.0418654362662));
#37606=CARTESIAN_POINT('Ctrl Pts',(0.221560531534333,1.23226747309818,-2.037707766503));
#37607=CARTESIAN_POINT('Ctrl Pts',(0.0206049999289771,1.25624693474514,
-2.02598976383744));
#37608=CARTESIAN_POINT('Ctrl Pts',(-0.11199415053374,1.25087818655238,-2.01857533351991));
#37609=CARTESIAN_POINT('Ctrl Pts',(-0.322236465734706,1.20977941365008,
-2.00643183442636));
#37610=CARTESIAN_POINT('Ctrl Pts',(-0.402346692969266,1.18583658575053,
-2.00170402448945));
#37611=CARTESIAN_POINT('Ctrl Pts',(-0.617543203539604,1.09717922754569,
-1.98830826792993));
#37612=CARTESIAN_POINT('Ctrl Pts',(-0.742072545436565,1.01688835433628,
-1.97974310797231));
#37613=CARTESIAN_POINT('Ctrl Pts',(-0.970528733933381,0.802411539894461,
-1.961916047245));
#37614=CARTESIAN_POINT('Ctrl Pts',(-1.06721562926637,0.669459708521441,
-1.9528453631822));
#37615=CARTESIAN_POINT('Ctrl Pts',(-1.16387689970394,0.461009366896075,
-1.93955597171686));
#37616=CARTESIAN_POINT('Ctrl Pts',(-1.18727315637734,0.396889281624173,
-1.93555952718361));
#37617=CARTESIAN_POINT('Ctrl Pts',(-1.24039670893314,0.201558749017812,
-1.92385192259047));
#37618=CARTESIAN_POINT('Ctrl Pts',(-1.25438695473961,0.0666101745329706,
-1.91628466662226));
#37619=CARTESIAN_POINT('Ctrl Pts',(-1.24301618552763,-0.14921257142496,
-1.90402880525015));
#37620=CARTESIAN_POINT('Ctrl Pts',(-1.2307474601993,-0.230947903243687,
-1.89934903401867));
#37621=CARTESIAN_POINT('Ctrl Pts',(-1.19244304551431,-0.381867692531711,
-1.89037302683353));
#37622=CARTESIAN_POINT('Ctrl Pts',(-1.16815111772457,-0.450924156209753,
-1.88609102206247));
#37623=CARTESIAN_POINT('Ctrl Pts',(-1.08371526213591,-0.635447518825377,
-1.87433352012401));
#37624=CARTESIAN_POINT('Ctrl Pts',(-1.01118775305882,-0.744554530895352,
-1.86700630443897));
#37625=CARTESIAN_POINT('Ctrl Pts',(-0.868260159324179,-0.901923869417574,
-1.85495740437297));
#37626=CARTESIAN_POINT('Ctrl Pts',(-0.806301169348746,-0.958058661436189,
-1.85023319411109));
#37627=CARTESIAN_POINT('Ctrl Pts',(-0.615864140590997,-1.09866090397637,
-1.83662343191714));
#37628=CARTESIAN_POINT('Ctrl Pts',(-0.478259891318438,-1.16521149345142,
-1.82779005534706));
#37629=CARTESIAN_POINT('Ctrl Pts',(-0.170195428785501,-1.24773053246873,
-1.80964900900546));
#37630=CARTESIAN_POINT('Ctrl Pts',(-0.00621787061589819,-1.25981453753794,
-1.80057552254435));
#37631=CARTESIAN_POINT('Ctrl Pts',(0.22148838945788,-1.23208442147924,-1.78730395750846));
#37632=CARTESIAN_POINT('Ctrl Pts',(0.287913517277362,-1.21826906905728,
-1.78333149002799));
#37633=CARTESIAN_POINT('Ctrl Pts',(0.48206990334696,-1.16057766045874,-1.77161922627142));
#37634=CARTESIAN_POINT('Ctrl Pts',(0.604642908876124,-1.10111918041112,
-1.76402300138723));
#37635=CARTESIAN_POINT('Ctrl Pts',(0.782442334550935,-0.977321574209538,
-1.75173597566535));
#37636=CARTESIAN_POINT('Ctrl Pts',(0.845406612756201,-0.923792114009704,
-1.74705547216814));
#37637=CARTESIAN_POINT('Ctrl Pts',(0.953023639005534,-0.812046846764356,
-1.73810889089031));
#37638=CARTESIAN_POINT('Ctrl Pts',(0.998555941030456,-0.755451629151792,
-1.73385923094735));
#37639=CARTESIAN_POINT('Ctrl Pts',(1.11085797729936,-0.586757033603323,
-1.72211958756504));
#37640=CARTESIAN_POINT('Ctrl Pts',(1.16554656062255,-0.467362481813021,
-1.71477694616158));
#37641=CARTESIAN_POINT('Ctrl Pts',(1.22407329621253,-0.262674922530386,
-1.70271079771865));
#37642=CARTESIAN_POINT('Ctrl Pts',(1.23913722339119,-0.180431870011504,
-1.6979856595597));
#37643=CARTESIAN_POINT('Ctrl Pts',(1.25815025227789,0.0538952546014994,
-1.68446543178557));
#37644=CARTESIAN_POINT('Ctrl Pts',(1.2426521532669,0.204271826373771,-1.67572541607777));
#37645=CARTESIAN_POINT('Ctrl Pts',(1.15216029633937,0.50829118316365,-1.65767678627267));
#37646=CARTESIAN_POINT('Ctrl Pts',(1.07656356464772,0.654366821513739,-1.64859980495065));
#37647=CARTESIAN_POINT('Ctrl Pts',(0.932841222330786,0.834919960138557,
-1.63525471667252));
#37648=CARTESIAN_POINT('Ctrl Pts',(0.885304617597667,0.885154473762003,
-1.63120703593855));
#37649=CARTESIAN_POINT('Ctrl Pts',(0.733892730794094,1.0199957546792,-1.61949235591571));
#37650=CARTESIAN_POINT('Ctrl Pts',(0.619904967924308,1.09243893007311,-1.61196568392511));
#37651=CARTESIAN_POINT('Ctrl Pts',(0.38102479404947,1.19652686604501,-1.59719153192072));
#37652=CARTESIAN_POINT('Ctrl Pts',(0.256450708106922,1.23003839998894,-1.58988830890701));
#37653=CARTESIAN_POINT('Ctrl Pts',(-0.0010614922244034,1.25675580911652,
-1.57476647375581));
#37654=CARTESIAN_POINT('Ctrl Pts',(-0.132557389488584,1.24899611401415,
-1.5673185533228));
#37655=CARTESIAN_POINT('Ctrl Pts',(-0.259591956716904,1.22190413578271,
-1.55995109671497));
#37656=CARTESIAN_POINT('',(-0.201562741974311,0.948826487356528,-1.3983503624951));
#37657=CARTESIAN_POINT('',(-0.2015628224599,0.948826869667,-1.39835034235));
#37658=CARTESIAN_POINT('Ctrl Pts',(-0.201438444627362,0.948254145075348,
-1.39833463125939));
#37659=CARTESIAN_POINT('Ctrl Pts',(-0.0987242220368489,0.970265808362698,
-1.40609108145075));
#37660=CARTESIAN_POINT('Ctrl Pts',(0.0257428725608549,0.980269505514474,
-1.4151452502064));
#37661=CARTESIAN_POINT('Ctrl Pts',(0.291387332434439,0.933304243270978,
-1.43508446652971));
#37662=CARTESIAN_POINT('Ctrl Pts',(0.412706897305461,0.88605986686801,-1.44450516556305));
#37663=CARTESIAN_POINT('Ctrl Pts',(0.628779001349331,0.749481019437183,
-1.46337969015587));
#37664=CARTESIAN_POINT('Ctrl Pts',(0.720840663164952,0.66158629606172,-1.47261419444165));
#37665=CARTESIAN_POINT('Ctrl Pts',(0.865891373452379,0.453145919229779,
-1.49136828466245));
#37666=CARTESIAN_POINT('Ctrl Pts',(0.917884397731051,0.336027550648196,
-1.50064573334002));
#37667=CARTESIAN_POINT('Ctrl Pts',(0.978638449230794,0.0708459015851718,
-1.52074725798837));
#37668=CARTESIAN_POINT('Ctrl Pts',(0.973931484966905,-0.0572846090069996,
-1.53002995833632));
#37669=CARTESIAN_POINT('Ctrl Pts',(0.934315968934625,-0.285437655104305,
-1.54712254226946));
#37670=CARTESIAN_POINT('Ctrl Pts',(0.890402125861598,-0.403268946572186,
-1.5562361743832));
#37671=CARTESIAN_POINT('Ctrl Pts',(0.747386626902548,-0.636741734663479,
-1.57647731730412));
#37672=CARTESIAN_POINT('Ctrl Pts',(0.651197130204397,-0.725508943735299,
-1.58593652604146));
#37673=CARTESIAN_POINT('Ctrl Pts',(0.46872734556964,-0.856930153167852,
-1.60253070931023));
#37674=CARTESIAN_POINT('Ctrl Pts',(0.357462783542698,-0.90979585830865,
-1.61146999211917));
#37675=CARTESIAN_POINT('Ctrl Pts',(0.1151570245764,-0.971772300974352,-1.62996387111578));
#37676=CARTESIAN_POINT('Ctrl Pts',(-0.016347839305272,-0.977573473079552,
-1.639492985865));
#37677=CARTESIAN_POINT('Ctrl Pts',(-0.245117563251694,-0.943476331507241,
-1.65656207327439));
#37678=CARTESIAN_POINT('Ctrl Pts',(-0.366912073350302,-0.90976070737921,
-1.66571067006408));
#37679=CARTESIAN_POINT('Ctrl Pts',(-0.601745916092765,-0.771019708663967,
-1.68587412445648));
#37680=CARTESIAN_POINT('Ctrl Pts',(-0.698962539434392,-0.683420729699717,
-1.69534357230481));
#37681=CARTESIAN_POINT('Ctrl Pts',(-0.853060563983244,-0.478627690499663,
-1.71426376865579));
#37682=CARTESIAN_POINT('Ctrl Pts',(-0.907464882095698,-0.365840031027879,
-1.72334711263655));
#37683=CARTESIAN_POINT('Ctrl Pts',(-0.970164031430926,-0.119629985848659,
-1.74211689745239));
#37684=CARTESIAN_POINT('Ctrl Pts',(-0.977417294464398,0.00938936091317684,
-1.75146963513136));
#37685=CARTESIAN_POINT('Ctrl Pts',(-0.938831912985727,0.290717066024187,
-1.77244468659029));
#37686=CARTESIAN_POINT('Ctrl Pts',(-0.884427664631833,0.408880548362764,
-1.78184632710929));
#37687=CARTESIAN_POINT('Ctrl Pts',(-0.772729409729827,0.598010361875881,
-1.79806327048482));
#37688=CARTESIAN_POINT('Ctrl Pts',(-0.688892984793707,0.693427839352924,
-1.80726343572838));
#37689=CARTESIAN_POINT('Ctrl Pts',(-0.473205224209429,0.859859072888414,
-1.82739908912347));
#37690=CARTESIAN_POINT('Ctrl Pts',(-0.353507651838664,0.908978961000493,
-1.83675941614616));
#37691=CARTESIAN_POINT('Ctrl Pts',(-0.132446689760668,0.967814534797147,
-1.85364192795321));
#37692=CARTESIAN_POINT('Ctrl Pts',(-0.00829769730837255,0.977449939050658,
-1.86267203669443));
#37693=CARTESIAN_POINT('Ctrl Pts',(0.272743269789277,0.944831723940324,
-1.88359146085372));
#37694=CARTESIAN_POINT('Ctrl Pts',(0.397319123049016,0.889004983339366,
-1.8934300912476));
#37695=CARTESIAN_POINT('Ctrl Pts',(0.54846316864109,0.803242517078114,-1.90625396287727));
#37696=CARTESIAN_POINT('Ctrl Pts',(0.657061179243564,0.731431679270899,
-1.91563986981193));
#37697=CARTESIAN_POINT('Ctrl Pts',(0.837016667682568,0.506409290281685,
-1.93694382317187));
#37698=CARTESIAN_POINT('Ctrl Pts',(0.896708335504397,0.389439444790955,
-1.94644765605331));
#37699=CARTESIAN_POINT('Ctrl Pts',(0.961575479660275,0.163480681552635,
-1.96379887442898));
#37700=CARTESIAN_POINT('Ctrl Pts',(0.980196107359686,0.038092952714017,
-1.97297967779038));
#37701=CARTESIAN_POINT('Ctrl Pts',(0.949796426925323,-0.232115295912927,
-1.99307419258545));
#37702=CARTESIAN_POINT('Ctrl Pts',(0.910338156983532,-0.356057593387196,
-2.00248672788133));
#37703=CARTESIAN_POINT('Ctrl Pts',(0.787597338177096,-0.580417039662108,
-2.02137165311335));
#37704=CARTESIAN_POINT('Ctrl Pts',(0.705541931920849,-0.677858961903907,
-2.03061365747613));
#37705=CARTESIAN_POINT('Ctrl Pts',(0.506633724951066,-0.835677971904185,
-2.04936477089474));
#37706=CARTESIAN_POINT('Ctrl Pts',(0.393146281041908,-0.894898742571984,
-2.05863327258857));
#37707=CARTESIAN_POINT('Ctrl Pts',(0.132370167545827,-0.972251332822705,
-2.07873243056899));
#37708=CARTESIAN_POINT('Ctrl Pts',(0.00409184961383252,-0.975578594338933,
-2.08802219266169));
#37709=CARTESIAN_POINT('Ctrl Pts',(-0.225854147439267,-0.950466860502564,
-2.10509568956757));
#37710=CARTESIAN_POINT('Ctrl Pts',(-0.346100609615678,-0.914145414198234,
-2.1141999618899));
#37711=CARTESIAN_POINT('Ctrl Pts',(-0.588320648121434,-0.786121492823866,
-2.13445454703384));
#37712=CARTESIAN_POINT('Ctrl Pts',(-0.683052440276746,-0.695538874693907,
-2.14392566572338));
#37713=CARTESIAN_POINT('Ctrl Pts',(-0.825486585716714,-0.522102941548968,
-2.16048705452036));
#37714=CARTESIAN_POINT('Ctrl Pts',(-0.88524530347349,-0.414549954481618,
-2.16941649293993));
#37715=CARTESIAN_POINT('Ctrl Pts',(-0.959910000303239,-0.184617722335589,
-2.18729260948374));
#37716=CARTESIAN_POINT('Ctrl Pts',(-0.974739175019372,-0.0624749986378993,
-2.19622204790341));
#37717=CARTESIAN_POINT('Ctrl Pts',(-0.961371621012054,0.161553609341058,
-2.21278343670051));
#37718=CARTESIAN_POINT('Ctrl Pts',(-0.937929646660382,0.290510179513995,
-2.22225455539021));
#37719=CARTESIAN_POINT('Ctrl Pts',(-0.817133378498529,0.536414496466949,
-2.24250914053417));
#37720=CARTESIAN_POINT('Ctrl Pts',(-0.741165879725255,0.636451480916389,
-2.25161341285639));
#37721=CARTESIAN_POINT('Ctrl Pts',(-0.569841157284644,0.791865766674308,
-2.26868690976221));
#37722=CARTESIAN_POINT('Ctrl Pts',(-0.464080472392293,0.864536772252294,
-2.27797667185481));
#37723=CARTESIAN_POINT('Ctrl Pts',(-0.207609487844049,0.955147139613417,
-2.29807582983535));
#37724=CARTESIAN_POINT('Ctrl Pts',(-0.0809805019614242,0.973898127262912,
-2.30734433152936));
#37725=CARTESIAN_POINT('Ctrl Pts',(0.172699493612978,0.963045728321461,
-2.32609544494811));
#37726=CARTESIAN_POINT('Ctrl Pts',(0.296347838905494,0.932400914526657,
-2.33533744931096));
#37727=CARTESIAN_POINT('Ctrl Pts',(0.527483844276784,0.822954047256741,
-2.35422237454296));
#37728=CARTESIAN_POINT('Ctrl Pts',(0.63223052539128,0.745838672878272,-2.36363490983875));
#37729=CARTESIAN_POINT('Ctrl Pts',(0.815578016510061,0.54503943060626,-2.38372942463377));
#37730=CARTESIAN_POINT('Ctrl Pts',(0.874175039145352,0.432633028397659,
-2.39291022799515));
#37731=CARTESIAN_POINT('Ctrl Pts',(0.954433739868647,0.211672285202659,
-2.41026144637082));
#37732=CARTESIAN_POINT('Ctrl Pts',(0.974849576921623,0.0819486036372085,
-2.41976527925227));
#37733=CARTESIAN_POINT('Ctrl Pts',(0.961425884758652,-0.205868800031195,
-2.44106923261221));
#37734=CARTESIAN_POINT('Ctrl Pts',(0.915734610801321,-0.327781194058935,
-2.45045513954686));
#37735=CARTESIAN_POINT('Ctrl Pts',(0.843810636917665,-0.485979377100993,
-2.4632790111765));
#37736=CARTESIAN_POINT('Ctrl Pts',(0.775799049655213,-0.604344034746782,
-2.47311764157039));
#37737=CARTESIAN_POINT('Ctrl Pts',(0.567537098494519,-0.795851039430973,
-2.49403706572968));
#37738=CARTESIAN_POINT('Ctrl Pts',(0.461411930121146,-0.860991364727363,
-2.50306717447086));
#37739=CARTESIAN_POINT('Ctrl Pts',(0.247958153459295,-0.943253500169966,
-2.51994968627787));
#37740=CARTESIAN_POINT('Ctrl Pts',(0.122238049409578,-0.973826816597205,
-2.52931001330053));
#37741=CARTESIAN_POINT('Ctrl Pts',(-0.150080047920812,-0.965863184981856,
-2.54944566669569));
#37742=CARTESIAN_POINT('Ctrl Pts',(-0.273980275415711,-0.937902949273016,
-2.55864583193933));
#37743=CARTESIAN_POINT('Ctrl Pts',(-0.475482963183443,-0.85047724750135,
-2.57486277531498));
#37744=CARTESIAN_POINT('Ctrl Pts',(-0.588929238049097,-0.786818991819914,
-2.58426441583404));
#37745=CARTESIAN_POINT('Ctrl Pts',(-0.785433476719409,-0.581830715298288,
-2.60523946729291));
#37746=CARTESIAN_POINT('Ctrl Pts',(-0.855362821274645,-0.473163846227886,
-2.61459220497182));
#37747=CARTESIAN_POINT('Ctrl Pts',(-0.949273543111333,-0.237088972514631,
-2.63336198978761));
#37748=CARTESIAN_POINT('Ctrl Pts',(-0.971510997389175,-0.113855934794878,
-2.64244533376835));
#37749=CARTESIAN_POINT('Ctrl Pts',(-0.967127048588767,0.142400130630832,
-2.6613655301193));
#37750=CARTESIAN_POINT('Ctrl Pts',(-0.939921400836311,0.270402106005835,
-2.67083497796768));
#37751=CARTESIAN_POINT('Ctrl Pts',(-0.831398503477933,0.520639551586384,
-2.69099843236003));
#37752=CARTESIAN_POINT('Ctrl Pts',(-0.752647366453703,0.619477319761821,
-2.70014702914963));
#37753=CARTESIAN_POINT('Ctrl Pts',(-0.587553439321292,0.78147175448688,
-2.7172161165589));
#37754=CARTESIAN_POINT('Ctrl Pts',(-0.477728333010138,0.854036407356267,
-2.726745231308));
#37755=CARTESIAN_POINT('Ctrl Pts',(-0.245237492311451,0.946238192940212,
-2.7452391103046));
#37756=CARTESIAN_POINT('Ctrl Pts',(-0.124140916952226,0.968825910384071,
-2.75417839311363));
#37757=CARTESIAN_POINT('Ctrl Pts',(0.100728002832586,0.969677678031108,
-2.77077257638251));
#37758=CARTESIAN_POINT('Ctrl Pts',(0.230717602518166,0.954356429549928,
-2.78023178511994));
#37759=CARTESIAN_POINT('Ctrl Pts',(0.483614457581182,0.849446199253669,
-2.80047292804102));
#37760=CARTESIAN_POINT('Ctrl Pts',(0.58837648052914,0.779893647824787,-2.80958656015487));
#37761=CARTESIAN_POINT('Ctrl Pts',(0.754474219189733,0.618540796080957,
-2.82667914408813));
#37762=CARTESIAN_POINT('Ctrl Pts',(0.833559877872636,0.517619827754594,
-2.83596184443618));
#37763=CARTESIAN_POINT('Ctrl Pts',(0.940190436386863,0.267335418003295,
-2.85606336908445));
#37764=CARTESIAN_POINT('Ctrl Pts',(0.966923459393059,0.142014500699582,
-2.86534081776185));
#37765=CARTESIAN_POINT('Ctrl Pts',(0.972003626913642,-0.111877781866752,
-2.88409490798249));
#37766=CARTESIAN_POINT('Ctrl Pts',(0.949143248594239,-0.237090541107098,
-2.89332941226818));
#37767=CARTESIAN_POINT('Ctrl Pts',(0.854532540396046,-0.474555800893968,
-2.912203936861));
#37768=CARTESIAN_POINT('Ctrl Pts',(0.784113881905413,-0.584062332473451,
-2.92162463589442));
#37769=CARTESIAN_POINT('Ctrl Pts',(0.596737771337372,-0.778136224042799,
-2.94156409432769));
#37770=CARTESIAN_POINT('Ctrl Pts',(0.490136620493726,-0.843165130861668,
-2.95061838510722));
#37771=CARTESIAN_POINT('Ctrl Pts',(0.394089576350919,-0.885695643716614,
-2.95837453804489));
#37772=CARTESIAN_POINT('Ctrl Pts',(-0.7601495323018,1.010461337524,-1.070459688113));
#37773=CARTESIAN_POINT('Ctrl Pts',(-0.5217111845523,1.189833661624,-1.087359779305));
#37774=CARTESIAN_POINT('Ctrl Pts',(0.08630816170208,1.371705237335,-1.121159961689));
#37775=CARTESIAN_POINT('Ctrl Pts',(0.9577659231642,0.986014487342,-1.171860235265));
#37776=CARTESIAN_POINT('Ctrl Pts',(1.36872301644,0.1263081428663,-1.222560508841));
#37777=CARTESIAN_POINT('Ctrl Pts',(1.121999630998,-0.7940472417276,-1.273260782417));
#37778=CARTESIAN_POINT('Ctrl Pts',(0.3360773550257,-1.332833081702,-1.323961055993));
#37779=CARTESIAN_POINT('Ctrl Pts',(-0.6113435996505,-1.231117050995,-1.374661329569));
#37780=CARTESIAN_POINT('Ctrl Pts',(-1.264982148074,-0.5377836494768,-1.425361603145));
#37781=CARTESIAN_POINT('Ctrl Pts',(-1.310728040867,0.4139841258882,-1.476061876721));
#37782=CARTESIAN_POINT('Ctrl Pts',(-0.7265983274592,1.16681007679,-1.526762150297));
#37783=CARTESIAN_POINT('Ctrl Pts',(0.2067011941596,1.358920713391,-1.577462423873));
#37784=CARTESIAN_POINT('Ctrl Pts',(1.040669609023,0.8979964642824,-1.628162697449));
#37785=CARTESIAN_POINT('Ctrl Pts',(1.374540008523,0.005536359898125,-1.678862971025));
#37786=CARTESIAN_POINT('Ctrl Pts',(1.047869610836,-0.8895842651211,-1.729563244601));
#37787=CARTESIAN_POINT('Ctrl Pts',(0.2176412060017,-1.357211550025,-1.780263518177));
#37788=CARTESIAN_POINT('Ctrl Pts',(-0.7171755664079,-1.172625299503,-1.830963791753));
#37789=CARTESIAN_POINT('Ctrl Pts',(-1.307350700813,-0.4245291876451,-1.881664065329));
#37790=CARTESIAN_POINT('Ctrl Pts',(-1.26927313384,0.5275761535541,-1.932364338905));
#37791=CARTESIAN_POINT('Ctrl Pts',(-0.621241195291,1.226152626448,-1.983064612481));
#37792=CARTESIAN_POINT('Ctrl Pts',(0.3253307286306,1.335496463145,-2.033764886057));
#37793=CARTESIAN_POINT('Ctrl Pts',(1.115563646671,0.8030620377886,-2.084465159633));
#37794=CARTESIAN_POINT('Ctrl Pts',(1.369707912366,-0.115287119011,-2.135165433209));
#37795=CARTESIAN_POINT('Ctrl Pts',(0.9656334669738,-0.978234581483,-2.185865706785));
#37796=CARTESIAN_POINT('Ctrl Pts',(0.0975199199624,-1.371087433381,-2.236565980361));
#37797=CARTESIAN_POINT('Ctrl Pts',(-0.8174571915112,-1.105058638105,-2.287266253937));
#37798=CARTESIAN_POINT('Ctrl Pts',(-1.339602034034,-0.3079894137849,-2.337966527513));
#37799=CARTESIAN_POINT('Ctrl Pts',(-1.217995246873,0.6370853700088,-2.388666801089));
#37800=CARTESIAN_POINT('Ctrl Pts',(-0.5110774485679,1.276006212291,-2.439367074665));
#37801=CARTESIAN_POINT('Ctrl Pts',(0.4414465317312,1.301736975613,-2.490067348241));
#37802=CARTESIAN_POINT('Ctrl Pts',(1.18180981307,0.7019131060313,-2.540767621817));
#37803=CARTESIAN_POINT('Ctrl Pts',(1.354330828351,-0.23521934487,-2.591467895393));
#37804=CARTESIAN_POINT('Ctrl Pts',(0.8757194191373,-1.059311028855,-2.642168168969));
#37805=CARTESIAN_POINT('Ctrl Pts',(0.2768459088523,-1.269347487952,-2.675968351353));
#37806=CARTESIAN_POINT('Ctrl Pts',(-0.02148540425545,-1.264277581662,-2.692868442545));
#37807=CARTESIAN_POINT('Ctrl Pts',(-0.6982454862957,0.9281727318386,-1.129911420741));
#37808=CARTESIAN_POINT('Ctrl Pts',(-0.479224763397,1.092937571317,-1.146811511933));
#37809=CARTESIAN_POINT('Ctrl Pts',(0.07927951248811,1.259998131679,-1.180611694317));
#37810=CARTESIAN_POINT('Ctrl Pts',(0.8797686565066,0.905716751708,-1.231311967893));
#37811=CARTESIAN_POINT('Ctrl Pts',(1.257258772921,0.1160220284182,-1.282012241469));
#37812=CARTESIAN_POINT('Ctrl Pts',(1.030627718204,-0.7293826791723,-1.332712515045));
#37813=CARTESIAN_POINT('Ctrl Pts',(0.3087083346382,-1.224291594926,-1.383412788621));
#37814=CARTESIAN_POINT('Ctrl Pts',(-0.561557813157,-1.130858978964,-1.434113062197));
#37815=CARTESIAN_POINT('Ctrl Pts',(-1.161966215335,-0.4939883403121,-1.484813335773));
#37816=CARTESIAN_POINT('Ctrl Pts',(-1.203986714989,0.3802706375734,-1.535513609349));
#37817=CARTESIAN_POINT('Ctrl Pts',(-0.6674265798232,1.071788950545,-1.586213882925));
#37818=CARTESIAN_POINT('Ctrl Pts',(0.1898681373872,1.248254736783,-1.636914156501));
#37819=CARTESIAN_POINT('Ctrl Pts',(0.9559209423246,0.8248666232761,-1.687614430077));
#37820=CARTESIAN_POINT('Ctrl Pts',(1.262602048544,0.005085497188518,-1.738314703653));
#37821=CARTESIAN_POINT('Ctrl Pts',(0.9625345999714,-0.8171394855951,-1.789014977229));
#37822=CARTESIAN_POINT('Ctrl Pts',(0.1999172311038,-1.246684761989,-1.839715250805));
#37823=CARTESIAN_POINT('Ctrl Pts',(-0.6587711770466,-1.077130600889,-1.890415524381));
#37824=CARTESIAN_POINT('Ctrl Pts',(-1.20088441426,-0.3899569446243,-1.941115797957));
#37825=CARTESIAN_POINT('Ctrl Pts',(-1.165907757512,0.4846121088583,-1.991816071533));
#37826=CARTESIAN_POINT('Ctrl Pts',(-0.5706493815754,1.126298840617,-2.042516345109));
#37827=CARTESIAN_POINT('Ctrl Pts',(0.2988368777019,1.226738079456,-2.093216618685));
#37828=CARTESIAN_POINT('Ctrl Pts',(1.024715859004,0.7376633402686,-2.143916892261));
#37829=CARTESIAN_POINT('Ctrl Pts',(1.258163462203,-0.1058985200368,-2.194617165837));
#37830=CARTESIAN_POINT('Ctrl Pts',(0.8869954937535,-0.8985704154689,-2.245317439413));
#37831=CARTESIAN_POINT('Ctrl Pts',(0.08957822249982,-1.259430639622,-2.296017712989));
#37832=CARTESIAN_POINT('Ctrl Pts',(-0.7508862006194,-1.015066343344,-2.346717986565));
#37833=CARTESIAN_POINT('Ctrl Pts',(-1.230509306326,-0.2829077817768,-2.397418260141));
#37834=CARTESIAN_POINT('Ctrl Pts',(-1.118805770864,0.585203259478,-2.448118533717));
#37835=CARTESIAN_POINT('Ctrl Pts',(-0.4694570034523,1.172092516481,-2.498818807293));
#37836=CARTESIAN_POINT('Ctrl Pts',(0.4054965965563,1.195727852142,-2.549519080869));
#37837=CARTESIAN_POINT('Ctrl Pts',(1.085567158264,0.6447516406069,-2.600219354445));
#37838=CARTESIAN_POINT('Ctrl Pts',(1.244038636693,-0.216063864892,-2.650919628021));
#37839=CARTESIAN_POINT('Ctrl Pts',(0.8044037464872,-0.973044267016,-2.701619901597));
#37840=CARTESIAN_POINT('Ctrl Pts',(0.2543005001532,-1.165976056474,-2.735420083981));
#37841=CARTESIAN_POINT('Ctrl Pts',(-0.01973570449643,-1.161319026465,-2.752320175173));
#37842=CARTESIAN_POINT('Ctrl Pts',(-0.6363414402896,0.8458841261532,-1.189363153369));
#37843=CARTESIAN_POINT('Ctrl Pts',(-0.4367383422416,0.9960414810095,-1.206263244561));
#37844=CARTESIAN_POINT('Ctrl Pts',(0.07225086327415,1.148291026024,-1.240063426945));
#37845=CARTESIAN_POINT('Ctrl Pts',(0.8017713898489,0.825419016074,-1.290763700521));
#37846=CARTESIAN_POINT('Ctrl Pts',(1.145794529402,0.10573591397,-1.341463974097));
#37847=CARTESIAN_POINT('Ctrl Pts',(0.9392558054095,-0.664718116617,-1.392164247673));
#37848=CARTESIAN_POINT('Ctrl Pts',(0.2813393142507,-1.11575010815,-1.442864521249));
#37849=CARTESIAN_POINT('Ctrl Pts',(-0.5117720266635,-1.030600906933,-1.493564794825));
#37850=CARTESIAN_POINT('Ctrl Pts',(-1.058950282596,-0.4501930311474,-1.544265068401));
#37851=CARTESIAN_POINT('Ctrl Pts',(-1.097245389111,0.3465571492585,-1.594965341977));
#37852=CARTESIAN_POINT('Ctrl Pts',(-0.6082548321872,0.9767678242997,-1.645665615553));
#37853=CARTESIAN_POINT('Ctrl Pts',(0.1730350806147,1.137588760174,-1.696365889129));
#37854=CARTESIAN_POINT('Ctrl Pts',(0.8711722756261,0.7517367822698,-1.747066162705));
#37855=CARTESIAN_POINT('Ctrl Pts',(1.150664088565,0.004634634478915,-1.797766436281));
#37856=CARTESIAN_POINT('Ctrl Pts',(0.877199589107,-0.7446947060692,-1.848466709857));
#37857=CARTESIAN_POINT('Ctrl Pts',(0.1821932562059,-1.136157973952,-1.899166983433));
#37858=CARTESIAN_POINT('Ctrl Pts',(-0.6003667876853,-0.9816359022759,-1.949867257009));
#37859=CARTESIAN_POINT('Ctrl Pts',(-1.094418127707,-0.3553847016034,-2.000567530585));
#37860=CARTESIAN_POINT('Ctrl Pts',(-1.062542381185,0.4416480641625,-2.051267804161));
#37861=CARTESIAN_POINT('Ctrl Pts',(-0.5200575678599,1.026445054786,-2.101968077737));
#37862=CARTESIAN_POINT('Ctrl Pts',(0.2723430267731,1.117979695766,-2.152668351313));
#37863=CARTESIAN_POINT('Ctrl Pts',(0.933868071336,0.6722646427485,-2.203368624889));
#37864=CARTESIAN_POINT('Ctrl Pts',(1.146619012041,-0.09650992106268,-2.254068898465));
#37865=CARTESIAN_POINT('Ctrl Pts',(0.8083575205332,-0.8189062494547,-2.304769172041));
#37866=CARTESIAN_POINT('Ctrl Pts',(0.08163652503724,-1.147773845863,-2.355469445617));
#37867=CARTESIAN_POINT('Ctrl Pts',(-0.6843152097275,-0.9250740485843,-2.406169719193));
#37868=CARTESIAN_POINT('Ctrl Pts',(-1.121416578618,-0.2578261497687,-2.456869992769));
#37869=CARTESIAN_POINT('Ctrl Pts',(-1.019616294854,0.5333211489471,-2.507570266345));
#37870=CARTESIAN_POINT('Ctrl Pts',(-0.4278365583367,1.068178820671,-2.558270539921));
#37871=CARTESIAN_POINT('Ctrl Pts',(0.3695466613813,1.089718728671,-2.608970813497));
#37872=CARTESIAN_POINT('Ctrl Pts',(0.9893245034571,0.5875901751825,-2.659671087073));
#37873=CARTESIAN_POINT('Ctrl Pts',(1.133746445034,-0.1969083849139,-2.710371360649));
#37874=CARTESIAN_POINT('Ctrl Pts',(0.7330880738372,-0.8867775051772,-2.761071634225));
#37875=CARTESIAN_POINT('Ctrl Pts',(0.2317550914541,-1.062604624995,-2.794871816609));
#37876=CARTESIAN_POINT('Ctrl Pts',(-0.01798600473741,-1.058360471267,-2.811771907801));
#37877=CARTESIAN_POINT('Ctrl Pts',(-0.5744373942835,0.7635955204679,-1.248814885998));
#37878=CARTESIAN_POINT('Ctrl Pts',(-0.3942519210863,0.8991453907025,-1.26571497719));
#37879=CARTESIAN_POINT('Ctrl Pts',(0.06522221406019,1.036583920368,-1.299515159574));
#37880=CARTESIAN_POINT('Ctrl Pts',(0.7237741231913,0.74512128044,-1.35021543315));
#37881=CARTESIAN_POINT('Ctrl Pts',(1.034330285883,0.09544979952193,-1.400915706726));
#37882=CARTESIAN_POINT('Ctrl Pts',(0.8478838926151,-0.6000535540617,-1.451615980302));
#37883=CARTESIAN_POINT('Ctrl Pts',(0.2539702938632,-1.007208621374,-1.502316253878));
#37884=CARTESIAN_POINT('Ctrl Pts',(-0.46198624017,-0.9303428349025,-1.553016527454));
#37885=CARTESIAN_POINT('Ctrl Pts',(-0.955934349857,-0.4063977219828,-1.60371680103));
#37886=CARTESIAN_POINT('Ctrl Pts',(-0.9905040632336,0.3128436609437,-1.654417074606));
#37887=CARTESIAN_POINT('Ctrl Pts',(-0.5490830845512,0.8817466980546,-1.705117348182));
#37888=CARTESIAN_POINT('Ctrl Pts',(0.1562020238423,1.026922783566,-1.755817621758));
#37889=CARTESIAN_POINT('Ctrl Pts',(0.7864236089275,0.6786069412635,-1.806517895334));
#37890=CARTESIAN_POINT('Ctrl Pts',(1.038726128586,0.004183771769308,-1.85721816891));
#37891=CARTESIAN_POINT('Ctrl Pts',(0.7918645782425,-0.6722499265432,-1.907918442486));
#37892=CARTESIAN_POINT('Ctrl Pts',(0.1644692813081,-1.025631185916,-1.958618716062));
#37893=CARTESIAN_POINT('Ctrl Pts',(-0.541962398324,-0.8861412036624,-2.009318989638));
#37894=CARTESIAN_POINT('Ctrl Pts',(-0.9879518411537,-0.3208124585826,-2.060019263214));
#37895=CARTESIAN_POINT('Ctrl Pts',(-0.9591770048575,0.3986840194666,-2.11071953679));
#37896=CARTESIAN_POINT('Ctrl Pts',(-0.4694657541443,0.9265912689544,-2.161419810366));
#37897=CARTESIAN_POINT('Ctrl Pts',(0.2458491758444,1.009221312076,-2.212120083942));
#37898=CARTESIAN_POINT('Ctrl Pts',(0.8430202836683,0.6068659452285,-2.262820357518));
#37899=CARTESIAN_POINT('Ctrl Pts',(1.035074561878,-0.08712132208854,-2.313520631094));
#37900=CARTESIAN_POINT('Ctrl Pts',(0.7297195473129,-0.7392420834405,-2.36422090467));
#37901=CARTESIAN_POINT('Ctrl Pts',(0.07369482757466,-1.036117052103,-2.414921178246));
#37902=CARTESIAN_POINT('Ctrl Pts',(-0.6177442188356,-0.8350817538242,-2.465621451822));
#37903=CARTESIAN_POINT('Ctrl Pts',(-1.01232385091,-0.2327445177605,-2.516321725398));
#37904=CARTESIAN_POINT('Ctrl Pts',(-0.9204268188452,0.4814390384163,-2.567021998974));
#37905=CARTESIAN_POINT('Ctrl Pts',(-0.3862161132211,0.9642651248607,-2.61772227255));
#37906=CARTESIAN_POINT('Ctrl Pts',(0.3335967262064,0.9837096051999,-2.668422546126));
#37907=CARTESIAN_POINT('Ctrl Pts',(0.8930818486504,0.5304287097581,-2.719122819702));
#37908=CARTESIAN_POINT('Ctrl Pts',(1.023454253376,-0.1777529049358,-2.769823093278));
#37909=CARTESIAN_POINT('Ctrl Pts',(0.6617724011872,-0.8005107433383,-2.820523366854));
#37910=CARTESIAN_POINT('Ctrl Pts',(0.209209682755,-0.9592331935163,-2.854323549238));
#37911=CARTESIAN_POINT('Ctrl Pts',(-0.01623630497839,-0.9554019160702,-2.87122364043));
#37912=CARTESIAN_POINT('',(-0.259620813216912,1.22212682904672,-1.11035239491773));
#37913=CARTESIAN_POINT('Ctrl Pts',(-0.259550427067826,1.2218848440576,-1.11004989456032));
#37914=CARTESIAN_POINT('Ctrl Pts',(-0.176089993779685,1.23970121447083,
-1.11497869489726));
#37915=CARTESIAN_POINT('Ctrl Pts',(-0.0908079081753038,1.24915717847783,
-1.11989604862454));
#37916=CARTESIAN_POINT('Ctrl Pts',(0.078907392811349,1.2503536393333,-1.12957295158789));
#37917=CARTESIAN_POINT('Ctrl Pts',(0.162375297690802,1.24228645451723,-1.13424992803467));
#37918=CARTESIAN_POINT('Ctrl Pts',(0.403734930196471,1.19332043365468,-1.14828701945804));
#37919=CARTESIAN_POINT('Ctrl Pts',(0.556180896601559,1.12984504867094,-1.15772076971209));
#37920=CARTESIAN_POINT('Ctrl Pts',(0.79311118448388,0.973386735470281,-1.17408123400961));
#37921=CARTESIAN_POINT('Ctrl Pts',(0.919885403903609,0.869811354026893,
-1.18306885097986));
#37922=CARTESIAN_POINT('Ctrl Pts',(1.12233993543671,0.571332489916865,-1.20376271043536));
#37923=CARTESIAN_POINT('Ctrl Pts',(1.18717976490115,0.420371499103929,-1.21315322596248));
#37924=CARTESIAN_POINT('Ctrl Pts',(1.26532256770491,0.0628365754308183,
-1.23413706582087));
#37925=CARTESIAN_POINT('Ctrl Pts',(1.25085721746949,-0.105155817320906,
-1.24338943208094));
#37926=CARTESIAN_POINT('Ctrl Pts',(1.20048510106074,-0.379552281401981,
-1.25946420042759));
#37927=CARTESIAN_POINT('Ctrl Pts',(1.1419432982034,-0.531453654769294,-1.26876281109958));
#37928=CARTESIAN_POINT('Ctrl Pts',(1.01524185767701,-0.73350518608508,-1.28235787310138));
#37929=CARTESIAN_POINT('Ctrl Pts',(0.967392529020281,-0.795523411523133,
-1.28673633950651));
#37930=CARTESIAN_POINT('Ctrl Pts',(0.857289770780207,-0.912799058533321,
-1.29591217872114));
#37931=CARTESIAN_POINT('Ctrl Pts',(0.795144597656944,-0.967011082703482,
-1.30064043572717));
#37932=CARTESIAN_POINT('Ctrl Pts',(0.599484790288714,-1.10705926876841,
-1.31453434606277));
#37933=CARTESIAN_POINT('Ctrl Pts',(0.453032617993671,-1.17555061064353,
-1.32374476309936));
#37934=CARTESIAN_POINT('Ctrl Pts',(0.261514424480917,-1.22293451905085,
-1.33491640565985));
#37935=CARTESIAN_POINT('Ctrl Pts',(0.223775349447442,-1.23038193593054,
-1.337082972641));
#37936=CARTESIAN_POINT('Ctrl Pts',(0.0402342673113264,-1.25757860289646,
-1.34762444380788));
#37937=CARTESIAN_POINT('Ctrl Pts',(-0.10904320782717,-1.25282127697789,
-1.35615292953458));
#37938=CARTESIAN_POINT('Ctrl Pts',(-0.333345813583322,-1.20674934849765,
-1.36937522906284));
#37939=CARTESIAN_POINT('Ctrl Pts',(-0.412152165025727,-1.18248733842875,
-1.37410284257688));
#37940=CARTESIAN_POINT('Ctrl Pts',(-0.560423900027475,-1.12010380073129,
-1.38327871661146));
#37941=CARTESIAN_POINT('Ctrl Pts',(-0.629363619347819,-1.082889305217,-1.38765781242608));
#37942=CARTESIAN_POINT('Ctrl Pts',(-0.826731718365693,-0.950152059149684,
-1.40121639690562));
#37943=CARTESIAN_POINT('Ctrl Pts',(-0.94156875397672,-0.835743004688424,
-1.41047617204213));
#37944=CARTESIAN_POINT('Ctrl Pts',(-1.09839950351904,-0.607361502190615,
-1.4264405463437));
#37945=CARTESIAN_POINT('Ctrl Pts',(-1.1806943421766,-0.459743797365995,
-1.43571505413252));
#37946=CARTESIAN_POINT('Ctrl Pts',(-1.25530379565404,-0.100950817236402,
-1.45672466500082));
#37947=CARTESIAN_POINT('Ctrl Pts',(-1.25775645832347,0.0628411125803556,
-1.46608791139449));
#37948=CARTESIAN_POINT('Ctrl Pts',(-1.1958299869675,0.413688700430408,-1.48653374157504));
#37949=CARTESIAN_POINT('Ctrl Pts',(-1.1241484394092,0.560291562992558,-1.49549654622063));
#37950=CARTESIAN_POINT('Ctrl Pts',(-0.969749982883845,0.803367902875652,
-1.51208747191069));
#37951=CARTESIAN_POINT('Ctrl Pts',(-0.856799218163433,0.923462389601029,
-1.52150714900259));
#37952=CARTESIAN_POINT('Ctrl Pts',(-0.656371658525956,1.06719626571009,
-1.53556970304047));
#37953=CARTESIAN_POINT('Ctrl Pts',(-0.582976315656834,1.10899652214491,
-1.54027990124189));
#37954=CARTESIAN_POINT('Ctrl Pts',(-0.426276585958984,1.17773985476701,
-1.55003464226733));
#37955=CARTESIAN_POINT('Ctrl Pts',(-0.343814511766357,1.20407158687264,
-1.55499493675363));
#37956=CARTESIAN_POINT('Ctrl Pts',(-0.259587618866585,1.2218769438964,-1.5599669049452));
#37957=CARTESIAN_POINT('',(-0.20156254994044,0.948825615807999,-1.27169584474002));
#37958=CARTESIAN_POINT('Ctrl Pts',(-0.201438348341829,0.948254165709337,
-1.27165078927618));
#37959=CARTESIAN_POINT('Ctrl Pts',(-0.0987243392846107,0.970265772525782,
-1.27940722318184));
#37960=CARTESIAN_POINT('Ctrl Pts',(0.025742728243312,0.980269531029446,
-1.28846139011945));
#37961=CARTESIAN_POINT('Ctrl Pts',(0.291387332434426,0.933304243270982,
-1.30840061727523));
#37962=CARTESIAN_POINT('Ctrl Pts',(0.412706897305448,0.886059866868016,
-1.31782131630864));
#37963=CARTESIAN_POINT('Ctrl Pts',(0.628779001349306,0.749481019437201,
-1.33669584090143));
#37964=CARTESIAN_POINT('Ctrl Pts',(0.720840663164924,0.661586296061749,
-1.34593034518707));
#37965=CARTESIAN_POINT('Ctrl Pts',(0.865891373452356,0.453145919229823,
-1.36468443540759));
#37966=CARTESIAN_POINT('Ctrl Pts',(0.917884397731031,0.336027550648247,
-1.37396188408488));
#37967=CARTESIAN_POINT('Ctrl Pts',(0.978638449230792,0.0708459015852234,
-1.39406340873307));
#37968=CARTESIAN_POINT('Ctrl Pts',(0.973931484966908,-0.0572846090069489,
-1.40334610908117));
#37969=CARTESIAN_POINT('Ctrl Pts',(0.934315968934639,-0.285437655104263,
-1.42043869301452));
#37970=CARTESIAN_POINT('Ctrl Pts',(0.890402125861612,-0.403268946572158,
-1.42955232512848));
#37971=CARTESIAN_POINT('Ctrl Pts',(0.747386626902557,-0.636741734663472,
-1.44979346804974));
#37972=CARTESIAN_POINT('Ctrl Pts',(0.651197130204398,-0.7255089437353,-1.45925267678724));
#37973=CARTESIAN_POINT('Ctrl Pts',(0.468727345569633,-0.856930153167856,
-1.47584686005623));
#37974=CARTESIAN_POINT('Ctrl Pts',(0.35746278354269,-0.909795858308654,
-1.48478614286536));
#37975=CARTESIAN_POINT('Ctrl Pts',(0.1151570245764,-0.97177230097435,-1.50328002186201));
#37976=CARTESIAN_POINT('Ctrl Pts',(-0.0163478393052635,-0.977573473079552,
-1.51280913661105));
#37977=CARTESIAN_POINT('Ctrl Pts',(-0.24511756325168,-0.943476331507244,
-1.52987822402024));
#37978=CARTESIAN_POINT('Ctrl Pts',(-0.366912073350283,-0.909760707379217,
-1.53902682080977));
#37979=CARTESIAN_POINT('Ctrl Pts',(-0.601745916092746,-0.771019708663982,
-1.55919027520204));
#37980=CARTESIAN_POINT('Ctrl Pts',(-0.698962539434374,-0.683420729699734,
-1.56865972305043));
#37981=CARTESIAN_POINT('Ctrl Pts',(-0.853060563983216,-0.478627690499707,
-1.58757991940138));
#37982=CARTESIAN_POINT('Ctrl Pts',(-0.907464882095679,-0.365840031027934,
-1.59666326338209));
#37983=CARTESIAN_POINT('Ctrl Pts',(-0.970164031430921,-0.119629985848702,
-1.61543304819782));
#37984=CARTESIAN_POINT('Ctrl Pts',(-0.977417294464398,0.00938936091313193,
-1.62478578587667));
#37985=CARTESIAN_POINT('Ctrl Pts',(-0.938831912985746,0.290717066024108,
-1.64576083733552));
#37986=CARTESIAN_POINT('Ctrl Pts',(-0.884427664631876,0.408880548362682,
-1.65516247785461));
#37987=CARTESIAN_POINT('Ctrl Pts',(-0.772729409729853,0.598010361875847,
-1.67137942123023));
#37988=CARTESIAN_POINT('Ctrl Pts',(-0.688892984793735,0.693427839352897,
-1.68057958647389));
#37989=CARTESIAN_POINT('Ctrl Pts',(-0.47320522420946,0.859859072888397,
-1.70071523986905));
#37990=CARTESIAN_POINT('Ctrl Pts',(-0.353507651838696,0.908978961000481,
-1.71007556689172));
#37991=CARTESIAN_POINT('Ctrl Pts',(-0.132446689760698,0.967814534797143,
-1.72695807869875));
#37992=CARTESIAN_POINT('Ctrl Pts',(-0.00829769730840238,0.977449939050657,
-1.73598818743995));
#37993=CARTESIAN_POINT('Ctrl Pts',(0.272743269789283,0.944831723940328,
-1.75690761159923));
#37994=CARTESIAN_POINT('Ctrl Pts',(0.397319123049025,0.889004983339358,
-1.76674624199313));
#37995=CARTESIAN_POINT('Ctrl Pts',(0.548463168641115,0.803242517078102,
-1.77957011362282));
#37996=CARTESIAN_POINT('Ctrl Pts',(0.657061179243573,0.731431679270879,
-1.7889560205575));
#37997=CARTESIAN_POINT('Ctrl Pts',(0.837016667682552,0.506409290281711,
-1.81025997391745));
#37998=CARTESIAN_POINT('Ctrl Pts',(0.896708335504385,0.389439444790983,
-1.81976380679888));
#37999=CARTESIAN_POINT('Ctrl Pts',(0.961575479660269,0.163480681552666,
-1.83711502517455));
#38000=CARTESIAN_POINT('Ctrl Pts',(0.980196107359684,0.0380929527140501,
-1.84629582853592));
#38001=CARTESIAN_POINT('Ctrl Pts',(0.949796426925332,-0.232115295912896,
-1.86639034333097));
#38002=CARTESIAN_POINT('Ctrl Pts',(0.910338156983544,-0.356057593387167,
-1.8758028786268));
#38003=CARTESIAN_POINT('Ctrl Pts',(0.787597338177108,-0.580417039662094,
-1.89468780385886));
#38004=CARTESIAN_POINT('Ctrl Pts',(0.705541931920857,-0.6778589619039,-1.90392980822176));
#38005=CARTESIAN_POINT('Ctrl Pts',(0.506633724951068,-0.835677971904184,
-1.92268092164057));
#38006=CARTESIAN_POINT('Ctrl Pts',(0.393146281041906,-0.894898742571985,
-1.93194942333464));
#38007=CARTESIAN_POINT('Ctrl Pts',(0.132370167545825,-0.972251332822704,
-1.95204858131521));
#38008=CARTESIAN_POINT('Ctrl Pts',(0.00409184961383161,-0.975578594338933,
-1.96133834340777));
#38009=CARTESIAN_POINT('Ctrl Pts',(-0.225854147439271,-0.950466860502563,
-1.9784118403135));
#38010=CARTESIAN_POINT('Ctrl Pts',(-0.346100609615679,-0.914145414198233,
-1.98751611263562));
#38011=CARTESIAN_POINT('Ctrl Pts',(-0.588320648121432,-0.786121492823868,
-2.00777069777945));
#38012=CARTESIAN_POINT('Ctrl Pts',(-0.683052440276743,-0.69553887469391,
-2.01724181646912));
#38013=CARTESIAN_POINT('Ctrl Pts',(-0.825486585716711,-0.522102941548972,
-2.0338032052662));
#38014=CARTESIAN_POINT('Ctrl Pts',(-0.885245303473489,-0.414549954481621,
-2.04273264368591));
#38015=CARTESIAN_POINT('Ctrl Pts',(-0.959910000303239,-0.184617722335591,
-2.06060876022976));
#38016=CARTESIAN_POINT('Ctrl Pts',(-0.974739175019373,-0.0624749986379006,
-2.06953819864937));
#38017=CARTESIAN_POINT('Ctrl Pts',(-0.961371621012054,0.161553609341053,
-2.08609958744636));
#38018=CARTESIAN_POINT('Ctrl Pts',(-0.937929646660384,0.290510179513987,
-2.0955707061359));
#38019=CARTESIAN_POINT('Ctrl Pts',(-0.817133378498537,0.536414496466936,
-2.11582529127975));
#38020=CARTESIAN_POINT('Ctrl Pts',(-0.741165879725267,0.636451480916373,
-2.12492956360197));
#38021=CARTESIAN_POINT('Ctrl Pts',(-0.569841157284668,0.791865766674289,
-2.14200306050775));
#38022=CARTESIAN_POINT('Ctrl Pts',(-0.464080472392323,0.864536772252278,
-2.15129282260037));
#38023=CARTESIAN_POINT('Ctrl Pts',(-0.207609487844088,0.955147139613408,
-2.17139198058076));
#38024=CARTESIAN_POINT('Ctrl Pts',(-0.0809805019614702,0.973898127262907,
-2.18066048227463));
#38025=CARTESIAN_POINT('Ctrl Pts',(0.172699493612926,0.96304572832147,-2.19941159569329));
#38026=CARTESIAN_POINT('Ctrl Pts',(0.296347838905441,0.932400914526673,
-2.20865360005613));
#38027=CARTESIAN_POINT('Ctrl Pts',(0.527483844276734,0.822954047256773,
-2.22753852528824));
#38028=CARTESIAN_POINT('Ctrl Pts',(0.632230525391237,0.745838672878308,
-2.23695106058418));
#38029=CARTESIAN_POINT('Ctrl Pts',(0.815578016510035,0.545039430606301,
-2.25704557537929));
#38030=CARTESIAN_POINT('Ctrl Pts',(0.874175039145334,0.432633028397699,
-2.26622637874067));
#38031=CARTESIAN_POINT('Ctrl Pts',(0.954433739868639,0.211672285202696,
-2.28357759711632));
#38032=CARTESIAN_POINT('Ctrl Pts',(0.97484957692162,0.0819486036372458,
-2.29308142999772));
#38033=CARTESIAN_POINT('Ctrl Pts',(0.961425884758658,-0.205868800031201,
-2.31438538335767));
#38034=CARTESIAN_POINT('Ctrl Pts',(0.915734610801314,-0.327781194058943,
-2.32377129029236));
#38035=CARTESIAN_POINT('Ctrl Pts',(0.843810636917658,-0.485979377101017,
-2.33659516192202));
#38036=CARTESIAN_POINT('Ctrl Pts',(0.775799049655197,-0.604344034746789,
-2.34643379231593));
#38037=CARTESIAN_POINT('Ctrl Pts',(0.567537098494545,-0.795851039430955,
-2.36735321647528));
#38038=CARTESIAN_POINT('Ctrl Pts',(0.461411930121172,-0.860991364727349,
-2.37638332521648));
#38039=CARTESIAN_POINT('Ctrl Pts',(0.247958153459323,-0.943253500169958,
-2.39326583702354));
#38040=CARTESIAN_POINT('Ctrl Pts',(0.122238049409607,-0.973826816597201,
-2.40262616404625));
#38041=CARTESIAN_POINT('Ctrl Pts',(-0.150080047920781,-0.965863184981861,
-2.42276181744138));
#38042=CARTESIAN_POINT('Ctrl Pts',(-0.273980275415678,-0.937902949273026,
-2.43196198268497));
#38043=CARTESIAN_POINT('Ctrl Pts',(-0.475482963183398,-0.850477247501373,
-2.44817892606057));
#38044=CARTESIAN_POINT('Ctrl Pts',(-0.588929238049058,-0.786818991819945,
-2.45758056657959));
#38045=CARTESIAN_POINT('Ctrl Pts',(-0.785433476719383,-0.581830715298323,
-2.47855561803846));
#38046=CARTESIAN_POINT('Ctrl Pts',(-0.855362821274623,-0.473163846227926,
-2.48790835571739));
#38047=CARTESIAN_POINT('Ctrl Pts',(-0.949273543111316,-0.237088972514691,
-2.50667814053319));
#38048=CARTESIAN_POINT('Ctrl Pts',(-0.97151099738917,-0.113855934794938,
-2.51576148451392));
#38049=CARTESIAN_POINT('Ctrl Pts',(-0.967127048588774,0.142400130630789,
-2.53468168086486));
#38050=CARTESIAN_POINT('Ctrl Pts',(-0.939921400836323,0.270402106005793,
-2.54415112871322));
#38051=CARTESIAN_POINT('Ctrl Pts',(-0.831398503477957,0.520639551586347,
-2.56431458310557));
#38052=CARTESIAN_POINT('Ctrl Pts',(-0.752647366453729,0.619477319761789,
-2.57346317989518));
#38053=CARTESIAN_POINT('Ctrl Pts',(-0.587553439321323,0.781471754486857,
-2.59053226730448));
#38054=CARTESIAN_POINT('Ctrl Pts',(-0.477728333010171,0.854036407356249,
-2.60006138205362));
#38055=CARTESIAN_POINT('Ctrl Pts',(-0.245237492311489,0.946238192940202,
-2.61855526105023));
#38056=CARTESIAN_POINT('Ctrl Pts',(-0.124140916952267,0.968825910384066,
-2.62749454385925));
#38057=CARTESIAN_POINT('Ctrl Pts',(0.100728002832542,0.969677678031112,
-2.64408872712811));
#38058=CARTESIAN_POINT('Ctrl Pts',(0.230717602518123,0.954356429549939,
-2.65354793586552));
#38059=CARTESIAN_POINT('Ctrl Pts',(0.483614457581144,0.849446199253691,
-2.6737890787866));
#38060=CARTESIAN_POINT('Ctrl Pts',(0.588376480529104,0.779893647824814,
-2.68290271090044));
#38061=CARTESIAN_POINT('Ctrl Pts',(0.754474219189705,0.618540796080992,
-2.69999529483371));
#38062=CARTESIAN_POINT('Ctrl Pts',(0.833559877872614,0.51761982775463,-2.70927799518176));
#38063=CARTESIAN_POINT('Ctrl Pts',(0.940190436386853,0.267335418003333,
-2.7293795198301));
#38064=CARTESIAN_POINT('Ctrl Pts',(0.966923459393054,0.142014500699619,
-2.73865696850759));
#38065=CARTESIAN_POINT('Ctrl Pts',(0.972003626913646,-0.111877781866718,
-2.75741105872829));
#38066=CARTESIAN_POINT('Ctrl Pts',(0.949143248594248,-0.237090541107069,
-2.766645563014));
#38067=CARTESIAN_POINT('Ctrl Pts',(0.854532540396059,-0.474555800893944,
-2.78552008760676));
#38068=CARTESIAN_POINT('Ctrl Pts',(0.784113881905431,-0.584062332473427,
-2.79494078664008));
#38069=CARTESIAN_POINT('Ctrl Pts',(0.596737734874605,-0.77813626180894,
-2.81488024895344));
#38070=CARTESIAN_POINT('Ctrl Pts',(0.490136541954605,-0.843165179166,-2.82393454260568));
#38071=CARTESIAN_POINT('Ctrl Pts',(0.394089470014046,-0.88569569080355,
-2.83169069737786));
#38072=CARTESIAN_POINT('',(-0.2597459052318,1.222715038231,-1.110008417723));
#38073=CARTESIAN_POINT('Ctrl Pts',(0.4032259446541,-0.8662939895831,0.2012068049836));
#38074=CARTESIAN_POINT('Ctrl Pts',(0.1988067354564,-0.9614431303197,0.1843067137916));
#38075=CARTESIAN_POINT('Ctrl Pts',(-0.2791972885623,-1.000404435832,0.1505065314076));
#38076=CARTESIAN_POINT('Ctrl Pts',(-0.8628093649628,-0.5784589040704,0.09980625783161));
#38077=CARTESIAN_POINT('Ctrl Pts',(-1.031587111702,0.1215641209151,0.04910598425561));
#38078=CARTESIAN_POINT('Ctrl Pts',(-0.7046871460694,0.7631430988109,-0.001594289320396));
#38079=CARTESIAN_POINT('Ctrl Pts',(-0.03913198596358,1.037997497496,-0.0522945628964));
#38080=CARTESIAN_POINT('Ctrl Pts',(0.6452242121113,0.8140361126302,-0.1029948364724));
#38081=CARTESIAN_POINT('Ctrl Pts',(1.01951635945,0.1988868585002,-0.1536951100484));
#38082=CARTESIAN_POINT('Ctrl Pts',(0.9038754829091,-0.5118384187131,-0.2043953836244));
#38083=CARTESIAN_POINT('Ctrl Pts',(0.353873640358,-0.9765976243727,-0.2550956572004));
#38084=CARTESIAN_POINT('Ctrl Pts',(-0.3661836412597,-0.972048875589,-0.3057959307764));
#38085=CARTESIAN_POINT('Ctrl Pts',(-0.9102698778482,-0.5003780799473,-0.3564962043524));
#38086=CARTESIAN_POINT('Ctrl Pts',(-1.016922220489,0.211751438319,-0.4071964779284));
#38087=CARTESIAN_POINT('Ctrl Pts',(-0.6348884498779,0.8221229410644,-0.4578967515044));
#38088=CARTESIAN_POINT('Ctrl Pts',(0.0522435497898,1.037419917643,-0.5085970250804));
#38089=CARTESIAN_POINT('Ctrl Pts',(0.7142696989558,0.7541805295677,-0.5592972986564));
#38090=CARTESIAN_POINT('Ctrl Pts',(1.033050636552,0.1085166178039,-0.6099975722324));
#38091=CARTESIAN_POINT('Ctrl Pts',(0.8553948853012,-0.5892953964066,-0.6606978458084));
#38092=CARTESIAN_POINT('Ctrl Pts',(0.2666756396737,-1.003919108903,-0.7113981193844));
#38093=CARTESIAN_POINT('Ctrl Pts',(-0.4501956701808,-0.9361054067588,-0.7620983929604));
#38094=CARTESIAN_POINT('Ctrl Pts',(-0.9507236181379,-0.4184424405686,-0.8127986665364));
#38095=CARTESIAN_POINT('Ctrl Pts',(-0.9943774606619,0.3003047437805,-0.8634989401124));
#38096=CARTESIAN_POINT('Ctrl Pts',(-0.5601791680333,0.8747392613582,-0.9141992136884));
#38097=CARTESIAN_POINT('Ctrl Pts',(0.1432155101674,1.028814264539,-0.9648994872644));
#38098=CARTESIAN_POINT('Ctrl Pts',(0.777787369792,0.6884883897838,-1.01559976084));
#38099=CARTESIAN_POINT('Ctrl Pts',(1.038590425217,0.01730659751134,-1.066300034416));
#38100=CARTESIAN_POINT('Ctrl Pts',(0.8002943153164,-0.6621918796188,-1.117000307992));
#38101=CARTESIAN_POINT('Ctrl Pts',(0.1774146655216,-1.023471618362,-1.167700581568));
#38102=CARTESIAN_POINT('Ctrl Pts',(-0.5307266205799,-0.8929169151192,-1.218400855144));
#38103=CARTESIAN_POINT('Ctrl Pts',(-0.9838090336742,-0.3332710455254,-1.26910112872));
#38104=CARTESIAN_POINT('Ctrl Pts',(-0.9641778538747,0.3865433611684,-1.319801402296));
#38105=CARTESIAN_POINT('Ctrl Pts',(-0.4809837433131,0.920551356439,-1.370501675872));
#38106=CARTESIAN_POINT('Ctrl Pts',(-0.00531754485576,0.9817681674502,-1.404301858256));
#38107=CARTESIAN_POINT('Ctrl Pts',(0.2144112878497,0.9311735812793,-1.421201949448));
#38108=CARTESIAN_POINT('Ctrl Pts',(0.446679448338,-0.9596498600741,0.1417550723552));
#38109=CARTESIAN_POINT('Ctrl Pts',(0.220231074158,-1.065052714869,0.1248549811632));
#38110=CARTESIAN_POINT('Ctrl Pts',(-0.3092848872596,-1.10821267192,0.09105479877921));
#38111=CARTESIAN_POINT('Ctrl Pts',(-0.9557897160936,-0.6407963266799,0.04035452520321));
#38112=CARTESIAN_POINT('Ctrl Pts',(-1.14275573801,0.1346644361256,-0.0103457483728));
#38113=CARTESIAN_POINT('Ctrl Pts',(-0.780627511276,0.8453829494337,-0.0610460219488));
#38114=CARTESIAN_POINT('Ctrl Pts',(-0.04334903082087,1.149856936799,-0.1117462955248));
#38115=CARTESIAN_POINT('Ctrl Pts',(0.714756574921,0.9017604311867,-0.1624465691008));
#38116=CARTESIAN_POINT('Ctrl Pts',(1.129384185339,0.2203198316338,-0.2131468426768));
#38117=CARTESIAN_POINT('Ctrl Pts',(1.001281309958,-0.5669965078887,-0.2638471162528));
#38118=CARTESIAN_POINT('Ctrl Pts',(0.3920087101342,-1.081840327703,-0.3145473898288));
#38119=CARTESIAN_POINT('Ctrl Pts',(-0.4056452940017,-1.076801384589,-0.3652476634048));
#38120=CARTESIAN_POINT('Ctrl Pts',(-1.008364794643,-0.5543011497017,-0.4159479369808));
#38121=CARTESIAN_POINT('Ctrl Pts',(-1.126510489895,0.2345707584224,-0.4666482105568));
#38122=CARTESIAN_POINT('Ctrl Pts',(-0.7033069828653,0.9107187338744,-0.5173484841328));
#38123=CARTESIAN_POINT('Ctrl Pts',(0.05787355776263,1.149217114254,-0.5680487577088));
#38124=CARTESIAN_POINT('Ctrl Pts',(0.7912427246413,0.8354545320332,-0.6187490312848));
#38125=CARTESIAN_POINT('Ctrl Pts',(1.144376979106,0.1202108733795,-0.6694493048608));
#38126=CARTESIAN_POINT('Ctrl Pts',(0.94757621761,-0.6528006098439,-0.7201495784368));
#38127=CARTESIAN_POINT('Ctrl Pts',(0.2954138472336,-1.112106102512,-0.7708498520128));
#38128=CARTESIAN_POINT('Ctrl Pts',(-0.4987108500002,-1.036984480341,-0.8215501255888));
#38129=CARTESIAN_POINT('Ctrl Pts',(-1.053178018186,-0.4635357446425,-0.8722503991648));
#38130=CARTESIAN_POINT('Ctrl Pts',(-1.101536201866,0.3326669800482,-0.9229506727408));
#38131=CARTESIAN_POINT('Ctrl Pts',(-0.6205466812466,0.9690052336249,-0.9736509463168));
#38132=CARTESIAN_POINT('Ctrl Pts',(0.1586490798104,1.139684075936,-1.024351219893));
#38133=CARTESIAN_POINT('Ctrl Pts',(0.8616053551838,0.7626831016531,-1.075051493469));
#38134=CARTESIAN_POINT('Ctrl Pts',(1.150513761169,0.01917163697293,-1.125751767045));
#38135=CARTESIAN_POINT('Ctrl Pts',(0.8865377538647,-0.7335527572161,-1.176452040621));
#38136=CARTESIAN_POINT('Ctrl Pts',(0.1965336952469,-1.133765681352,-1.227152314197));
#38137=CARTESIAN_POINT('Ctrl Pts',(-0.5879201902604,-0.9891417959213,-1.277852587773));
#38138=CARTESIAN_POINT('Ctrl Pts',(-1.08982887202,-0.369185883835,-1.328552861349));
#38139=CARTESIAN_POINT('Ctrl Pts',(-1.068082144957,0.4281990720453,-1.379253134925));
#38140=CARTESIAN_POINT('Ctrl Pts',(-0.5328167891255,1.019754253199,-1.429953408501));
#38141=CARTESIAN_POINT('Ctrl Pts',(-0.005890588227703,1.087568072557,-1.463753590885));
#38142=CARTESIAN_POINT('Ctrl Pts',(0.2375172457128,1.031521178404,-1.480653682077));
#38143=CARTESIAN_POINT('Ctrl Pts',(0.490132952022,-1.053005730565,0.08230333972681));
#38144=CARTESIAN_POINT('Ctrl Pts',(0.2416554128596,-1.168662299419,0.06540324853481));
#38145=CARTESIAN_POINT('Ctrl Pts',(-0.3393724859569,-1.216020908007,0.03160306615081));
#38146=CARTESIAN_POINT('Ctrl Pts',(-1.048770067224,-0.7031337492895,-0.01909720742519));
#38147=CARTESIAN_POINT('Ctrl Pts',(-1.253924364317,0.1477647513361,-0.0697974810012));
#38148=CARTESIAN_POINT('Ctrl Pts',(-0.8565678764825,0.9276228000565,-0.1204977545772));
#38149=CARTESIAN_POINT('Ctrl Pts',(-0.04756607567816,1.261716376102,-0.1711980281532));
#38150=CARTESIAN_POINT('Ctrl Pts',(0.7842889377307,0.9894847497432,-0.2218983017292));
#38151=CARTESIAN_POINT('Ctrl Pts',(1.239252011228,0.2417528047674,-0.2725985753052));
#38152=CARTESIAN_POINT('Ctrl Pts',(1.098687137006,-0.6221545970643,-0.3232988488812));
#38153=CARTESIAN_POINT('Ctrl Pts',(0.4301437799104,-1.187083031034,-0.3739991224572));
#38154=CARTESIAN_POINT('Ctrl Pts',(-0.4451069467436,-1.181553893589,-0.4246993960332));
#38155=CARTESIAN_POINT('Ctrl Pts',(-1.106459711439,-0.6082242194561,-0.4753996696092));
#38156=CARTESIAN_POINT('Ctrl Pts',(-1.236098759301,0.2573900785259,-0.5260999431852));
#38157=CARTESIAN_POINT('Ctrl Pts',(-0.7717255158527,0.9993145266845,-0.5768002167612));
#38158=CARTESIAN_POINT('Ctrl Pts',(0.06350356573547,1.261014310865,-0.6275004903372));
#38159=CARTESIAN_POINT('Ctrl Pts',(0.8682157503269,0.9167285344986,-0.6782007639132));
#38160=CARTESIAN_POINT('Ctrl Pts',(1.25570332166,0.1319051289551,-0.7289010374892));
#38161=CARTESIAN_POINT('Ctrl Pts',(1.039757549919,-0.7163058232812,-0.7796013110652));
#38162=CARTESIAN_POINT('Ctrl Pts',(0.3241520547935,-1.220293096121,-0.8303015846412));
#38163=CARTESIAN_POINT('Ctrl Pts',(-0.5472260298195,-1.137863553924,-0.8810018582172));
#38164=CARTESIAN_POINT('Ctrl Pts',(-1.155632418233,-0.5086290487165,-0.9317021317932));
#38165=CARTESIAN_POINT('Ctrl Pts',(-1.208694943071,0.365029216316,-0.9824024053692));
#38166=CARTESIAN_POINT('Ctrl Pts',(-0.6809141944598,1.063271205892,-1.033102678945));
#38167=CARTESIAN_POINT('Ctrl Pts',(0.1740826494533,1.250553887333,-1.083802952521));
#38168=CARTESIAN_POINT('Ctrl Pts',(0.9454233405756,0.8368778135224,-1.134503226097));
#38169=CARTESIAN_POINT('Ctrl Pts',(1.262437097122,0.02103667643451,-1.185203499673));
#38170=CARTESIAN_POINT('Ctrl Pts',(0.9727811924131,-0.8049136348134,-1.235903773249));
#38171=CARTESIAN_POINT('Ctrl Pts',(0.2156527249721,-1.244059744342,-1.286604046825));
#38172=CARTESIAN_POINT('Ctrl Pts',(-0.6451137599409,-1.085366676723,-1.337304320401));
#38173=CARTESIAN_POINT('Ctrl Pts',(-1.195848710366,-0.4051007221447,-1.388004593977));
#38174=CARTESIAN_POINT('Ctrl Pts',(-1.17198643604,0.4698547829221,-1.438704867553));
#38175=CARTESIAN_POINT('Ctrl Pts',(-0.5846498349379,1.118957149958,-1.489405141129));
#38176=CARTESIAN_POINT('Ctrl Pts',(-0.006463631599642,1.193367977664,-1.523205323513));
#38177=CARTESIAN_POINT('Ctrl Pts',(0.2606232035759,1.13186877553,-1.540105414705));
#38178=CARTESIAN_POINT('Ctrl Pts',(0.533586455706,-1.146361601056,0.02285160709841));
#38179=CARTESIAN_POINT('Ctrl Pts',(0.2630797515613,-1.272271883969,0.005951515906407));
#38180=CARTESIAN_POINT('Ctrl Pts',(-0.3694600846542,-1.323829144095,-0.02784866647759));
#38181=CARTESIAN_POINT('Ctrl Pts',(-1.141750418355,-0.7654711718991,-0.0785489400536));
#38182=CARTESIAN_POINT('Ctrl Pts',(-1.365092990625,0.1608650665466,-0.1292492136296));
#38183=CARTESIAN_POINT('Ctrl Pts',(-0.932508241689,1.009862650679,-0.1799494872056));
#38184=CARTESIAN_POINT('Ctrl Pts',(-0.05178312053545,1.373575815405,-0.2306497607816));
#38185=CARTESIAN_POINT('Ctrl Pts',(0.8538213005404,1.0772090683,-0.2813500343576));
#38186=CARTESIAN_POINT('Ctrl Pts',(1.349119837117,0.2631857779009,-0.3320503079336));
#38187=CARTESIAN_POINT('Ctrl Pts',(1.196092964055,-0.67731268624,-0.3827505815096));
#38188=CARTESIAN_POINT('Ctrl Pts',(0.4682788496866,-1.292325734365,-0.4334508550856));
#38189=CARTESIAN_POINT('Ctrl Pts',(-0.4845685994856,-1.286306402589,-0.4841511286616));
#38190=CARTESIAN_POINT('Ctrl Pts',(-1.204554628234,-0.6621472892105,-0.5348514022376));
#38191=CARTESIAN_POINT('Ctrl Pts',(-1.345687028708,0.2802093986293,-0.5855516758136));
#38192=CARTESIAN_POINT('Ctrl Pts',(-0.84014404884,1.087910319495,-0.6362519493896));
#38193=CARTESIAN_POINT('Ctrl Pts',(0.0691335737083,1.372811507476,-0.6869522229656));
#38194=CARTESIAN_POINT('Ctrl Pts',(0.9451887760124,0.9980025369641,-0.7376524965416));
#38195=CARTESIAN_POINT('Ctrl Pts',(1.367029664214,0.1435993845308,-0.7883527701176));
#38196=CARTESIAN_POINT('Ctrl Pts',(1.131938882228,-0.7798110367185,-0.8390530436936));
#38197=CARTESIAN_POINT('Ctrl Pts',(0.3528902623533,-1.32848008973,-0.8897533172696));
#38198=CARTESIAN_POINT('Ctrl Pts',(-0.5957412096389,-1.238742627507,-0.9404535908456));
#38199=CARTESIAN_POINT('Ctrl Pts',(-1.258086818281,-0.5537223527904,-0.9911538644216));
#38200=CARTESIAN_POINT('Ctrl Pts',(-1.315853684276,0.3973914525837,-1.041854137998));
#38201=CARTESIAN_POINT('Ctrl Pts',(-0.7412817076731,1.157537178158,-1.092554411574));
#38202=CARTESIAN_POINT('Ctrl Pts',(0.1895162190963,1.36142369873,-1.14325468515));
#38203=CARTESIAN_POINT('Ctrl Pts',(1.029241325967,0.9110725253918,-1.193954958726));
#38204=CARTESIAN_POINT('Ctrl Pts',(1.374360433074,0.0229017158961,-1.244655232302));
#38205=CARTESIAN_POINT('Ctrl Pts',(1.059024630961,-0.8762745124107,-1.295355505878));
#38206=CARTESIAN_POINT('Ctrl Pts',(0.2347717546974,-1.354353807332,-1.346055779454));
#38207=CARTESIAN_POINT('Ctrl Pts',(-0.7023073296214,-1.181591557525,-1.39675605303));
#38208=CARTESIAN_POINT('Ctrl Pts',(-1.301868548712,-0.4410155604543,-1.447456326606));
#38209=CARTESIAN_POINT('Ctrl Pts',(-1.275890727122,0.5115104937989,-1.498156600182));
#38210=CARTESIAN_POINT('Ctrl Pts',(-0.6364828807503,1.218160046718,-1.548856873758));
#38211=CARTESIAN_POINT('Ctrl Pts',(-0.007036674971584,1.299167882771,-1.582657056142));
#38212=CARTESIAN_POINT('Ctrl Pts',(0.2837291614389,1.232216372655,-1.599557147334));
#38213=CARTESIAN_POINT('',(-6.27395596736609E-7,1.24997530203264,-0.225010645721405));
#38214=CARTESIAN_POINT('Ctrl Pts',(-0.259605225442742,1.2221096527782,-1.11018313383523));
#38215=CARTESIAN_POINT('Ctrl Pts',(-0.332793343799699,1.20658875041188,
-1.10592121754818));
#38216=CARTESIAN_POINT('Ctrl Pts',(-0.404627231171491,1.18460760228849,
-1.10163375818886));
#38217=CARTESIAN_POINT('Ctrl Pts',(-0.540907581423731,1.12907020932194,
-1.09310261960631));
#38218=CARTESIAN_POINT('Ctrl Pts',(-0.605051057074797,1.09610920194188,
-1.08886731166991));
#38219=CARTESIAN_POINT('Ctrl Pts',(-0.707773733444926,1.03133277602085,
-1.08183127853167));
#38220=CARTESIAN_POINT('Ctrl Pts',(-0.747876095420288,1.00251248508937,
-1.07901758676475));
#38221=CARTESIAN_POINT('Ctrl Pts',(-0.902490851934647,0.876949291775734,
-1.06774084144926));
#38222=CARTESIAN_POINT('Ctrl Pts',(-1.0138428358634,0.751833092841553,-1.0586505729085));
#38223=CARTESIAN_POINT('Ctrl Pts',(-1.15509080823289,0.491421217862387,
-1.0413068606991));
#38224=CARTESIAN_POINT('Ctrl Pts',(-1.19657771566736,0.379998490744453,
-1.03436574906601));
#38225=CARTESIAN_POINT('Ctrl Pts',(-1.2388812299059,0.183548531329244,-1.02304603182886));
#38226=CARTESIAN_POINT('Ctrl Pts',(-1.24822862158008,0.101353967219403,
-1.01848558150274));
#38227=CARTESIAN_POINT('Ctrl Pts',(-1.25064592547273,-0.0636385446959788,
-1.00914796937442));
#38228=CARTESIAN_POINT('Ctrl Pts',(-1.24360156558463,-0.146207101339098,
-1.00435180784633));
#38229=CARTESIAN_POINT('Ctrl Pts',(-1.21423532252292,-0.305473346970245,
-0.994882212107024));
#38230=CARTESIAN_POINT('Ctrl Pts',(-1.19240456889098,-0.382419882142272,
-0.990208810300233));
#38231=CARTESIAN_POINT('Ctrl Pts',(-1.12389530484134,-0.557706864720993,
-0.979389360044569));
#38232=CARTESIAN_POINT('Ctrl Pts',(-1.07140580908498,-0.652703390758001,
-0.973454062146158));
#38233=CARTESIAN_POINT('Ctrl Pts',(-0.957706313327495,-0.806805752769416,
-0.962575907373815));
#38234=CARTESIAN_POINT('Ctrl Pts',(-0.901724979600007,-0.868706008625303,
-0.95778528251258));
#38235=CARTESIAN_POINT('Ctrl Pts',(-0.760433678514357,-0.997215776308453,
-0.946724551610701));
#38236=CARTESIAN_POINT('Ctrl Pts',(-0.629136492052712,-1.09917336210828,
-0.937280108523909));
#38237=CARTESIAN_POINT('Ctrl Pts',(-0.286239863661689,-1.22739413114836,
-0.916469035572465));
#38238=CARTESIAN_POINT('Ctrl Pts',(-0.120960966641227,-1.2541031443743,
-0.907128686921723));
#38239=CARTESIAN_POINT('Ctrl Pts',(0.208839532035743,-1.24344135072375,
-0.888124527877101));
#38240=CARTESIAN_POINT('Ctrl Pts',(0.369351146014912,-1.20548598183773,
-0.878658033949627));
#38241=CARTESIAN_POINT('Ctrl Pts',(0.653530517151995,-1.0748595082132,-0.86097736285615));
#38242=CARTESIAN_POINT('Ctrl Pts',(0.790494633015143,-0.983540006369001,
-0.851915963648905));
#38243=CARTESIAN_POINT('Ctrl Pts',(0.953029280869852,-0.81090557025396,
-0.838012247102954));
#38244=CARTESIAN_POINT('Ctrl Pts',(0.991988826150089,-0.762820428211738,
-0.834376907931348));
#38245=CARTESIAN_POINT('Ctrl Pts',(1.07322924803779,-0.645542409563646,
-0.826147306672509));
#38246=CARTESIAN_POINT('Ctrl Pts',(1.11272193143574,-0.574484813871174,
-0.821616299393835));
#38247=CARTESIAN_POINT('Ctrl Pts',(1.17942583426961,-0.421500002001213,
-0.812271789218584));
#38248=CARTESIAN_POINT('Ctrl Pts',(1.20574918191328,-0.339071245799685,
-0.80744115527922));
#38249=CARTESIAN_POINT('Ctrl Pts',(1.23707666683118,-0.188495172720685,
-0.798542895360767));
#38250=CARTESIAN_POINT('Ctrl Pts',(1.24548240634588,-0.121339319207742,
-0.794572714122722));
#38251=CARTESIAN_POINT('Ctrl Pts',(1.25116016900615,0.00698728876904618,
-0.787045887630086));
#38252=CARTESIAN_POINT('Ctrl Pts',(1.24941924339205,0.0681398408708604,
-0.783485541818798));
#38253=CARTESIAN_POINT('Ctrl Pts',(1.2339249163468,0.218447452511582,-0.774855578245345));
#38254=CARTESIAN_POINT('Ctrl Pts',(1.21484458608801,0.306985921576119,-0.76988232292773));
#38255=CARTESIAN_POINT('Ctrl Pts',(1.13817170855602,0.537816874620536,-0.756169063891392));
#38256=CARTESIAN_POINT('Ctrl Pts',(1.06292716185562,0.674062946336455,-0.74715663760518));
#38257=CARTESIAN_POINT('Ctrl Pts',(0.863239166447923,0.918638712550113,
-0.728857496300459));
#38258=CARTESIAN_POINT('Ctrl Pts',(0.737765941036426,1.02175471207368,-0.719966828231533));
#38259=CARTESIAN_POINT('Ctrl Pts',(0.450407462399465,1.17664995234507,-0.701312819538328));
#38260=CARTESIAN_POINT('Ctrl Pts',(0.290549704395172,1.22653947134232,-0.691803216516644));
#38261=CARTESIAN_POINT('Ctrl Pts',(-0.0690464104451976,1.26381173939837,
-0.670928898290121));
#38262=CARTESIAN_POINT('Ctrl Pts',(-0.232457553950564,1.23284703202773,
-0.661775424726093));
#38263=CARTESIAN_POINT('Ctrl Pts',(-0.422221745520559,1.17880981536598,
-0.650567281786364));
#38264=CARTESIAN_POINT('Ctrl Pts',(-0.49988825970878,1.14823635435013,-0.645820122340236));
#38265=CARTESIAN_POINT('Ctrl Pts',(-0.675688210706989,1.05778575460495,
-0.63433732422714));
#38266=CARTESIAN_POINT('Ctrl Pts',(-0.769326149939173,0.991764411544746,
-0.627632995995563));
#38267=CARTESIAN_POINT('Ctrl Pts',(-0.940227857022287,0.831585618564714,
-0.614362618801111));
#38268=CARTESIAN_POINT('Ctrl Pts',(-1.01560232478908,0.737510606305067,
-0.607753301954979));
#38269=CARTESIAN_POINT('Ctrl Pts',(-1.11731256009701,0.565318137788229,
-0.596307515497301));
#38270=CARTESIAN_POINT('Ctrl Pts',(-1.15146949806823,0.492073084034203,
-0.591572524153841));
#38271=CARTESIAN_POINT('Ctrl Pts',(-1.23762695617272,0.248876879143746,
-0.576429879567165));
#38272=CARTESIAN_POINT('Ctrl Pts',(-1.25549403921304,0.0854208148786327,
-0.567497360503563));
#38273=CARTESIAN_POINT('Ctrl Pts',(-1.2435576294284,-0.151614161959077,
-0.554097694180581));
#38274=CARTESIAN_POINT('Ctrl Pts',(-1.22928407832564,-0.2406361994489,-0.548885683063481));
#38275=CARTESIAN_POINT('Ctrl Pts',(-1.18465125529801,-0.405610547927827,
-0.53890480609632));
#38276=CARTESIAN_POINT('Ctrl Pts',(-1.15574468996294,-0.482337194960969,
-0.534126831413352));
#38277=CARTESIAN_POINT('Ctrl Pts',(-1.08203534383963,-0.631471820430162,
-0.524572690598339));
#38278=CARTESIAN_POINT('Ctrl Pts',(-1.03702148565761,-0.702882648383947,
-0.519898968031909));
#38279=CARTESIAN_POINT('Ctrl Pts',(-0.910841802069064,-0.863842420970694,
-0.508352193175204));
#38280=CARTESIAN_POINT('Ctrl Pts',(-0.822947338097478,-0.947547974950528,
-0.501423235127909));
#38281=CARTESIAN_POINT('Ctrl Pts',(-0.630595413860702,-1.08499069844033,
-0.487744504217735));
#38282=CARTESIAN_POINT('Ctrl Pts',(-0.483561323942755,-1.17152246765561,
-0.478109711456321));
#38283=CARTESIAN_POINT('Ctrl Pts',(-0.124038455487387,-1.25358912017759,
-0.457131876544059));
#38284=CARTESIAN_POINT('Ctrl Pts',(0.0401015968144676,-1.25900722545789,
-0.447984992876773));
#38285=CARTESIAN_POINT('Ctrl Pts',(0.278334007624253,-1.22110149435487,
-0.434047780606309));
#38286=CARTESIAN_POINT('Ctrl Pts',(0.355786009597055,-1.20096149810893,
-0.429370639175397));
#38287=CARTESIAN_POINT('Ctrl Pts',(0.509700848956409,-1.14427501326509,
-0.419895090107493));
#38288=CARTESIAN_POINT('Ctrl Pts',(0.585431982044724,-1.10717498072944,
-0.415154599429063));
#38289=CARTESIAN_POINT('Ctrl Pts',(0.726440296136035,-1.01980746202791,
-0.405808910950304));
#38290=CARTESIAN_POINT('Ctrl Pts',(0.79193847440835,-0.969854266302534,
-0.401199774458878));
#38291=CARTESIAN_POINT('Ctrl Pts',(0.926169591232099,-0.84503220543306,
-0.390708198653976));
#38292=CARTESIAN_POINT('Ctrl Pts',(0.99128315661927,-0.76773893124781,-0.384765925133727));
#38293=CARTESIAN_POINT('Ctrl Pts',(1.1056674942179,-0.592740847284177,-0.372559831060587));
#38294=CARTESIAN_POINT('Ctrl Pts',(1.15251793540906,-0.494962026616307,
-0.366525724523134));
#38295=CARTESIAN_POINT('Ctrl Pts',(1.211992125177,-0.314944289016718,-0.355916308375784));
#38296=CARTESIAN_POINT('Ctrl Pts',(1.23008311876091,-0.234572869544146,
-0.351298961060406));
#38297=CARTESIAN_POINT('Ctrl Pts',(1.25162567813202,-0.0594674105239562,
-0.341082907897881));
#38298=CARTESIAN_POINT('Ctrl Pts',(1.25262045616465,0.0352488940142594,
-0.335515074999312));
#38299=CARTESIAN_POINT('Ctrl Pts',(1.23180559406545,0.23879103312473,-0.323618943883807));
#38300=CARTESIAN_POINT('Ctrl Pts',(1.20612903123305,0.345765504090371,-0.317532801802942));
#38301=CARTESIAN_POINT('Ctrl Pts',(1.11630809624336,0.578614762255521,-0.303513296923535));
#38302=CARTESIAN_POINT('Ctrl Pts',(1.04407223873877,0.69991393392008,-0.295409808134786));
#38303=CARTESIAN_POINT('Ctrl Pts',(0.901474408285513,0.869328395269686,
-0.282544897417378));
#38304=CARTESIAN_POINT('Ctrl Pts',(0.842103580503381,0.927316454384216,
-0.277758230779022));
#38305=CARTESIAN_POINT('Ctrl Pts',(0.7128421979089,1.03016942444653,-0.268352130319226));
#38306=CARTESIAN_POINT('Ctrl Pts',(0.643326063905394,1.07469652485503,-0.263721551697975));
#38307=CARTESIAN_POINT('Ctrl Pts',(0.481942935922786,1.15691777598009,-0.253411516358004));
#38308=CARTESIAN_POINT('Ctrl Pts',(0.388650741524565,1.19137466480566,-0.247759035619074));
#38309=CARTESIAN_POINT('Ctrl Pts',(0.197097186680785,1.23781549769892,-0.236421653898855));
#38310=CARTESIAN_POINT('Ctrl Pts',(0.098659664897847,1.24992163553485,-0.230723881923306));
#38311=CARTESIAN_POINT('Ctrl Pts',(-6.27396302407881E-7,1.24997530203264,
-0.225010645721364));
#38312=CARTESIAN_POINT('',(0.000261740803262159,-1.24944061383241,-1.10756895875068E-17));
#38313=CARTESIAN_POINT('Ctrl Pts',(0.000250820037674612,-1.24944062023903,
-8.31504902660109E-5));
#38314=CARTESIAN_POINT('Ctrl Pts',(-0.133757168394608,-1.24960261218778,
-0.00770034556823749));
#38315=CARTESIAN_POINT('Ctrl Pts',(-0.294458227534603,-1.22918577895942,
-0.0167176425491502));
#38316=CARTESIAN_POINT('Ctrl Pts',(-0.617257941985387,-1.09834322766392,
-0.0368409886524448));
#38317=CARTESIAN_POINT('Ctrl Pts',(-0.756097898427124,-1.00766451211646,
-0.0462884129246149));
#38318=CARTESIAN_POINT('Ctrl Pts',(-0.931307333688564,-0.837492637847146,
-0.0601764677254039));
#38319=CARTESIAN_POINT('Ctrl Pts',(-0.983901742932066,-0.775245228369939,
-0.0647038041558236));
#38320=CARTESIAN_POINT('Ctrl Pts',(-1.07689915920209,-0.639776624696279,
-0.0740181627002627));
#38321=CARTESIAN_POINT('Ctrl Pts',(-1.11671817330185,-0.566878286914523,
-0.0788188276728031));
#38322=CARTESIAN_POINT('Ctrl Pts',(-1.18393443259893,-0.408967913919388,
-0.0888250499830544));
#38323=CARTESIAN_POINT('Ctrl Pts',(-1.21017638688533,-0.323286163379387,
-0.0940389468331596));
#38324=CARTESIAN_POINT('Ctrl Pts',(-1.24216459446644,-0.157877480752195,
-0.103691420051535));
#38325=CARTESIAN_POINT('Ctrl Pts',(-1.24971357675157,-0.0790974806829304,
-0.108085773361406));
#38326=CARTESIAN_POINT('Ctrl Pts',(-1.24988593361916,0.180418214864625,
-0.122611971346616));
#38327=CARTESIAN_POINT('Ctrl Pts',(-1.21089420993376,0.339040334133182,
-0.132125186565245));
#38328=CARTESIAN_POINT('Ctrl Pts',(-1.1187141109918,0.566425990040005,-0.14640077042418));
#38329=CARTESIAN_POINT('Ctrl Pts',(-1.06707412558697,0.658374409984222,
-0.152274352254586));
#38330=CARTESIAN_POINT('Ctrl Pts',(-0.956624024988722,0.808168419043991,
-0.162709266732783));
#38331=CARTESIAN_POINT('Ctrl Pts',(-0.901806032273976,0.869170379558039,
-0.16729669577124));
#38332=CARTESIAN_POINT('Ctrl Pts',(-0.791635807660082,0.969568013609325,
-0.175918025352255));
#38333=CARTESIAN_POINT('Ctrl Pts',(-0.738127885519106,1.01083833790894,
-0.179895394613272));
#38334=CARTESIAN_POINT('Ctrl Pts',(-0.580657072298911,1.11300758383781,
-0.190853149459495));
#38335=CARTESIAN_POINT('Ctrl Pts',(-0.470261305987306,1.16362448208699,
-0.197671271948075));
#38336=CARTESIAN_POINT('Ctrl Pts',(-0.240422179831552,1.23203934577827,
-0.21123374577893));
#38337=CARTESIAN_POINT('Ctrl Pts',(-0.120522818343935,1.25004086036163,
-0.218031427147732));
#38338=CARTESIAN_POINT('Ctrl Pts',(-6.27395597339278E-7,1.24997530203264,
-0.225010645721405));
#38339=CARTESIAN_POINT('',(-0.750030728394555,0.614591155635446,2.91990672313832E-5));
#38340=CARTESIAN_POINT('Ctrl Pts',(-0.750067840413312,0.61462509807075,
1.40946282423116E-17));
#38341=CARTESIAN_POINT('Ctrl Pts',(-0.809882553799936,0.557747719474187,
1.47833675193833E-17));
#38342=CARTESIAN_POINT('Ctrl Pts',(-0.862349497861938,0.493132905553222,
-4.34146451643364E-14));
#38343=CARTESIAN_POINT('Ctrl Pts',(-0.951569996446674,0.351090626404901,
-4.34169746916308E-14));
#38344=CARTESIAN_POINT('Ctrl Pts',(-0.987840882420652,0.27321621504591,
-4.32888744424384E-14));
#38345=CARTESIAN_POINT('Ctrl Pts',(-1.06248896738419,0.0396486927506802,
-4.32921841402061E-14));
#38346=CARTESIAN_POINT('Ctrl Pts',(-1.06751788595683,-0.101067592918028,
-4.36369690381966E-14));
#38347=CARTESIAN_POINT('Ctrl Pts',(-1.04580751638871,-0.351127201170586,
-4.36369690381966E-14));
#38348=CARTESIAN_POINT('Ctrl Pts',(-1.0082451256689,-0.485854779973621,
-4.39388442066686E-14));
#38349=CARTESIAN_POINT('Ctrl Pts',(-0.87764068444681,-0.7489867036794,-4.39424836500747E-14));
#38350=CARTESIAN_POINT('Ctrl Pts',(-0.783955290032865,-0.861345679857431,
-4.37323788293753E-14));
#38351=CARTESIAN_POINT('Ctrl Pts',(-0.59508582408829,-1.03154986337642,
-4.37323788293753E-14));
#38352=CARTESIAN_POINT('Ctrl Pts',(-0.488478947016535,-1.10097347077607,
-4.37150315946155E-14));
#38353=CARTESIAN_POINT('Ctrl Pts',(-0.256010239028481,-1.20416167455751,
-4.37150315946155E-14));
#38354=CARTESIAN_POINT('Ctrl Pts',(-0.131274571541265,-1.23651444295296,
-9.87156134091518E-19));
#38355=CARTESIAN_POINT('Ctrl Pts',(0.000261567582557562,-1.24929773378779,
-1.551537897789E-18));
#38356=CARTESIAN_POINT('Ctrl Pts',(-0.749485555563958,0.615178325934084,
-1.00645712846747E-9));
#38357=CARTESIAN_POINT('Ctrl Pts',(-0.691520344892466,0.685982827107283,
-0.00665992653678659));
#38358=CARTESIAN_POINT('Ctrl Pts',(-0.626014663918608,0.746342019032374,
-0.0133903488232786));
#38359=CARTESIAN_POINT('Ctrl Pts',(-0.48111095763836,0.846675629347526,
-0.0266157197187053));
#38360=CARTESIAN_POINT('Ctrl Pts',(-0.402197526342482,0.886528754234619,
-0.0330223634080707));
#38361=CARTESIAN_POINT('Ctrl Pts',(-0.238934813994007,0.943471759217515,
-0.0456276817308198));
#38362=CARTESIAN_POINT('Ctrl Pts',(-0.115826409566955,0.975260036400719,
-0.0547106245734519));
#38363=CARTESIAN_POINT('Ctrl Pts',(0.164263817962017,0.964276610736639,
-0.0756311165135602));
#38364=CARTESIAN_POINT('Ctrl Pts',(0.290738210007054,0.93356407375508,-0.0850937529442948));
#38365=CARTESIAN_POINT('Ctrl Pts',(0.471484943071061,0.85048861220488,-0.0997098803749702));
#38366=CARTESIAN_POINT('Ctrl Pts',(0.553331236734125,0.804677385467775,
-0.106422351683403));
#38367=CARTESIAN_POINT('Ctrl Pts',(0.685919407220429,0.688542270735864,
-0.119427545256577));
#38368=CARTESIAN_POINT('Ctrl Pts',(0.730011830464401,0.641340091837972,
-0.124237753090772));
#38369=CARTESIAN_POINT('Ctrl Pts',(0.837073888756735,0.501697000330135,
-0.137407244034439));
#38370=CARTESIAN_POINT('Ctrl Pts',(0.890067026179102,0.401433006390183,
-0.145762637896906));
#38371=CARTESIAN_POINT('Ctrl Pts',(0.937995412326277,0.251339217130985,
-0.157129989608011));
#38372=CARTESIAN_POINT('Ctrl Pts',(0.948722183341347,0.206675013450165,
-0.160392202885067));
#38373=CARTESIAN_POINT('Ctrl Pts',(0.966841915727626,0.0978769514002914,
-0.16847170289435));
#38374=CARTESIAN_POINT('Ctrl Pts',(0.971099109898709,0.0332044837877513,
-0.173336332219429));
#38375=CARTESIAN_POINT('Ctrl Pts',(0.967109275650522,-0.0922210214390128,
-0.182824410034968));
#38376=CARTESIAN_POINT('Ctrl Pts',(0.959517392720682,-0.153054110414589,
-0.187448619923345));
#38377=CARTESIAN_POINT('Ctrl Pts',(0.93214355099431,-0.276126422630988,
-0.196804854482268));
#38378=CARTESIAN_POINT('Ctrl Pts',(0.911745488645913,-0.337497518214735,
-0.201414941440259));
#38379=CARTESIAN_POINT('Ctrl Pts',(0.871687644696651,-0.426322591305666,
-0.208342672883873));
#38380=CARTESIAN_POINT('Ctrl Pts',(0.856929712329002,-0.455088174577703,
-0.210646074157641));
#38381=CARTESIAN_POINT('Ctrl Pts',(0.79817844630675,-0.55688844568411,-0.219226576125532));
#38382=CARTESIAN_POINT('Ctrl Pts',(0.745902330282399,-0.625206381972658,
-0.225805894744982));
#38383=CARTESIAN_POINT('Ctrl Pts',(0.65741174802194,-0.714092647241932,
-0.235350413404771));
#38384=CARTESIAN_POINT('Ctrl Pts',(0.627290301908243,-0.740832051278823,
-0.238389348669223));
#38385=CARTESIAN_POINT('Ctrl Pts',(0.558112227078551,-0.794812864846272,
-0.244885578166819));
#38386=CARTESIAN_POINT('Ctrl Pts',(0.518730216599021,-0.820992168547267,
-0.248261446274541));
#38387=CARTESIAN_POINT('Ctrl Pts',(0.442762049537832,-0.863751369927401,
-0.254433632373426));
#38388=CARTESIAN_POINT('Ctrl Pts',(0.406828890414051,-0.881133535967991,
-0.257239594387939));
#38389=CARTESIAN_POINT('Ctrl Pts',(0.337922691941123,-0.909442434782747,
-0.262605528275797));
#38390=CARTESIAN_POINT('Ctrl Pts',(0.305172653215591,-0.920914951539425,
-0.265161727418624));
#38391=CARTESIAN_POINT('Ctrl Pts',(0.208833043339074,-0.949078965083362,
-0.272720576179139));
#38392=CARTESIAN_POINT('Ctrl Pts',(0.143883729565482,-0.961233950332467,
-0.277833572029439));
#38393=CARTESIAN_POINT('Ctrl Pts',(0.0474934194474711,-0.969260940555831,
-0.285200154333576));
#38394=CARTESIAN_POINT('Ctrl Pts',(0.0164729529270842,-0.970342851269044,
-0.287537796531342));
#38395=CARTESIAN_POINT('Ctrl Pts',(-0.0653424655873088,-0.969146078894895,
-0.293578410026805));
#38396=CARTESIAN_POINT('Ctrl Pts',(-0.115961921977653,-0.964260454480337,
-0.297175859780403));
#38397=CARTESIAN_POINT('Ctrl Pts',(-0.219326353346127,-0.946082009489617,
-0.304602214808625));
#38398=CARTESIAN_POINT('Ctrl Pts',(-0.272046588834085,-0.932185270994219,
-0.308438650414657));
#38399=CARTESIAN_POINT('Ctrl Pts',(-0.388457131395581,-0.89101105826433,
-0.317508561425316));
#38400=CARTESIAN_POINT('Ctrl Pts',(-0.451243879102635,-0.861103249574949,
-0.322888442321947));
#38401=CARTESIAN_POINT('Ctrl Pts',(-0.536924828764396,-0.80837273831466,
-0.330617878612817));
#38402=CARTESIAN_POINT('Ctrl Pts',(-0.56292256459701,-0.790562087639446,
-0.333020777544854));
#38403=CARTESIAN_POINT('Ctrl Pts',(-0.655459430115703,-0.720081713362681,
-0.341718175884925));
#38404=CARTESIAN_POINT('Ctrl Pts',(-0.715775943532788,-0.659618235498914,
-0.347651089220564));
#38405=CARTESIAN_POINT('Ctrl Pts',(-0.78938680568236,-0.564076306987063,
-0.356257395470773));
#38406=CARTESIAN_POINT('Ctrl Pts',(-0.809829274119129,-0.534301363634571,
-0.358851432426246));
#38407=CARTESIAN_POINT('Ctrl Pts',(-0.857148042928083,-0.456585611588798,
-0.36554070102133));
#38408=CARTESIAN_POINT('Ctrl Pts',(-0.881793208184187,-0.407291199819409,
-0.369757859596612));
#38409=CARTESIAN_POINT('Ctrl Pts',(-0.915140502090481,-0.323377452942217,
-0.376703795174359));
#38410=CARTESIAN_POINT('Ctrl Pts',(-0.926413362915516,-0.289723950008743,
-0.379424856895539));
#38411=CARTESIAN_POINT('Ctrl Pts',(-0.949217677992506,-0.206078634024043,
-0.385930058678096));
#38412=CARTESIAN_POINT('Ctrl Pts',(-0.95864053732603,-0.155610638698208,
-0.389652058555324));
#38413=CARTESIAN_POINT('Ctrl Pts',(-0.969801649691148,-0.0507346562473078,
-0.397241599742637));
#38414=CARTESIAN_POINT('Ctrl Pts',(-0.971042800459035,0.00372980374851009,
-0.401105959396232));
#38415=CARTESIAN_POINT('Ctrl Pts',(-0.964781747558175,0.108989751510079,
-0.408723240957605));
#38416=CARTESIAN_POINT('Ctrl Pts',(-0.957774403787605,0.159842111318367,
-0.412474409006774));
#38417=CARTESIAN_POINT('Ctrl Pts',(-0.936386151240434,0.257402756862024,
-0.420023567590751));
#38418=CARTESIAN_POINT('Ctrl Pts',(-0.922354447477273,0.304279775572638,
-0.423797646603852));
#38419=CARTESIAN_POINT('Ctrl Pts',(-0.876119748295039,0.423693609136073,
-0.433462572432769));
#38420=CARTESIAN_POINT('Ctrl Pts',(-0.838231267092757,0.493856015239188,
-0.439224044298467));
#38421=CARTESIAN_POINT('Ctrl Pts',(-0.750851903981765,0.617560390565297,
-0.45018890711371));
#38422=CARTESIAN_POINT('Ctrl Pts',(-0.702623906629978,0.672054807996416,
-0.455405243399353));
#38423=CARTESIAN_POINT('Ctrl Pts',(-0.61200683040724,0.754041925758708,
-0.464422790609882));
#38424=CARTESIAN_POINT('Ctrl Pts',(-0.572430898513051,0.784671935337174,
-0.468192630225527));
#38425=CARTESIAN_POINT('Ctrl Pts',(-0.42528387712119,0.880845379749878,
-0.481445694398355));
#38426=CARTESIAN_POINT('Ctrl Pts',(-0.306094576674206,0.928412167081991,
-0.490662182298744));
#38427=CARTESIAN_POINT('Ctrl Pts',(-0.0580387459248825,0.976280702919913,
-0.509137535815805));
#38428=CARTESIAN_POINT('Ctrl Pts',(0.0673226445171873,0.976182205587661,
-0.5182088722675));
#38429=CARTESIAN_POINT('Ctrl Pts',(0.316083555754992,0.925111746696705,
-0.537108943756486));
#38430=CARTESIAN_POINT('Ctrl Pts',(0.434544326120844,0.875853962304653,
-0.546484461318104));
#38431=CARTESIAN_POINT('Ctrl Pts',(0.595730525638291,0.768532624929862,
-0.560666972570654));
#38432=CARTESIAN_POINT('Ctrl Pts',(0.647507647599943,0.725427789814852,
-0.565481489071531));
#38433=CARTESIAN_POINT('Ctrl Pts',(0.771623016477007,0.597458990055328,
-0.578599412540456));
#38434=CARTESIAN_POINT('Ctrl Pts',(0.834953406182651,0.504894658297685,
-0.587009219997219));
#38435=CARTESIAN_POINT('Ctrl Pts',(0.913148157900059,0.335498841908481,
-0.600918696671118));
#38436=CARTESIAN_POINT('Ctrl Pts',(0.937025197171096,0.262572447747291,
-0.606489962377818));
#38437=CARTESIAN_POINT('Ctrl Pts',(0.96211804984445,0.133913557420753,-0.615862958247662));
#38438=CARTESIAN_POINT('Ctrl Pts',(0.96793885815068,0.0799127885607206,
-0.619764510095875));
#38439=CARTESIAN_POINT('Ctrl Pts',(0.971270407808221,-0.0536288537972403,
-0.629707374053931));
#38440=CARTESIAN_POINT('Ctrl Pts',(0.963618744815539,-0.133350948918856,
-0.635805461263067));
#38441=CARTESIAN_POINT('Ctrl Pts',(0.934684022216928,-0.264515812148018,
-0.645935617275956));
#38442=CARTESIAN_POINT('Ctrl Pts',(0.918344524967836,-0.317102670203463,
-0.650023894001686));
#38443=CARTESIAN_POINT('Ctrl Pts',(0.88093418694075,-0.408375981736267,
-0.657144069358296));
#38444=CARTESIAN_POINT('Ctrl Pts',(0.861505526854446,-0.447688550533692,
-0.660221153294291));
#38445=CARTESIAN_POINT('Ctrl Pts',(0.818634181423107,-0.521432643019005,
-0.666290778824999));
#38446=CARTESIAN_POINT('Ctrl Pts',(0.795448704704568,-0.556002997167771,
-0.669292859829739));
#38447=CARTESIAN_POINT('Ctrl Pts',(0.726083876580491,-0.646524696234794,
-0.677783861362529));
#38448=CARTESIAN_POINT('Ctrl Pts',(0.675617822908381,-0.699242006906682,
-0.683396820829173));
#38449=CARTESIAN_POINT('Ctrl Pts',(0.583580615244474,-0.776112140596742,
-0.692525787113359));
#38450=CARTESIAN_POINT('Ctrl Pts',(0.544956949962885,-0.803848212499719,
-0.696095953845777));
#38451=CARTESIAN_POINT('Ctrl Pts',(0.477884260938761,-0.844685356806632,
-0.701817575538396));
#38452=CARTESIAN_POINT('Ctrl Pts',(0.450525645314577,-0.85952961025533,
-0.704033736041437));
#38453=CARTESIAN_POINT('Ctrl Pts',(0.363625550595281,-0.901361797886043,
-0.710867230111145));
#38454=CARTESIAN_POINT('Ctrl Pts',(0.301857203280628,-0.923702600477772,
-0.715444995721303));
#38455=CARTESIAN_POINT('Ctrl Pts',(0.188452732200309,-0.952442397040851,
-0.724108234250529));
#38456=CARTESIAN_POINT('Ctrl Pts',(0.137386209506803,-0.96120634008556,
-0.728077126307842));
#38457=CARTESIAN_POINT('Ctrl Pts',(0.029045336628559,-0.971079074828047,
-0.736444084393938));
#38458=CARTESIAN_POINT('Ctrl Pts',(-0.0283379223967618,-0.971271313100352,
-0.740841700768136));
#38459=CARTESIAN_POINT('Ctrl Pts',(-0.137706274659779,-0.961615230071308,
-0.748946462498991));
#38460=CARTESIAN_POINT('Ctrl Pts',(-0.189712132252472,-0.952572327642054,
-0.752680183344212));
#38461=CARTESIAN_POINT('Ctrl Pts',(-0.297558271626115,-0.92469155413691,
-0.760570659714922));
#38462=CARTESIAN_POINT('Ctrl Pts',(-0.353134000454666,-0.904834935521383,
-0.764729186214));
#38463=CARTESIAN_POINT('Ctrl Pts',(-0.433587763705638,-0.867731809970381,
-0.771275474762301));
#38464=CARTESIAN_POINT('Ctrl Pts',(-0.460115617634662,-0.854008763357978,
-0.773532975406683));
#38465=CARTESIAN_POINT('Ctrl Pts',(-0.538944921022525,-0.808557613284767,
-0.780492826456917));
#38466=CARTESIAN_POINT('Ctrl Pts',(-0.589072542125404,-0.773045633364942,
-0.785266151052505));
#38467=CARTESIAN_POINT('Ctrl Pts',(-0.670211461650972,-0.702760392407441,
-0.793324680399299));
#38468=CARTESIAN_POINT('Ctrl Pts',(-0.702805900693151,-0.66999869322811,
-0.796672630188785));
#38469=CARTESIAN_POINT('Ctrl Pts',(-0.78233279965786,-0.577811931065102,
-0.805404264469002));
#38470=CARTESIAN_POINT('Ctrl Pts',(-0.825087301881679,-0.514676999541364,
-0.810728582252462));
#38471=CARTESIAN_POINT('Ctrl Pts',(-0.880434048504769,-0.408558473588861,
-0.819489984580917));
#38472=CARTESIAN_POINT('Ctrl Pts',(-0.898163875161468,-0.368204861415813,
-0.822804768713365));
#38473=CARTESIAN_POINT('Ctrl Pts',(-0.930208860998752,-0.279316122077531,
-0.830043067073164));
#38474=CARTESIAN_POINT('Ctrl Pts',(-0.943651535328424,-0.230373629098725,
-0.833956404373398));
#38475=CARTESIAN_POINT('Ctrl Pts',(-0.966335841184824,-0.109950723894625,
-0.843124312315739));
#38476=CARTESIAN_POINT('Ctrl Pts',(-0.97157941071164,-0.0380282375235174,
-0.848283775586799));
#38477=CARTESIAN_POINT('Ctrl Pts',(-0.966088027504813,0.114896524809793,
-0.859281137041708));
#38478=CARTESIAN_POINT('Ctrl Pts',(-0.95310172230759,0.195876161046513,
-0.865129935021918));
#38479=CARTESIAN_POINT('Ctrl Pts',(-0.918435757121371,0.314593071809577,
-0.87441646900891));
#38480=CARTESIAN_POINT('Ctrl Pts',(-0.903903884112642,0.354459195987018,
-0.877670783324424));
#38481=CARTESIAN_POINT('Ctrl Pts',(-0.860546750461119,0.452274810527204,
-0.885775133373804));
#38482=CARTESIAN_POINT('Ctrl Pts',(-0.828253384759571,0.50859402221818,
-0.890546529256785));
#38483=CARTESIAN_POINT('Ctrl Pts',(-0.720433024176727,0.65990956703673,
-0.90412234912441));
#38484=CARTESIAN_POINT('Ctrl Pts',(-0.631664981090838,0.745716425089765,
-0.912829925791812));
#38485=CARTESIAN_POINT('Ctrl Pts',(-0.476618706517394,0.847317999288356,
-0.926673505026629));
#38486=CARTESIAN_POINT('Ctrl Pts',(-0.419945460265682,0.876638661709985,
-0.93145667890111));
#38487=CARTESIAN_POINT('Ctrl Pts',(-0.243307508699527,0.94696398470386,
-0.945583159110242));
#38488=CARTESIAN_POINT('Ctrl Pts',(-0.11654790194724,0.970817054884752,
-0.954851035349461));
#38489=CARTESIAN_POINT('Ctrl Pts',(0.0727293711116787,0.969303096643114,
-0.968730319005118));
#38490=CARTESIAN_POINT('Ctrl Pts',(0.134962790795066,0.962658818848594,
-0.973292180744191));
#38491=CARTESIAN_POINT('Ctrl Pts',(0.316775418871325,0.924637990171389,
-0.98705329882165));
#38492=CARTESIAN_POINT('Ctrl Pts',(0.432175375890316,0.876436011350086,
-0.996300528584387));
#38493=CARTESIAN_POINT('Ctrl Pts',(0.639110439441325,0.740299900579539,
-1.01459255276467));
#38494=CARTESIAN_POINT('Ctrl Pts',(0.727700888215557,0.653091805650583,
-1.0232355501562));
#38495=CARTESIAN_POINT('Ctrl Pts',(0.871881721970838,0.443330411650751,
-1.04224793536479));
#38496=CARTESIAN_POINT('Ctrl Pts',(0.924412601499112,0.321183448355106,
-1.05225574397271));
#38497=CARTESIAN_POINT('Ctrl Pts',(0.960404105110912,0.145014724677346,
-1.06526952055553));
#38498=CARTESIAN_POINT('Ctrl Pts',(0.966421868613754,0.095847093404394,
-1.06874606528881));
#38499=CARTESIAN_POINT('Ctrl Pts',(0.970729240872516,0.00187689603276803,
-1.0755116092022));
#38500=CARTESIAN_POINT('Ctrl Pts',(0.969681721175105,-0.042983065569024,
-1.07881945506364));
#38501=CARTESIAN_POINT('Ctrl Pts',(0.959834904353882,-0.150613410626042,
-1.08694389716873));
#38502=CARTESIAN_POINT('Ctrl Pts',(0.947993986329022,-0.213147916679648,
-1.09180528355103));
#38503=CARTESIAN_POINT('Ctrl Pts',(0.91650765643918,-0.320938744543342,
-1.10030805612764));
#38504=CARTESIAN_POINT('Ctrl Pts',(0.899234303655736,-0.366914797765025,
-1.10397668870833));
#38505=CARTESIAN_POINT('Ctrl Pts',(0.863181522759483,-0.444015255370893,
-1.1101697508737));
#38506=CARTESIAN_POINT('Ctrl Pts',(0.846026395087111,-0.475758637002667,
-1.1127263083037));
#38507=CARTESIAN_POINT('Ctrl Pts',(0.798792801753869,-0.552547557874234,
-1.11910921362408));
#38508=CARTESIAN_POINT('Ctrl Pts',(0.766517069542252,-0.596285269892296,
-1.12294200679953));
#38509=CARTESIAN_POINT('Ctrl Pts',(0.709453468724753,-0.661624638763062,
-1.12936425172609));
#38510=CARTESIAN_POINT('Ctrl Pts',(0.686807319865723,-0.685101926287355,
-1.13182699222252));
#38511=CARTESIAN_POINT('Ctrl Pts',(0.61169482423289,-0.755632958071713,
-1.13968210824357));
#38512=CARTESIAN_POINT('Ctrl Pts',(0.555141377307848,-0.79838321724767,
-1.14515031283205));
#38513=CARTESIAN_POINT('Ctrl Pts',(0.460693609271441,-0.854546637786924,
-1.15335827155446));
#38514=CARTESIAN_POINT('Ctrl Pts',(0.425801821844024,-0.872433493271216,
-1.15620343196439));
#38515=CARTESIAN_POINT('Ctrl Pts',(0.332388309604862,-0.913226856010398,
-1.16347685538568));
#38516=CARTESIAN_POINT('Ctrl Pts',(0.272558685364116,-0.93264051043169,
-1.16783965424534));
#38517=CARTESIAN_POINT('Ctrl Pts',(0.178496355530374,-0.953565561825706,
-1.17481380345513));
#38518=CARTESIAN_POINT('Ctrl Pts',(0.145167214285422,-0.959204683225914,
-1.17731585786918));
#38519=CARTESIAN_POINT('Ctrl Pts',(0.0692468388711174,-0.968078113397592,
-1.1830999057879));
#38520=CARTESIAN_POINT('Ctrl Pts',(0.0265243779043479,-0.970282399643622,
-1.18639965660027));
#38521=CARTESIAN_POINT('Ctrl Pts',(-0.0595890125701362,-0.969042878863386,
-1.19302385637117));
#38522=CARTESIAN_POINT('Ctrl Pts',(-0.102993939759864,-0.96549738632567,
-1.19634798154522));
#38523=CARTESIAN_POINT('Ctrl Pts',(-0.20107109129166,-0.950564436110202,
-1.20370419682778));
#38524=CARTESIAN_POINT('Ctrl Pts',(-0.255406864398631,-0.937259321727124,
-1.20766967676982));
#38525=CARTESIAN_POINT('Ctrl Pts',(-0.368152213245982,-0.899195722399789,
-1.21611327792907));
#38526=CARTESIAN_POINT('Ctrl Pts',(-0.426127408467094,-0.873136977883424,
-1.22059321122393));
#38527=CARTESIAN_POINT('Ctrl Pts',(-0.522461577342956,-0.818207220712546,
-1.22881100441419));
#38528=CARTESIAN_POINT('Ctrl Pts',(-0.562146172966108,-0.791604600021575,
-1.2324777898972));
#38529=CARTESIAN_POINT('Ctrl Pts',(-0.641434912696933,-0.729513125602168,
-1.24023231918795));
#38530=CARTESIAN_POINT('Ctrl Pts',(-0.680474960080581,-0.693387406624301,
-1.24429626135695));
#38531=CARTESIAN_POINT('Ctrl Pts',(-0.743404971363553,-0.624247255645805,
-1.25119387979881));
#38532=CARTESIAN_POINT('Ctrl Pts',(-0.768483395909982,-0.592929417872231,
-1.25408423581254));
#38533=CARTESIAN_POINT('Ctrl Pts',(-0.841810780459252,-0.488842643262975,
-1.26320858723048));
#38534=CARTESIAN_POINT('Ctrl Pts',(-0.882534380138505,-0.410710524809581,
-1.26937889325325));
#38535=CARTESIAN_POINT('Ctrl Pts',(-0.924615817339235,-0.294621768222479,
-1.27859240981985));
#38536=CARTESIAN_POINT('Ctrl Pts',(-0.935069062702998,-0.259889965944934,
-1.28136301627869));
#38537=CARTESIAN_POINT('Ctrl Pts',(-0.957698601773173,-0.165675486443003,
-1.2887871053272));
#38538=CARTESIAN_POINT('Ctrl Pts',(-0.966086884769573,-0.105988567500736,
-1.29333243383832));
#38539=CARTESIAN_POINT('Ctrl Pts',(-0.971698370569345,0.0191806258173882,
-1.30254126644064));
#38540=CARTESIAN_POINT('Ctrl Pts',(-0.968077282694246,0.0841725751854099,
-1.30719622877896));
#38541=CARTESIAN_POINT('Ctrl Pts',(-0.948242901745456,0.212255169708748,
-1.31655232412133));
#38542=CARTESIAN_POINT('Ctrl Pts',(-0.932004641003878,0.275387666342886,
-1.321259447385));
#38543=CARTESIAN_POINT('Ctrl Pts',(-0.892092351256462,0.384106329597992,
-1.32990535923517));
#38544=CARTESIAN_POINT('Ctrl Pts',(-0.870726395993944,0.430625752678655,
-1.33382068132123));
#38545=CARTESIAN_POINT('Ctrl Pts',(-0.806284444068375,0.544987834505778,
-1.34369202911898));
#38546=CARTESIAN_POINT('Ctrl Pts',(-0.758204956847398,0.609636286270502,
-1.34956506288098));
#38547=CARTESIAN_POINT('Ctrl Pts',(-0.636948315443397,0.737144060549658,
-1.3624084876591));
#38548=CARTESIAN_POINT('Ctrl Pts',(-0.560587252664674,0.797127369094058,
-1.36937786797394));
#38549=CARTESIAN_POINT('Ctrl Pts',(-0.370613295808071,0.904890897651286,
-1.38555811559755));
#38550=CARTESIAN_POINT('Ctrl Pts',(-0.272904921177973,0.933380625736226,
-1.39307688337039));
#38551=CARTESIAN_POINT('Ctrl Pts',(-0.201493905888848,0.948457169294521,
-1.39848693227111));
#38552=CARTESIAN_POINT('Ctrl Pts',(0.6384670947158,1.091429885542,0.1954399664911));
#38553=CARTESIAN_POINT('Ctrl Pts',(0.8484087081986,0.9686177710893,0.1816635794825));
#38554=CARTESIAN_POINT('Ctrl Pts',(1.194967633217,0.5987185795046,0.1541108054654));
#38555=CARTESIAN_POINT('Ctrl Pts',(1.328153666836,-0.150240885146,0.1127816444398));
#38556=CARTESIAN_POINT('Ctrl Pts',(1.031103739632,-0.8504871930036,0.07145248341419));
#38557=CARTESIAN_POINT('Ctrl Pts',(0.4001420220925,-1.275306320712,0.03012332238856));
#38558=CARTESIAN_POINT('Ctrl Pts',(-0.3604180561742,-1.287095826843,-0.01120583863706));
#38559=CARTESIAN_POINT('Ctrl Pts',(-1.004249922984,-0.8820425745732,-0.05253499966269));
#38560=CARTESIAN_POINT('Ctrl Pts',(-1.322842019319,-0.1913273198153,-0.09386416068832));
#38561=CARTESIAN_POINT('Ctrl Pts',(-1.213013257137,0.5613518632076,-0.1351933217139));
#38562=CARTESIAN_POINT('Ctrl Pts',(-0.710333370038,1.13222948353,-0.1765224827396));
#38563=CARTESIAN_POINT('Ctrl Pts',(0.02239783615318,1.33641888331,-0.2178516437652));
#38564=CARTESIAN_POINT('Ctrl Pts',(0.7478751900674,1.107790501614,-0.2591808047908));
#38565=CARTESIAN_POINT('Ctrl Pts',(1.231142796103,0.5203888075962,-0.3005099658165));
#38566=CARTESIAN_POINT('Ctrl Pts',(1.315687739353,-0.2355480161242,-0.3418391268421));
#38567=CARTESIAN_POINT('Ctrl Pts',(0.9741289680772,-0.9151993493049,-0.3831682878677));
#38568=CARTESIAN_POINT('Ctrl Pts',(0.3170850255305,-1.298450685237,-0.4244974488933));
#38569=CARTESIAN_POINT('Ctrl Pts',(-0.442651298475,-1.26118076554,-0.465826609919));
#38570=CARTESIAN_POINT('Ctrl Pts',(-1.059028862723,-0.815459970401,-0.5071557709446));
#38571=CARTESIAN_POINT('Ctrl Pts',(-1.332425247817,-0.1056411586267,-0.5484849319702));
#38572=CARTESIAN_POINT('Ctrl Pts',(-1.174297244163,0.6383910069347,-0.5898140929959));
#38573=CARTESIAN_POINT('Ctrl Pts',(-0.6358567980407,1.175671394503,-0.6311432540215));
#38574=CARTESIAN_POINT('Ctrl Pts',(0.1085146876066,1.332194301879,-0.6724724150471));
#38575=CARTESIAN_POINT('Ctrl Pts',(0.8177421864919,1.057267615679,-0.7138015760727));
#38576=CARTESIAN_POINT('Ctrl Pts',(1.262132544314,0.4399301541693,-0.7551307370984));
#38577=CARTESIAN_POINT('Ctrl Pts',(1.297763769147,-0.3198847852044,-0.796459898124));
#38578=CARTESIAN_POINT('Ctrl Pts',(0.9130962459419,-0.9761006080475,-0.8377890591496));
#38579=CARTESIAN_POINT('Ctrl Pts',(0.232709694298,-1.316192694613,-0.8791182201752));
#38580=CARTESIAN_POINT('Ctrl Pts',(-0.5230425568228,-1.23001761225,-0.9204473812009));
#38581=CARTESIAN_POINT('Ctrl Pts',(-1.109402319153,-0.7454839661251,-0.9617765422265));
#38582=CARTESIAN_POINT('Ctrl Pts',(-1.336458943337,-0.01951615025343,-1.003105703252));
#38583=CARTESIAN_POINT('Ctrl Pts',(-1.130713983139,0.7127765250298,-1.044434864278));
#38584=CARTESIAN_POINT('Ctrl Pts',(-0.5586627502186,1.214210654458,-1.085764025303));
#38585=CARTESIAN_POINT('Ctrl Pts',(-0.05694569140623,1.286380546669,-1.11331679932));
#38586=CARTESIAN_POINT('Ctrl Pts',(0.1836986798923,1.251045251418,-1.127093186329));
#38587=CARTESIAN_POINT('Ctrl Pts',(0.5864724611271,1.002547470996,0.1359882338627));
#38588=CARTESIAN_POINT('Ctrl Pts',(0.779317128881,0.889736766082,0.1222118468541));
#38589=CARTESIAN_POINT('Ctrl Pts',(1.097653449364,0.5499609326004,0.09465907283704));
#38590=CARTESIAN_POINT('Ctrl Pts',(1.219993256021,-0.1380057678818,0.05332991181142));
#38591=CARTESIAN_POINT('Ctrl Pts',(0.9471340854743,-0.7812263488064,0.01200075078579));
#38592=CARTESIAN_POINT('Ctrl Pts',(0.3675557886055,-1.171449621741,-0.02932841023984));
#38593=CARTESIAN_POINT('Ctrl Pts',(-0.3310668101591,-1.182279029761,-0.07065757126547));
#38594=CARTESIAN_POINT('Ctrl Pts',(-0.9224671542099,-0.8102119652057,-0.1119867322911));
#38595=CARTESIAN_POINT('Ctrl Pts',(-1.215114171385,-0.1757462601622,-0.1533158933167));
#38596=CARTESIAN_POINT('Ctrl Pts',(-1.114229497778,0.5156372372177,-0.1946450543423));
#38597=CARTESIAN_POINT('Ctrl Pts',(-0.6524861863591,1.040024485619,-0.235974215368));
#38598=CARTESIAN_POINT('Ctrl Pts',(0.02057383097953,1.227585380795,-0.2773033763936));
#38599=CARTESIAN_POINT('Ctrl Pts',(0.6869707256095,1.017575732989,-0.3186325374192));
#38600=CARTESIAN_POINT('Ctrl Pts',(1.130882627476,0.4780100764156,-0.3599616984449));
#38601=CARTESIAN_POINT('Ctrl Pts',(1.20854251215,-0.2163657702539,-0.4012908594705));
#38602=CARTESIAN_POINT('Ctrl Pts',(0.8947991495438,-0.8406685626417,-0.4426200204961));
#38603=CARTESIAN_POINT('Ctrl Pts',(0.2912626771974,-1.192709186308,-0.4839491815217));
#38604=CARTESIAN_POINT('Ctrl Pts',(-0.4066032511093,-1.158474404732,-0.5252783425474));
#38605=CARTESIAN_POINT('Ctrl Pts',(-0.9727850795543,-0.749051626544,-0.566607503573));
#38606=CARTESIAN_POINT('Ctrl Pts',(-1.223916973674,-0.0970380945375,-0.6079366645986));
#38607=CARTESIAN_POINT('Ctrl Pts',(-1.078666387945,0.5864025696815,-0.6492658256243));
#38608=CARTESIAN_POINT('Ctrl Pts',(-0.5840747383189,1.079928632059,-0.6905949866499));
#38609=CARTESIAN_POINT('Ctrl Pts',(0.09967761288844,1.223704835204,-0.7319241476755));
#38610=CARTESIAN_POINT('Ctrl Pts',(0.751147986558,0.9711672626034,-0.7732533087011));
#38611=CARTESIAN_POINT('Ctrl Pts',(1.159348673814,0.4041037077322,-0.8145824697268));
#38612=CARTESIAN_POINT('Ctrl Pts',(1.192078210377,-0.293834433769,-0.8559116307524));
#38613=CARTESIAN_POINT('Ctrl Pts',(0.8387367290116,-0.8966102257221,-0.897240791778));
#38614=CARTESIAN_POINT('Ctrl Pts',(0.2137585919034,-1.209006345536,-0.9385699528036));
#38615=CARTESIAN_POINT('Ctrl Pts',(-0.4804477131443,-1.129849074849,-0.9798991138293));
#38616=CARTESIAN_POINT('Ctrl Pts',(-1.019056289477,-0.6847742349804,-1.021228274855));
#38617=CARTESIAN_POINT('Ctrl Pts',(-1.227622178466,-0.01792681998115,-1.062557435881));
#38618=CARTESIAN_POINT('Ctrl Pts',(-1.038632402532,0.654730378946,-1.103886596906));
#38619=CARTESIAN_POINT('Ctrl Pts',(-0.5131671166336,1.115329383049,-1.145215757932));
#38620=CARTESIAN_POINT('Ctrl Pts',(-0.0523082239727,1.181621999622,-1.172768531949));
#38621=CARTESIAN_POINT('Ctrl Pts',(0.1687388712651,1.149164293121,-1.186544918957));
#38622=CARTESIAN_POINT('Ctrl Pts',(0.5344778275383,0.91366505645,0.07653650123427));
#38623=CARTESIAN_POINT('Ctrl Pts',(0.7102255495633,0.8108557610746,0.06276011422573));
#38624=CARTESIAN_POINT('Ctrl Pts',(1.00033926551,0.5012032856962,0.03520734020864));
#38625=CARTESIAN_POINT('Ctrl Pts',(1.111832845205,-0.1257706506175,-0.006121820816984));
#38626=CARTESIAN_POINT('Ctrl Pts',(0.863164431317,-0.7119655046093,-0.04745098184261));
#38627=CARTESIAN_POINT('Ctrl Pts',(0.3349695551186,-1.06759292277,-0.08878014286824));
#38628=CARTESIAN_POINT('Ctrl Pts',(-0.301715564144,-1.077462232679,-0.1301093038939));
#38629=CARTESIAN_POINT('Ctrl Pts',(-0.8406843854358,-0.7383813558381,-0.1714384649195));
#38630=CARTESIAN_POINT('Ctrl Pts',(-1.107386323452,-0.1601652005091,-0.2127676259451));
#38631=CARTESIAN_POINT('Ctrl Pts',(-1.015445738419,0.4699226112277,-0.2540967869707));
#38632=CARTESIAN_POINT('Ctrl Pts',(-0.5946390026802,0.947819487708,-0.2954259479964));
#38633=CARTESIAN_POINT('Ctrl Pts',(0.01874982580589,1.11875187828,-0.336755109022));
#38634=CARTESIAN_POINT('Ctrl Pts',(0.6260662611517,0.9273609643639,-0.3780842700476));
#38635=CARTESIAN_POINT('Ctrl Pts',(1.03062245885,0.435631345235,-0.4194134310733));
#38636=CARTESIAN_POINT('Ctrl Pts',(1.101397284947,-0.1971835243837,-0.4607425920989));
#38637=CARTESIAN_POINT('Ctrl Pts',(0.8154693310105,-0.7661377759785,-0.5020717531245));
#38638=CARTESIAN_POINT('Ctrl Pts',(0.2654403288644,-1.086967687379,-0.5434009141501));
#38639=CARTESIAN_POINT('Ctrl Pts',(-0.3705552037435,-1.055768043925,-0.5847300751758));
#38640=CARTESIAN_POINT('Ctrl Pts',(-0.8865412963853,-0.682643282687,-0.6260592362014));
#38641=CARTESIAN_POINT('Ctrl Pts',(-1.115408699531,-0.08843503044831,-0.667388397227));
#38642=CARTESIAN_POINT('Ctrl Pts',(-0.9830355317275,0.5344141324282,-0.7087175582527));
#38643=CARTESIAN_POINT('Ctrl Pts',(-0.532292678597,0.9841858696144,-0.7500467192783));
#38644=CARTESIAN_POINT('Ctrl Pts',(0.09084053817027,1.115215368529,-0.7913758803039));
#38645=CARTESIAN_POINT('Ctrl Pts',(0.6845537866242,0.8850669095274,-0.8327050413295));
#38646=CARTESIAN_POINT('Ctrl Pts',(1.056564803313,0.3682772612952,-0.8740342023552));
#38647=CARTESIAN_POINT('Ctrl Pts',(1.086392651607,-0.2677840823335,-0.9153633633808));
#38648=CARTESIAN_POINT('Ctrl Pts',(0.7643772120813,-0.8171198433967,-0.9566925244064));
#38649=CARTESIAN_POINT('Ctrl Pts',(0.1948074895087,-1.101819996459,-0.998021685432));
#38650=CARTESIAN_POINT('Ctrl Pts',(-0.4378528694657,-1.029680537447,-1.039350846458));
#38651=CARTESIAN_POINT('Ctrl Pts',(-0.9287102597998,-0.6240645038357,-1.080680007483));
#38652=CARTESIAN_POINT('Ctrl Pts',(-1.118785413596,-0.01633748970886,-1.122009168509));
#38653=CARTESIAN_POINT('Ctrl Pts',(-0.9465508219251,0.5966842328622,-1.163338329535));
#38654=CARTESIAN_POINT('Ctrl Pts',(-0.4676714830486,1.016448111641,-1.20466749056));
#38655=CARTESIAN_POINT('Ctrl Pts',(-0.04767075653918,1.076863452575,-1.232220264577));
#38656=CARTESIAN_POINT('Ctrl Pts',(0.1537790626378,1.047283334825,-1.245996651586));
#38657=CARTESIAN_POINT('Ctrl Pts',(0.4824831939496,0.824782641904,0.01708476860587));
#38658=CARTESIAN_POINT('Ctrl Pts',(0.6411339702457,0.7319747560673,0.003308381597328));
#38659=CARTESIAN_POINT('Ctrl Pts',(0.9030250816571,0.452445638792,-0.02424439241976));
#38660=CARTESIAN_POINT('Ctrl Pts',(1.00367243439,-0.1135355333533,-0.06557355344538));
#38661=CARTESIAN_POINT('Ctrl Pts',(0.7791947771597,-0.6427046604121,-0.106902714471));
#38662=CARTESIAN_POINT('Ctrl Pts',(0.3023833216316,-0.963736223799,-0.1482318754966));
#38663=CARTESIAN_POINT('Ctrl Pts',(-0.2723643181289,-0.9726454355976,-0.1895610365223));
#38664=CARTESIAN_POINT('Ctrl Pts',(-0.7589016166616,-0.6665507464705,-0.2308901975479));
#38665=CARTESIAN_POINT('Ctrl Pts',(-0.9996584755179,-0.144584140856,-0.2722193585735));
#38666=CARTESIAN_POINT('Ctrl Pts',(-0.9166619790597,0.4242079852378,-0.3135485195992));
#38667=CARTESIAN_POINT('Ctrl Pts',(-0.5367918190013,0.8556144897971,-0.3548776806248));
#38668=CARTESIAN_POINT('Ctrl Pts',(0.01692582063224,1.009918375764,-0.3962068416504));
#38669=CARTESIAN_POINT('Ctrl Pts',(0.5651617966938,0.8371461957389,-0.437536002676));
#38670=CARTESIAN_POINT('Ctrl Pts',(0.930362290223,0.3932526140544,-0.4788651637017));
#38671=CARTESIAN_POINT('Ctrl Pts',(0.9942520577446,-0.1780012785134,-0.5201943247273));
#38672=CARTESIAN_POINT('Ctrl Pts',(0.7361395124771,-0.6916069893153,-0.5615234857529));
#38673=CARTESIAN_POINT('Ctrl Pts',(0.2396179805314,-0.9812261884506,-0.6028526467785));
#38674=CARTESIAN_POINT('Ctrl Pts',(-0.3345071563778,-0.9530616831182,-0.6441818078042));
#38675=CARTESIAN_POINT('Ctrl Pts',(-0.8002975132164,-0.61623493883,-0.6855109688298));
#38676=CARTESIAN_POINT('Ctrl Pts',(-1.006900425388,-0.07983196635911,-0.7268401298554));
#38677=CARTESIAN_POINT('Ctrl Pts',(-0.8874046755098,0.482425695175,-0.7681692908811));
#38678=CARTESIAN_POINT('Ctrl Pts',(-0.4805106188751,0.88844310717,-0.8094984519067));
#38679=CARTESIAN_POINT('Ctrl Pts',(0.0820034634521,1.006725901854,-0.8508276129323));
#38680=CARTESIAN_POINT('Ctrl Pts',(0.6179595866904,0.7989665564513,-0.8921567739579));
#38681=CARTESIAN_POINT('Ctrl Pts',(0.953780932813,0.3324508148581,-0.9334859349836));
#38682=CARTESIAN_POINT('Ctrl Pts',(0.9807070928362,-0.2417337308981,-0.9748150960092));
#38683=CARTESIAN_POINT('Ctrl Pts',(0.6900176951509,-0.7376294610713,-1.016144257035));
#38684=CARTESIAN_POINT('Ctrl Pts',(0.1758563871141,-0.9946336473814,-1.05747341806));
#38685=CARTESIAN_POINT('Ctrl Pts',(-0.3952580257872,-0.929512000046,-1.098802579086));
#38686=CARTESIAN_POINT('Ctrl Pts',(-0.838364230123,-0.563354772691,-1.140131740112));
#38687=CARTESIAN_POINT('Ctrl Pts',(-1.009948648725,-0.01474815943658,-1.181460901137));
#38688=CARTESIAN_POINT('Ctrl Pts',(-0.8544692413182,0.5386380867785,-1.222790062163));
#38689=CARTESIAN_POINT('Ctrl Pts',(-0.4221758494636,0.917566840232,-1.264119223189));
#38690=CARTESIAN_POINT('Ctrl Pts',(-0.04303328910565,0.9721049055279,-1.291671997206));
#38691=CARTESIAN_POINT('Ctrl Pts',(0.1388192540106,0.9454023765286,-1.305448384214));
#38692=CARTESIAN_POINT('',(0.74999306484827,0.614597305574217,-4.00551630894776E-5));
#38693=CARTESIAN_POINT('Ctrl Pts',(0.749942259149723,0.614550663048058,
-8.01103261789551E-5));
#38694=CARTESIAN_POINT('Ctrl Pts',(0.791983524359411,0.563130688889933,
-0.00506365794800816));
#38695=CARTESIAN_POINT('Ctrl Pts',(0.828853698246298,0.507432374712272,
-0.0100335934428759));
#38696=CARTESIAN_POINT('Ctrl Pts',(0.883652016474552,0.40296070733887,-0.01863173248958));
#38697=CARTESIAN_POINT('Ctrl Pts',(0.903976280274475,0.355428000376728,
-0.0222930935158685));
#38698=CARTESIAN_POINT('Ctrl Pts',(0.945112425463336,0.232125211536002,
-0.0317283958672095));
#38699=CARTESIAN_POINT('Ctrl Pts',(0.960463073437942,0.15487698483769,-0.037641304524705));
#38700=CARTESIAN_POINT('Ctrl Pts',(0.972136041926485,0.00566423762840502,
-0.0489416354037443));
#38701=CARTESIAN_POINT('Ctrl Pts',(0.969920363139232,-0.0664489906790064,
-0.0543314837744917));
#38702=CARTESIAN_POINT('Ctrl Pts',(0.952845641494024,-0.187463666740853,
-0.0631691753546404));
#38703=CARTESIAN_POINT('Ctrl Pts',(0.941911392506289,-0.236942726623874,
-0.0667515552081078));
#38704=CARTESIAN_POINT('Ctrl Pts',(0.910032892029366,-0.340886784729333,
-0.0746354041702569));
#38705=CARTESIAN_POINT('Ctrl Pts',(0.887879663818006,-0.39458678324541,
-0.078978483112223));
#38706=CARTESIAN_POINT('Ctrl Pts',(0.837190085734205,-0.491974936808162,
-0.0872933748465481));
#38707=CARTESIAN_POINT('Ctrl Pts',(0.809447932280059,-0.536225496558952,
-0.0912601761201217));
#38708=CARTESIAN_POINT('Ctrl Pts',(0.745727613947211,-0.622018883008426,
-0.0992342754801228));
#38709=CARTESIAN_POINT('Ctrl Pts',(0.709374774495646,-0.663315871701172,
-0.103193347360063));
#38710=CARTESIAN_POINT('Ctrl Pts',(0.639665749887592,-0.730196799627268,
-0.110110728583079));
#38711=CARTESIAN_POINT('Ctrl Pts',(0.607654488054685,-0.757179480716653,
-0.113094028586163));
#38712=CARTESIAN_POINT('Ctrl Pts',(0.515932509582186,-0.824619428772014,
-0.12140492900092));
#38713=CARTESIAN_POINT('Ctrl Pts',(0.453268841285773,-0.860336599303275,
-0.126895272802062));
#38714=CARTESIAN_POINT('Ctrl Pts',(0.350267581391511,-0.90503139921325,
-0.135421322538143));
#38715=CARTESIAN_POINT('Ctrl Pts',(0.311820637222686,-0.918937827419921,
-0.138498935117359));
#38716=CARTESIAN_POINT('Ctrl Pts',(0.201231201838853,-0.951361775068941,
-0.146975200161323));
#38717=CARTESIAN_POINT('Ctrl Pts',(0.127398061288026,-0.964243706377321,
-0.152233261936751));
#38718=CARTESIAN_POINT('Ctrl Pts',(-0.0336134095385275,-0.973378111806249,
-0.163901967566458));
#38719=CARTESIAN_POINT('Ctrl Pts',(-0.123625851787474,-0.96679156459634,
-0.170751849284573));
#38720=CARTESIAN_POINT('Ctrl Pts',(-0.316887057539714,-0.92183570319369,
-0.185752030374903));
#38721=CARTESIAN_POINT('Ctrl Pts',(-0.412369132536766,-0.883411422569636,
-0.1929868936821));
#38722=CARTESIAN_POINT('Ctrl Pts',(-0.546681183057338,-0.803098998306091,
-0.204307268407498));
#38723=CARTESIAN_POINT('Ctrl Pts',(-0.591282134992225,-0.770982938595183,
-0.208336742454701));
#38724=CARTESIAN_POINT('Ctrl Pts',(-0.660253360078768,-0.711392617957626,
-0.215229605273813));
#38725=CARTESIAN_POINT('Ctrl Pts',(-0.686096589098383,-0.68637400301508,
-0.217973597276779));
#38726=CARTESIAN_POINT('Ctrl Pts',(-0.773158243241712,-0.592240477703788,
-0.227664066266423));
#38727=CARTESIAN_POINT('Ctrl Pts',(-0.826261125605108,-0.51551052279722,
-0.234333483418219));
#38728=CARTESIAN_POINT('Ctrl Pts',(-0.891002385709881,-0.386433201759339,
-0.244785638657728));
#38729=CARTESIAN_POINT('Ctrl Pts',(-0.910634463542769,-0.338015506376734,
-0.248568477582743));
#38730=CARTESIAN_POINT('Ctrl Pts',(-0.941663311231948,-0.23862283217278,
-0.256301109307229));
#38731=CARTESIAN_POINT('Ctrl Pts',(-0.952940373909301,-0.187919019203186,
-0.260257442745707));
#38732=CARTESIAN_POINT('Ctrl Pts',(-0.976579884718872,-0.0191923880794445,
-0.273064045851657));
#38733=CARTESIAN_POINT('Ctrl Pts',(-0.971486452655273,0.101515762448749,
-0.281615508345684));
#38734=CARTESIAN_POINT('Ctrl Pts',(-0.916250609043354,0.344322935157297,
-0.29983581525101));
#38735=CARTESIAN_POINT('Ctrl Pts',(-0.863336468372821,0.459566612118886,
-0.309279469701199));
#38736=CARTESIAN_POINT('Ctrl Pts',(-0.718479399789711,0.662138109821643,
-0.327620527323536));
#38737=CARTESIAN_POINT('Ctrl Pts',(-0.62926076313351,0.748204380563924,
-0.336486135655537));
#38738=CARTESIAN_POINT('Ctrl Pts',(-0.419514882340921,0.883880734586201,
-0.355016179589254));
#38739=CARTESIAN_POINT('Ctrl Pts',(-0.297907992893379,0.931346865568005,
-0.364531941465149));
#38740=CARTESIAN_POINT('Ctrl Pts',(-0.0747702911518417,0.97190093761318,
-0.381256259175794));
#38741=CARTESIAN_POINT('Ctrl Pts',(0.0548610048127376,0.980868053947884,
-0.390482407034185));
#38742=CARTESIAN_POINT('Ctrl Pts',(0.305117797151989,0.925811521815035,
-0.409544191108791));
#38743=CARTESIAN_POINT('Ctrl Pts',(0.400680065497012,0.888629667696109,
-0.417137232122319));
#38744=CARTESIAN_POINT('Ctrl Pts',(0.539981830635489,0.807861115764787,
-0.428956507776047));
#38745=CARTESIAN_POINT('Ctrl Pts',(0.589067024577443,0.773041452413226,
-0.433253104806547));
#38746=CARTESIAN_POINT('Ctrl Pts',(0.682940467548811,0.69172444342647,-0.442355819649039));
#38747=CARTESIAN_POINT('Ctrl Pts',(0.727022565187571,0.6449176869188,-0.447147826651843));
#38748=CARTESIAN_POINT('Ctrl Pts',(0.823468275286885,0.520157342563299,
-0.458978900547134));
#38749=CARTESIAN_POINT('Ctrl Pts',(0.870238754511863,0.437739837279528,
-0.466015568909245));
#38750=CARTESIAN_POINT('Ctrl Pts',(0.921483109890555,0.306373388564749,
-0.476189946572354));
#38751=CARTESIAN_POINT('Ctrl Pts',(0.935462861091772,0.261002090651833,
-0.479570604180273));
#38752=CARTESIAN_POINT('Ctrl Pts',(0.9599443780831,0.152734089995508,-0.487718202795412));
#38753=CARTESIAN_POINT('Ctrl Pts',(0.967683840302401,0.0894680808929378,
-0.492505558444665));
#38754=CARTESIAN_POINT('Ctrl Pts',(0.971177436970066,-0.0491146553268897,
-0.502969086788959));
#38755=CARTESIAN_POINT('Ctrl Pts',(0.964444230504448,-0.124564260901227,
-0.508635168130123));
#38756=CARTESIAN_POINT('Ctrl Pts',(0.939038261849135,-0.247481041764794,
-0.517709582193673));
#38757=CARTESIAN_POINT('Ctrl Pts',(0.925059000873544,-0.295947373429156,
-0.521275659929971));
#38758=CARTESIAN_POINT('Ctrl Pts',(0.886885808674521,-0.397192666158041,
-0.529121629020463));
#38759=CARTESIAN_POINT('Ctrl Pts',(0.861547358587474,-0.449146237612015,
-0.53344245588854));
#38760=CARTESIAN_POINT('Ctrl Pts',(0.804855469806404,-0.54330017437357,
-0.541764954413461));
#38761=CARTESIAN_POINT('Ctrl Pts',(0.774161129252339,-0.586052779452843,
-0.545762573621421));
#38762=CARTESIAN_POINT('Ctrl Pts',(0.704972516616502,-0.66784568297347,
-0.553757270164554));
#38763=CARTESIAN_POINT('Ctrl Pts',(0.666184984261621,-0.706672470628262,
-0.557708044978171));
#38764=CARTESIAN_POINT('Ctrl Pts',(0.592531416782339,-0.768938598262087,
-0.564614415613664));
#38765=CARTESIAN_POINT('Ctrl Pts',(0.55890727215155,-0.793843373949183,
-0.567595783171078));
#38766=CARTESIAN_POINT('Ctrl Pts',(0.482442285068433,-0.842982043982225,
-0.574230428205313));
#38767=CARTESIAN_POINT('Ctrl Pts',(0.439226062869622,-0.866150678023914,
-0.577914785710056));
#38768=CARTESIAN_POINT('Ctrl Pts',(0.351273383110356,-0.905088258260573,
-0.585220395996211));
#38769=CARTESIAN_POINT('Ctrl Pts',(0.306537912905923,-0.921090214720483,
-0.588842029064422));
#38770=CARTESIAN_POINT('Ctrl Pts',(0.212318111789294,-0.947333946871234,
-0.596161639099133));
#38771=CARTESIAN_POINT('Ctrl Pts',(0.162693879292811,-0.957145637324262,
-0.599822161736598));
#38772=CARTESIAN_POINT('Ctrl Pts',(0.0630807526456533,-0.968979995725448,
-0.607028244911473));
#38773=CARTESIAN_POINT('Ctrl Pts',(0.0130963722548543,-0.971086087328877,
-0.610583547815589));
#38774=CARTESIAN_POINT('Ctrl Pts',(-0.0948203098140028,-0.967146775844488,
-0.618454240488956));
#38775=CARTESIAN_POINT('Ctrl Pts',(-0.152163307377428,-0.959666261898805,
-0.622811432133744));
#38776=CARTESIAN_POINT('Ctrl Pts',(-0.246590878698771,-0.938661050813737,
-0.630175650382095));
#38777=CARTESIAN_POINT('Ctrl Pts',(-0.284225753088723,-0.927866370246119,
-0.633153675375206));
#38778=CARTESIAN_POINT('Ctrl Pts',(-0.383838222143453,-0.892771238153227,
-0.641033652516603));
#38779=CARTESIAN_POINT('Ctrl Pts',(-0.444388465973063,-0.864294935496258,
-0.645816195732069));
#38780=CARTESIAN_POINT('Ctrl Pts',(-0.555347902358027,-0.797578903642003,
-0.655132530400022));
#38781=CARTESIAN_POINT('Ctrl Pts',(-0.606265079112514,-0.759872162087916,
-0.65968352933207));
#38782=CARTESIAN_POINT('Ctrl Pts',(-0.685742102906565,-0.687430621601045,
-0.667745538161171));
#38783=CARTESIAN_POINT('Ctrl Pts',(-0.716337706344111,-0.655319110682923,
-0.67113286930802));
#38784=CARTESIAN_POINT('Ctrl Pts',(-0.808431881110594,-0.544440049093277,
-0.682047581387006));
#38785=CARTESIAN_POINT('Ctrl Pts',(-0.860482686265615,-0.457700340596788,
-0.689255051361111));
#38786=CARTESIAN_POINT('Ctrl Pts',(-0.956498986002975,-0.222988363490985,
-0.707619665221014));
#38787=CARTESIAN_POINT('Ctrl Pts',(-0.970872220697877,-0.0926079183447355,
-0.717487448773803));
#38788=CARTESIAN_POINT('Ctrl Pts',(-0.968471358047173,0.0968236024967683,
-0.731486319252523));
#38789=CARTESIAN_POINT('Ctrl Pts',(-0.956077990535885,0.18282017286137,
-0.737708137479027));
#38790=CARTESIAN_POINT('Ctrl Pts',(-0.897463278185653,0.390384619048993,
-0.753470239990772));
#38791=CARTESIAN_POINT('Ctrl Pts',(-0.839165556372643,0.502339013087694,
-0.762874973552972));
#38792=CARTESIAN_POINT('Ctrl Pts',(-0.681628130937872,0.700824545961502,
-0.781551104288793));
#38793=CARTESIAN_POINT('Ctrl Pts',(-0.58382868541532,0.784948724465537,
-0.790752835947921));
#38794=CARTESIAN_POINT('Ctrl Pts',(-0.367879607316997,0.905580061152143,
-0.809112470384984));
#38795=CARTESIAN_POINT('Ctrl Pts',(-0.251227423629182,0.944074570175999,
-0.818081691658179));
#38796=CARTESIAN_POINT('Ctrl Pts',(-0.0414591985823136,0.973069690006431,
-0.833704184817049));
#38797=CARTESIAN_POINT('Ctrl Pts',(0.0914991124827709,0.979358329861489,
-0.843139905578241));
#38798=CARTESIAN_POINT('Ctrl Pts',(0.366894717045133,0.905774711964452,
-0.86432281438767));
#38799=CARTESIAN_POINT('Ctrl Pts',(0.479709653824472,0.851493263089896,
-0.873558629646538));
#38800=CARTESIAN_POINT('Ctrl Pts',(0.613243488570379,0.752718937475823,
-0.885668616486831));
#38801=CARTESIAN_POINT('Ctrl Pts',(0.646332450220662,0.724629142748078,
-0.888781829972234));
#38802=CARTESIAN_POINT('Ctrl Pts',(0.723720361021099,0.64901667464327,-0.896708056507243));
#38803=CARTESIAN_POINT('Ctrl Pts',(0.76532774394799,0.599040606791593,-0.901552489526432));
#38804=CARTESIAN_POINT('Ctrl Pts',(0.837280957327974,0.492922625274083,
-0.911169298602814));
#38805=CARTESIAN_POINT('Ctrl Pts',(0.867844069777876,0.436877849438058,
-0.915942103711501));
#38806=CARTESIAN_POINT('Ctrl Pts',(0.919704693491599,0.315108995311966,
-0.925696753666225));
#38807=CARTESIAN_POINT('Ctrl Pts',(0.940019434097609,0.248948964472203,
-0.930583205817245));
#38808=CARTESIAN_POINT('Ctrl Pts',(0.962038031158095,0.133358754910732,
-0.939148061290653));
#38809=CARTESIAN_POINT('Ctrl Pts',(0.967403938251554,0.0847432434698806,
-0.942785265685722));
#38810=CARTESIAN_POINT('Ctrl Pts',(0.972891026474809,-0.0722954589448364,
-0.954601302008364));
#38811=CARTESIAN_POINT('Ctrl Pts',(0.958551136764753,-0.181393992542052,
-0.962853996903281));
#38812=CARTESIAN_POINT('Ctrl Pts',(0.913251694825849,-0.329836589486158,
-0.974011839960728));
#38813=CARTESIAN_POINT('Ctrl Pts',(0.89638517457652,-0.373562923404985,
-0.977335956267267));
#38814=CARTESIAN_POINT('Ctrl Pts',(0.84934792524559,-0.472776728484108,
-0.9853447168436));
#38815=CARTESIAN_POINT('Ctrl Pts',(0.816640996218955,-0.52686934189899,
-0.990108581234102));
#38816=CARTESIAN_POINT('Ctrl Pts',(0.739823597464444,-0.630112006451014,
-0.999865949489146));
#38817=CARTESIAN_POINT('Ctrl Pts',(0.695147302894014,-0.679014457321637,
-1.00486018760927));
#38818=CARTESIAN_POINT('Ctrl Pts',(0.612977208335645,-0.752633887809531,
-1.01289439295814));
#38819=CARTESIAN_POINT('Ctrl Pts',(0.577871549805956,-0.780050049767168,
-1.01606063470027));
#38820=CARTESIAN_POINT('Ctrl Pts',(0.49706649081279,-0.83462082236835,-1.02304974459024));
#38821=CARTESIAN_POINT('Ctrl Pts',(0.450801544925927,-0.8605767780256,-1.02688818266538));
#38822=CARTESIAN_POINT('Ctrl Pts',(0.355596389864133,-0.903785060190799,
-1.03473028500779));
#38823=CARTESIAN_POINT('Ctrl Pts',(0.307265162344229,-0.921182218996251,
-1.03865156049473));
#38824=CARTESIAN_POINT('Ctrl Pts',(0.207636054043817,-0.948485892976383,
-1.04648091965244));
#38825=CARTESIAN_POINT('Ctrl Pts',(0.15627754791737,-0.958263403146292,
-1.05036439257441));
#38826=CARTESIAN_POINT('Ctrl Pts',(0.0452409221182438,-0.970418428176485,
-1.05846212592755));
#38827=CARTESIAN_POINT('Ctrl Pts',(-0.014592215616271,-0.971535239894634,
-1.06268803907717));
#38828=CARTESIAN_POINT('Ctrl Pts',(-0.121223996625228,-0.963571095923621,
-1.07043210119647));
#38829=CARTESIAN_POINT('Ctrl Pts',(-0.167744946763637,-0.956571121920403,
-1.07391006816536));
#38830=CARTESIAN_POINT('Ctrl Pts',(-0.249386558305709,-0.937956544665916,
-1.0802478199119));
#38831=CARTESIAN_POINT('Ctrl Pts',(-0.284409709922977,-0.927838590886795,
-1.08303157260172));
#38832=CARTESIAN_POINT('Ctrl Pts',(-0.370096933566187,-0.897817774242533,
-1.08991847173514));
#38833=CARTESIAN_POINT('Ctrl Pts',(-0.419951230586404,-0.875543746334502,
-1.09395546676393));
#38834=CARTESIAN_POINT('Ctrl Pts',(-0.53718092214749,-0.811100788087201,
-1.10366225027211));
#38835=CARTESIAN_POINT('Ctrl Pts',(-0.602145102563672,-0.764469256881141,
-1.10928973709699));
#38836=CARTESIAN_POINT('Ctrl Pts',(-0.694162572215653,-0.679135878923541,
-1.11853453562391));
#38837=CARTESIAN_POINT('Ctrl Pts',(-0.725451186358578,-0.645480474978077,
-1.12200914481219));
#38838=CARTESIAN_POINT('Ctrl Pts',(-0.797876204012436,-0.555501978720714,
-1.13079010844328));
#38839=CARTESIAN_POINT('Ctrl Pts',(-0.835686460518628,-0.496481257598879,
-1.13600950543592));
#38840=CARTESIAN_POINT('Ctrl Pts',(-0.903359586564656,-0.361389621174484,
-1.14701804001649));
#38841=CARTESIAN_POINT('Ctrl Pts',(-0.947933188046413,-0.250988328500812,
-1.15526661898464));
#38842=CARTESIAN_POINT('Ctrl Pts',(-0.96863761515076,-0.0660972046724641,
-1.16930417636519));
#38843=CARTESIAN_POINT('Ctrl Pts',(-0.970507420996907,-0.0228215652799758,
-1.17259199202591));
#38844=CARTESIAN_POINT('Ctrl Pts',(-0.967880972425023,0.0906473176846458,
-1.18106168070997));
#38845=CARTESIAN_POINT('Ctrl Pts',(-0.958669179681034,0.160761742191593,
-1.18618840283058));
#38846=CARTESIAN_POINT('Ctrl Pts',(-0.927176450774154,0.291022169363798,
-1.19594157664097));
#38847=CARTESIAN_POINT('Ctrl Pts',(-0.906184283733861,0.351524969776246,
-1.20057529257284));
#38848=CARTESIAN_POINT('Ctrl Pts',(-0.846738408387065,0.479668453351846,
-1.21103506207018));
#38849=CARTESIAN_POINT('Ctrl Pts',(-0.805691619443741,0.545257313881333,
-1.21686511129903));
#38850=CARTESIAN_POINT('Ctrl Pts',(-0.688381393394236,0.691533926080835,
-1.23075331546858));
#38851=CARTESIAN_POINT('Ctrl Pts',(-0.604306969817395,0.766315083863186,
-1.23882509336762));
#38852=CARTESIAN_POINT('Ctrl Pts',(-0.414950826661446,0.884032183373647,
-1.25522713697232));
#38853=CARTESIAN_POINT('Ctrl Pts',(-0.312130052609453,0.925099829793529,
-1.26336940557668));
#38854=CARTESIAN_POINT('Ctrl Pts',(-0.201489314110026,0.948458138715504,
-1.27174112566436));
#38855=CARTESIAN_POINT('Ctrl Pts',(0.000261914023966756,-1.24958349387703,
-2.05998412772246E-17));
#38856=CARTESIAN_POINT('Ctrl Pts',(0.156016439362075,-1.23406571896253,
-1.91588362189685E-17));
#38857=CARTESIAN_POINT('Ctrl Pts',(0.309361253433594,-1.19037621015537,
6.20163642661709E-16));
#38858=CARTESIAN_POINT('Ctrl Pts',(0.58815550652336,-1.04085178026832,6.20163642661709E-16));
#38859=CARTESIAN_POINT('Ctrl Pts',(0.708122763155166,-0.943561790489167,
2.60208521396521E-17));
#38860=CARTESIAN_POINT('Ctrl Pts',(0.928835256908631,-0.678043480207547,
2.60208521396521E-17));
#38861=CARTESIAN_POINT('Ctrl Pts',(0.985613606267667,-0.53354825918773,
1.31001685194088E-10));
#38862=CARTESIAN_POINT('Ctrl Pts',(1.05519459948604,-0.306237812616919,
1.31001685194088E-10));
#38863=CARTESIAN_POINT('Ctrl Pts',(1.07176070683132,-0.165494960865087,
-1.73472347597681E-17));
#38864=CARTESIAN_POINT('Ctrl Pts',(1.04494763475789,0.102321842499411,-1.73472347597681E-17));
#38865=CARTESIAN_POINT('Ctrl Pts',(1.01124950363173,0.222287506844967,2.51534904016637E-15));
#38866=CARTESIAN_POINT('Ctrl Pts',(0.892911145490497,0.464634040295056,
2.51534904016637E-15));
#38867=CARTESIAN_POINT('Ctrl Pts',(0.813327676481858,0.554951540676525,
0.));
#38868=CARTESIAN_POINT('Ctrl Pts',(0.750043870546816,0.614643948100375,
0.));
#38869=CARTESIAN_POINT('Origin',(0.,0.,0.));
#38870=CARTESIAN_POINT('Ctrl Pts',(0.749944789178387,0.614547568599164,
-3.81639164714898E-17));
#38871=CARTESIAN_POINT('Ctrl Pts',(0.730682841831246,0.638106731811761,
-3.84621583023737E-17));
#38872=CARTESIAN_POINT('Ctrl Pts',(0.71051437582472,0.660555707618496,1.10349477427045E-17));
#38873=CARTESIAN_POINT('Ctrl Pts',(0.689467072170113,0.681929481619668,
0.));
#38874=CARTESIAN_POINT('Ctrl Pts',(0.672065821349576,0.699600647887774,
-9.12334884379743E-18));
#38875=CARTESIAN_POINT('Ctrl Pts',(0.654061014915041,0.716538155044498,
-4.71483132268289E-17));
#38876=CARTESIAN_POINT('Ctrl Pts',(0.635452996963201,0.732740730419006,
-1.04083408558608E-17));
#38877=CARTESIAN_POINT('Ctrl Pts',(0.614550903662948,0.750940827982265,
3.08610910811809E-17));
#38878=CARTESIAN_POINT('Ctrl Pts',(0.592891705743417,0.768209749170047,
-4.16188708512546E-17));
#38879=CARTESIAN_POINT('Ctrl Pts',(0.570482844003363,0.784505783724916,
-3.46944695195361E-17));
#38880=CARTESIAN_POINT('Ctrl Pts',(0.55812694614723,0.793491163739113,-3.68990344897851E-17));
#38881=CARTESIAN_POINT('Ctrl Pts',(0.545544606031477,0.802179299411958,
7.41430263895259E-17));
#38882=CARTESIAN_POINT('Ctrl Pts',(0.532735933416764,0.810573129558699,
5.55111512312578E-17));
#38883=CARTESIAN_POINT('Ctrl Pts',(0.513532008218362,0.823157921996984,
2.75765519477732E-17));
#38884=CARTESIAN_POINT('Ctrl Pts',(0.49380962086728,0.835091709771066,-1.22052527852199E-17));
#38885=CARTESIAN_POINT('Ctrl Pts',(0.473457409740538,0.846417134999195,
-6.93889390390723E-18));
#38886=CARTESIAN_POINT('Ctrl Pts',(0.455793315912445,0.856246699591803,
-2.36811499282974E-18));
#38887=CARTESIAN_POINT('Ctrl Pts',(0.437653628660792,0.865617731461489,
7.3032627247367E-17));
#38888=CARTESIAN_POINT('Ctrl Pts',(0.418956034393796,0.874528239752056,
4.16333634234434E-17));
#38889=CARTESIAN_POINT('Ctrl Pts',(0.395466891195609,0.885722204184967,
2.18755056934525E-18));
#38890=CARTESIAN_POINT('Ctrl Pts',(0.371103317522214,0.89618643526344,-1.13375735736027E-17));
#38891=CARTESIAN_POINT('Ctrl Pts',(0.345777858685626,0.905826232280199,
1.38777878078145E-17));
#38892=CARTESIAN_POINT('Ctrl Pts',(0.323399828563073,0.914344129997601,
3.61585338422832E-17));
#38893=CARTESIAN_POINT('Ctrl Pts',(0.300270073851916,0.922218006361476,
5.83990733107664E-17));
#38894=CARTESIAN_POINT('Ctrl Pts',(0.276333460210171,0.929346534537895,
4.16333634234434E-17));
#38895=CARTESIAN_POINT('Ctrl Pts',(0.254600684654987,0.935818740891543,
2.6411268290944E-17));
#38896=CARTESIAN_POINT('Ctrl Pts',(0.232200474936726,0.941678715556752,
7.26819386870289E-18));
#38897=CARTESIAN_POINT('Ctrl Pts',(0.209029079790626,0.946833180007271,
1.38777878078145E-17));
#38898=CARTESIAN_POINT('Ctrl Pts',(0.192470401980619,0.950516649025046,
1.86011174046147E-17));
#38899=CARTESIAN_POINT('Ctrl Pts',(0.175517891095409,0.953838936393204,
-1.55953622066509E-17));
#38900=CARTESIAN_POINT('Ctrl Pts',(0.15813628128911,0.95675004350001,-1.38777878078145E-17));
#38901=CARTESIAN_POINT('Ctrl Pts',(0.144196498316047,0.959084706499147,
-1.25003196315819E-17));
#38902=CARTESIAN_POINT('Ctrl Pts',(0.129979600100864,0.961154811600588,
2.22457029106987E-17));
#38903=CARTESIAN_POINT('Ctrl Pts',(0.115472874029535,0.962927165407642,
2.77555756156289E-17));
#38904=CARTESIAN_POINT('Ctrl Pts',(0.090329044023351,0.965999103391187,
3.73055803491087E-17));
#38905=CARTESIAN_POINT('Ctrl Pts',(0.0643321939263775,0.968169205716358,
1.79555613037849E-17));
#38906=CARTESIAN_POINT('Ctrl Pts',(0.0377310960825474,0.969238009639096,
-1.38777878078145E-17));
#38907=CARTESIAN_POINT('Ctrl Pts',(0.0234354151615083,0.969812394949669,
-3.09853299182623E-17));
#38908=CARTESIAN_POINT('Ctrl Pts',(0.0089657315485847,0.970069420136057,
-3.34851907640562E-17));
#38909=CARTESIAN_POINT('Ctrl Pts',(-0.00563632681277814,0.969983624511508,
-5.55111512312578E-17));
#38910=CARTESIAN_POINT('Ctrl Pts',(-0.0297733890182163,0.969841805168272,
-7.80420644965808E-17));
#38911=CARTESIAN_POINT('Ctrl Pts',(-0.0542700208752427,0.968761074770255,
5.50656997416883E-17));
#38912=CARTESIAN_POINT('Ctrl Pts',(-0.0789382482361072,0.966698551285329,
4.16333634234434E-17));
#38913=CARTESIAN_POINT('Ctrl Pts',(-0.105720565843984,0.964459267601142,
2.70498632704578E-17));
#38914=CARTESIAN_POINT('Ctrl Pts',(-0.132708401591014,0.961061724830605,
1.50291167672607E-17));
#38915=CARTESIAN_POINT('Ctrl Pts',(-0.159653017437302,0.956501006938883,
1.38777878078145E-17));
#38916=CARTESIAN_POINT('Ctrl Pts',(-0.181599435693551,0.952786297366793,
1.294002914617E-17));
#38917=CARTESIAN_POINT('Ctrl Pts',(-0.203516867164854,0.948300956670757,
-5.31396574931834E-18));
#38918=CARTESIAN_POINT('Ctrl Pts',(-0.225271705910235,0.943067776032336,
0.));
#38919=CARTESIAN_POINT('Ctrl Pts',(-0.239913324915326,0.939545698117194,
3.57644856936239E-18));
#38920=CARTESIAN_POINT('Ctrl Pts',(-0.254479084059815,0.935686010161577,
6.34983178660048E-17));
#38921=CARTESIAN_POINT('Ctrl Pts',(-0.26893705135892,0.931498981315315,
6.93889390390723E-17));
#38922=CARTESIAN_POINT('Ctrl Pts',(-0.302363902922641,0.921818561596446,
8.30080678900847E-17));
#38923=CARTESIAN_POINT('Ctrl Pts',(-0.335243053394182,0.910386042359239,
-2.12046701469247E-17));
#38924=CARTESIAN_POINT('Ctrl Pts',(-0.367493440333633,0.897221403951318,
-4.16333634234434E-17));
#38925=CARTESIAN_POINT('Ctrl Pts',(-0.386971348403746,0.889270503480971,
-5.397145444789E-17));
#38926=CARTESIAN_POINT('Ctrl Pts',(-0.406219625336411,0.880686830958701,
9.6942143763509E-18));
#38927=CARTESIAN_POINT('Ctrl Pts',(-0.42521626419776,0.871466546064191,
0.));
#38928=CARTESIAN_POINT('Ctrl Pts',(-0.438835063269308,0.864856471077914,
-6.94983774296248E-18));
#38929=CARTESIAN_POINT('Ctrl Pts',(-0.452327762572579,0.857917215840695,
4.71089931603229E-17));
#38930=CARTESIAN_POINT('Ctrl Pts',(-0.465671631291066,0.850652922959293,
4.16333634234434E-17));
#38931=CARTESIAN_POINT('Ctrl Pts',(-0.491771919138885,0.836444139943257,
3.09231627091158E-17));
#38932=CARTESIAN_POINT('Ctrl Pts',(-0.517289162072855,0.820994711100186,
4.19174349399959E-17));
#38933=CARTESIAN_POINT('Ctrl Pts',(-0.541979559119698,0.804412747338752,
5.55111512312578E-17));
#38934=CARTESIAN_POINT('Ctrl Pts',(-0.554737268949053,0.795844724650907,
6.25351244633398E-17));
#38935=CARTESIAN_POINT('Ctrl Pts',(-0.567274624913577,0.786975062654238,
3.61841045289072E-18));
#38936=CARTESIAN_POINT('Ctrl Pts',(-0.579561138071597,0.777823172216688,
0.));
#38937=CARTESIAN_POINT('Ctrl Pts',(-0.591997021826605,0.768560019672416,
-5.96044223634771E-17));
#38938=CARTESIAN_POINT('Ctrl Pts',(-0.604175244810911,0.759008321414952,
2.9479058197616E-17));
#38939=CARTESIAN_POINT('Ctrl Pts',(-0.616075811532905,0.749198177128338,
2.77555756156289E-17));
#38940=CARTESIAN_POINT('Ctrl Pts',(-0.636745216472705,0.732159505818413,
2.47621585602927E-17));
#38941=CARTESIAN_POINT('Ctrl Pts',(-0.656592760626642,0.714334970677369,
5.70078597589259E-17));
#38942=CARTESIAN_POINT('Ctrl Pts',(-0.675690425296587,0.69570759103261,
5.55111512312578E-17));
#38943=CARTESIAN_POINT('Ctrl Pts',(-0.694906682459675,0.676964539266104,
5.40051484574673E-17));
#38944=CARTESIAN_POINT('Ctrl Pts',(-0.713364184544054,0.657408093760942,
-5.91853539566696E-18));
#38945=CARTESIAN_POINT('Ctrl Pts',(-0.731099444893425,0.636983809797649,
-2.77555756156289E-17));
#38946=CARTESIAN_POINT('Ctrl Pts',(-0.737317170045828,0.629823351951712,
-3.54113253229913E-17));
#38947=CARTESIAN_POINT('Ctrl Pts',(-0.743445761422563,0.622555934095105,
3.31673986846265E-17));
#38948=CARTESIAN_POINT('Ctrl Pts',(-0.749485555517556,0.615178325990764,
2.77555756156289E-17));
#38949=CARTESIAN_POINT('Ctrl Pts',(-0.9278486567136,0.2828371797248,0.1713479786129));
#38950=CARTESIAN_POINT('Ctrl Pts',(-0.8680237607561,0.4790930234802,0.1561991832375));
#38951=CARTESIAN_POINT('Ctrl Pts',(-0.6198030816887,0.8317102040798,0.1259015924865));
#38952=CARTESIAN_POINT('Ctrl Pts',(-0.006020401385728,1.0373137838,0.08045520636017));
#38953=CARTESIAN_POINT('Ctrl Pts',(0.6100667263548,0.8389364077892,0.03500882023379));
#38954=CARTESIAN_POINT('Ctrl Pts',(0.9886505599867,0.3139752873927,-0.01043756589259));
#38955=CARTESIAN_POINT('Ctrl Pts',(0.9823257752865,-0.3332333632255,-0.05588395201896));
#38956=CARTESIAN_POINT('Ctrl Pts',(0.5935583558294,-0.8507036453223,-0.1013303381453));
#38957=CARTESIAN_POINT('Ctrl Pts',(-0.02629601796974,-1.036974907694,-0.1467767242717));
#38958=CARTESIAN_POINT('Ctrl Pts',(-0.6359126558604,-0.8195263571088,-0.1922231103981));
#38959=CARTESIAN_POINT('Ctrl Pts',(-0.9979529948525,-0.2830162467567,-0.2376694965245));
#38960=CARTESIAN_POINT('Ctrl Pts',(-0.9714658785124,0.363679007019,-0.2831158826508));
#38961=CARTESIAN_POINT('Ctrl Pts',(-0.5667633924888,0.8687851459845,-0.3285622687772));
#38962=CARTESIAN_POINT('Ctrl Pts',(0.05859391180608,1.035652029771,-0.3740086549036));
#38963=CARTESIAN_POINT('Ctrl Pts',(0.6611391764405,0.7993143077222,-0.41945504103));
#38964=CARTESIAN_POINT('Ctrl Pts',(1.006286827598,0.2517840220961,-0.4649014271564));
#38965=CARTESIAN_POINT('Ctrl Pts',(0.9596624628927,-0.3937719269989,-0.5103478132827));
#38966=CARTESIAN_POINT('Ctrl Pts',(0.5394180851663,-0.8860228566873,-0.5557941994091));
#38967=CARTESIAN_POINT('Ctrl Pts',(-0.09083491517071,-1.033323468892,-0.6012405855355));
#38968=CARTESIAN_POINT('Ctrl Pts',(-0.6857236666216,-0.7783260410752,-0.6466869716619));
#38969=CARTESIAN_POINT('Ctrl Pts',(-1.013643462657,-0.2203072939477,-0.6921333577882));
#38970=CARTESIAN_POINT('Ctrl Pts',(-0.9469271253684,0.4234824583282,-0.7375797439146));
#38971=CARTESIAN_POINT('Ctrl Pts',(-0.5115489524506,0.9024001563583,-0.783026130041));
#38972=CARTESIAN_POINT('Ctrl Pts',(0.1229877087451,1.029991454701,-0.8284725161674));
#38973=CARTESIAN_POINT('Ctrl Pts',(0.7096422575036,0.7565819468032,-0.8739189022937));
#38974=CARTESIAN_POINT('Ctrl Pts',(1.020015746615,0.1886166284744,-0.9193652884201));
#38975=CARTESIAN_POINT('Ctrl Pts',(0.9332722659451,-0.4527817546746,-0.9648116745465));
#38976=CARTESIAN_POINT('Ctrl Pts',(0.4831829360834,-0.9179011189761,-1.010258060673));
#38977=CARTESIAN_POINT('Ctrl Pts',(-0.1550206148297,-1.025659306074,-1.055704446799));
#38978=CARTESIAN_POINT('Ctrl Pts',(-0.7328734174699,-0.7341028298687,-1.101150832926));
#38979=CARTESIAN_POINT('Ctrl Pts',(-1.025391163463,-0.1567439594124,-1.146597219052));
#38980=CARTESIAN_POINT('Ctrl Pts',(-0.9187347609085,0.481645689685,-1.192043605178));
#38981=CARTESIAN_POINT('Ctrl Pts',(-0.4542594454663,0.9324945468184,-1.237489991305));
#38982=CARTESIAN_POINT('Ctrl Pts',(-0.02703741779296,0.9910925044735,-1.267787582056));
#38983=CARTESIAN_POINT('Ctrl Pts',(0.1747761851207,0.9541243551627,-1.282936377431));
#38984=CARTESIAN_POINT('Ctrl Pts',(-0.9278486567136,0.2828371797248,0.1179886138536));
#38985=CARTESIAN_POINT('Ctrl Pts',(-0.8680237607561,0.4790930234802,0.1028398184781));
#38986=CARTESIAN_POINT('Ctrl Pts',(-0.6198030816887,0.8317102040798,0.0725422277272));
#38987=CARTESIAN_POINT('Ctrl Pts',(-0.006020401385728,1.0373137838,0.02709584160082));
#38988=CARTESIAN_POINT('Ctrl Pts',(0.6100667263548,0.8389364077892,-0.01835054452555));
#38989=CARTESIAN_POINT('Ctrl Pts',(0.9886505599867,0.3139752873927,-0.06379693065193));
#38990=CARTESIAN_POINT('Ctrl Pts',(0.9823257752865,-0.3332333632255,-0.1092433167783));
#38991=CARTESIAN_POINT('Ctrl Pts',(0.5935583558294,-0.8507036453223,-0.1546897029047));
#38992=CARTESIAN_POINT('Ctrl Pts',(-0.02629601796974,-1.036974907694,-0.2001360890311));
#38993=CARTESIAN_POINT('Ctrl Pts',(-0.6359126558604,-0.8195263571088,-0.2455824751574));
#38994=CARTESIAN_POINT('Ctrl Pts',(-0.9979529948525,-0.2830162467567,-0.2910288612838));
#38995=CARTESIAN_POINT('Ctrl Pts',(-0.9714658785124,0.363679007019,-0.3364752474102));
#38996=CARTESIAN_POINT('Ctrl Pts',(-0.5667633924888,0.8687851459845,-0.3819216335366));
#38997=CARTESIAN_POINT('Ctrl Pts',(0.05859391180608,1.035652029771,-0.4273680196629));
#38998=CARTESIAN_POINT('Ctrl Pts',(0.6611391764405,0.7993143077222,-0.4728144057893));
#38999=CARTESIAN_POINT('Ctrl Pts',(1.006286827598,0.2517840220961,-0.5182607919157));
#39000=CARTESIAN_POINT('Ctrl Pts',(0.9596624628927,-0.3937719269989,-0.5637071780421));
#39001=CARTESIAN_POINT('Ctrl Pts',(0.5394180851663,-0.8860228566873,-0.6091535641684));
#39002=CARTESIAN_POINT('Ctrl Pts',(-0.09083491517071,-1.033323468892,-0.6545999502948));
#39003=CARTESIAN_POINT('Ctrl Pts',(-0.6857236666216,-0.7783260410752,-0.7000463364212));
#39004=CARTESIAN_POINT('Ctrl Pts',(-1.013643462657,-0.2203072939477,-0.7454927225476));
#39005=CARTESIAN_POINT('Ctrl Pts',(-0.9469271253684,0.4234824583282,-0.790939108674));
#39006=CARTESIAN_POINT('Ctrl Pts',(-0.5115489524506,0.9024001563583,-0.8363854948003));
#39007=CARTESIAN_POINT('Ctrl Pts',(0.1229877087451,1.029991454701,-0.8818318809267));
#39008=CARTESIAN_POINT('Ctrl Pts',(0.7096422575036,0.7565819468032,-0.9272782670531));
#39009=CARTESIAN_POINT('Ctrl Pts',(1.020015746615,0.1886166284744,-0.9727246531795));
#39010=CARTESIAN_POINT('Ctrl Pts',(0.9332722659451,-0.4527817546746,-1.018171039306));
#39011=CARTESIAN_POINT('Ctrl Pts',(0.4831829360834,-0.9179011189761,-1.063617425432));
#39012=CARTESIAN_POINT('Ctrl Pts',(-0.1550206148297,-1.025659306074,-1.109063811559));
#39013=CARTESIAN_POINT('Ctrl Pts',(-0.7328734174699,-0.7341028298687,-1.154510197685));
#39014=CARTESIAN_POINT('Ctrl Pts',(-1.025391163463,-0.1567439594124,-1.199956583811));
#39015=CARTESIAN_POINT('Ctrl Pts',(-0.9187347609085,0.481645689685,-1.245402969938));
#39016=CARTESIAN_POINT('Ctrl Pts',(-0.4542594454663,0.9324945468184,-1.290849356064));
#39017=CARTESIAN_POINT('Ctrl Pts',(-0.02703741779296,0.9910925044735,-1.321146946815));
#39018=CARTESIAN_POINT('Ctrl Pts',(0.1747761851207,0.9541243551627,-1.33629574219));
#39019=CARTESIAN_POINT('Ctrl Pts',(-0.9278486567136,0.2828371797248,0.06462924909423));
#39020=CARTESIAN_POINT('Ctrl Pts',(-0.8680237607561,0.4790930234802,0.04948045371878));
#39021=CARTESIAN_POINT('Ctrl Pts',(-0.6198030816887,0.8317102040798,0.01918286296786));
#39022=CARTESIAN_POINT('Ctrl Pts',(-0.006020401385728,1.0373137838,-0.02626352315852));
#39023=CARTESIAN_POINT('Ctrl Pts',(0.6100667263548,0.8389364077892,-0.07170990928489));
#39024=CARTESIAN_POINT('Ctrl Pts',(0.9886505599867,0.3139752873927,-0.1171562954113));
#39025=CARTESIAN_POINT('Ctrl Pts',(0.9823257752865,-0.3332333632255,-0.1626026815376));
#39026=CARTESIAN_POINT('Ctrl Pts',(0.5935583558294,-0.8507036453223,-0.208049067664));
#39027=CARTESIAN_POINT('Ctrl Pts',(-0.02629601796974,-1.036974907694,-0.2534954537904));
#39028=CARTESIAN_POINT('Ctrl Pts',(-0.6359126558604,-0.8195263571088,-0.2989418399168));
#39029=CARTESIAN_POINT('Ctrl Pts',(-0.9979529948525,-0.2830162467567,-0.3443882260432));
#39030=CARTESIAN_POINT('Ctrl Pts',(-0.9714658785124,0.363679007019,-0.3898346121695));
#39031=CARTESIAN_POINT('Ctrl Pts',(-0.5667633924888,0.8687851459845,-0.4352809982959));
#39032=CARTESIAN_POINT('Ctrl Pts',(0.05859391180608,1.035652029771,-0.4807273844223));
#39033=CARTESIAN_POINT('Ctrl Pts',(0.6611391764405,0.7993143077222,-0.5261737705487));
#39034=CARTESIAN_POINT('Ctrl Pts',(1.006286827598,0.2517840220961,-0.571620156675));
#39035=CARTESIAN_POINT('Ctrl Pts',(0.9596624628927,-0.3937719269989,-0.6170665428014));
#39036=CARTESIAN_POINT('Ctrl Pts',(0.5394180851663,-0.8860228566873,-0.6625129289278));
#39037=CARTESIAN_POINT('Ctrl Pts',(-0.09083491517071,-1.033323468892,-0.7079593150542));
#39038=CARTESIAN_POINT('Ctrl Pts',(-0.6857236666216,-0.7783260410752,-0.7534057011805));
#39039=CARTESIAN_POINT('Ctrl Pts',(-1.013643462657,-0.2203072939477,-0.7988520873069));
#39040=CARTESIAN_POINT('Ctrl Pts',(-0.9469271253684,0.4234824583282,-0.8442984734333));
#39041=CARTESIAN_POINT('Ctrl Pts',(-0.5115489524506,0.9024001563583,-0.8897448595597));
#39042=CARTESIAN_POINT('Ctrl Pts',(0.1229877087451,1.029991454701,-0.935191245686));
#39043=CARTESIAN_POINT('Ctrl Pts',(0.7096422575036,0.7565819468032,-0.9806376318124));
#39044=CARTESIAN_POINT('Ctrl Pts',(1.020015746615,0.1886166284744,-1.026084017939));
#39045=CARTESIAN_POINT('Ctrl Pts',(0.9332722659451,-0.4527817546746,-1.071530404065));
#39046=CARTESIAN_POINT('Ctrl Pts',(0.4831829360834,-0.9179011189761,-1.116976790192));
#39047=CARTESIAN_POINT('Ctrl Pts',(-0.1550206148297,-1.025659306074,-1.162423176318));
#39048=CARTESIAN_POINT('Ctrl Pts',(-0.7328734174699,-0.7341028298688,-1.207869562444));
#39049=CARTESIAN_POINT('Ctrl Pts',(-1.025391163463,-0.1567439594124,-1.253315948571));
#39050=CARTESIAN_POINT('Ctrl Pts',(-0.9187347609085,0.481645689685,-1.298762334697));
#39051=CARTESIAN_POINT('Ctrl Pts',(-0.4542594454663,0.9324945468184,-1.344208720823));
#39052=CARTESIAN_POINT('Ctrl Pts',(-0.02703741779297,0.9910925044735,-1.374506311574));
#39053=CARTESIAN_POINT('Ctrl Pts',(0.1747761851207,0.9541243551627,-1.38965510695));
#39054=CARTESIAN_POINT('Ctrl Pts',(-0.9278486567136,0.2828371797248,0.01126988433489));
#39055=CARTESIAN_POINT('Ctrl Pts',(-0.8680237607561,0.4790930234802,-0.003878911040566));
#39056=CARTESIAN_POINT('Ctrl Pts',(-0.6198030816887,0.8317102040798,-0.03417650179148));
#39057=CARTESIAN_POINT('Ctrl Pts',(-0.006020401385728,1.0373137838,-0.07962288791786));
#39058=CARTESIAN_POINT('Ctrl Pts',(0.6100667263548,0.8389364077892,-0.1250692740442));
#39059=CARTESIAN_POINT('Ctrl Pts',(0.9886505599867,0.3139752873927,-0.1705156601706));
#39060=CARTESIAN_POINT('Ctrl Pts',(0.9823257752865,-0.3332333632255,-0.215962046297));
#39061=CARTESIAN_POINT('Ctrl Pts',(0.5935583558294,-0.8507036453223,-0.2614084324234));
#39062=CARTESIAN_POINT('Ctrl Pts',(-0.02629601796974,-1.036974907694,-0.3068548185497));
#39063=CARTESIAN_POINT('Ctrl Pts',(-0.6359126558604,-0.8195263571088,-0.3523012046761));
#39064=CARTESIAN_POINT('Ctrl Pts',(-0.9979529948525,-0.2830162467567,-0.3977475908025));
#39065=CARTESIAN_POINT('Ctrl Pts',(-0.9714658785124,0.363679007019,-0.4431939769289));
#39066=CARTESIAN_POINT('Ctrl Pts',(-0.5667633924888,0.8687851459845,-0.4886403630552));
#39067=CARTESIAN_POINT('Ctrl Pts',(0.05859391180608,1.035652029771,-0.5340867491816));
#39068=CARTESIAN_POINT('Ctrl Pts',(0.6611391764405,0.7993143077222,-0.579533135308));
#39069=CARTESIAN_POINT('Ctrl Pts',(1.006286827598,0.2517840220961,-0.6249795214344));
#39070=CARTESIAN_POINT('Ctrl Pts',(0.9596624628927,-0.3937719269989,-0.6704259075608));
#39071=CARTESIAN_POINT('Ctrl Pts',(0.5394180851663,-0.8860228566873,-0.7158722936871));
#39072=CARTESIAN_POINT('Ctrl Pts',(-0.09083491517071,-1.033323468892,-0.7613186798135));
#39073=CARTESIAN_POINT('Ctrl Pts',(-0.6857236666216,-0.7783260410752,-0.8067650659399));
#39074=CARTESIAN_POINT('Ctrl Pts',(-1.013643462657,-0.2203072939477,-0.8522114520663));
#39075=CARTESIAN_POINT('Ctrl Pts',(-0.9469271253684,0.4234824583282,-0.8976578381926));
#39076=CARTESIAN_POINT('Ctrl Pts',(-0.5115489524506,0.9024001563583,-0.943104224319));
#39077=CARTESIAN_POINT('Ctrl Pts',(0.1229877087451,1.029991454701,-0.9885506104454));
#39078=CARTESIAN_POINT('Ctrl Pts',(0.7096422575036,0.7565819468032,-1.033996996572));
#39079=CARTESIAN_POINT('Ctrl Pts',(1.020015746615,0.1886166284744,-1.079443382698));
#39080=CARTESIAN_POINT('Ctrl Pts',(0.9332722659451,-0.4527817546746,-1.124889768825));
#39081=CARTESIAN_POINT('Ctrl Pts',(0.4831829360834,-0.9179011189761,-1.170336154951));
#39082=CARTESIAN_POINT('Ctrl Pts',(-0.1550206148297,-1.025659306074,-1.215782541077));
#39083=CARTESIAN_POINT('Ctrl Pts',(-0.7328734174699,-0.7341028298688,-1.261228927204));
#39084=CARTESIAN_POINT('Ctrl Pts',(-1.025391163463,-0.1567439594124,-1.30667531333));
#39085=CARTESIAN_POINT('Ctrl Pts',(-0.9187347609085,0.481645689685,-1.352121699456));
#39086=CARTESIAN_POINT('Ctrl Pts',(-0.4542594454663,0.9324945468184,-1.397568085583));
#39087=CARTESIAN_POINT('Ctrl Pts',(-0.02703741779297,0.9910925044735,-1.427865676334));
#39088=CARTESIAN_POINT('Ctrl Pts',(0.1747761851207,0.9541243551627,-1.443014471709));
#39089=CARTESIAN_POINT('',(-0.2015628224599,0.948826869667,-1.271666493096));
#39090=CARTESIAN_POINT('Ctrl Pts',(-0.5831303237782,0.7751509694829,-1.22376920223));
#39091=CARTESIAN_POINT('Ctrl Pts',(-0.400218113725,0.9127521084488,-1.240669293422));
#39092=CARTESIAN_POINT('Ctrl Pts',(0.06620921823847,1.052270487825,-1.274469475806));
#39093=CARTESIAN_POINT('Ctrl Pts',(0.7347269571914,0.7563971597966,-1.325169749382));
#39094=CARTESIAN_POINT('Ctrl Pts',(1.049982749214,0.09689423608854,-1.375870022958));
#39095=CARTESIAN_POINT('Ctrl Pts',(0.8607148729301,-0.6091341314935,-1.426570296534));
#39096=CARTESIAN_POINT('Ctrl Pts',(0.2578136123524,-1.022450654046,-1.47727057011));
#39097=CARTESIAN_POINT('Ctrl Pts',(-0.4689774525342,-0.944421661856,-1.527970843686));
#39098=CARTESIAN_POINT('Ctrl Pts',(-0.9704004517988,-0.4125477163584,-1.578671117262));
#39099=CARTESIAN_POINT('Ctrl Pts',(-1.005493306747,0.317577906859,-1.629371390838));
#39100=CARTESIAN_POINT('Ctrl Pts',(-0.5573923286712,0.8950901223419,-1.680071664414));
#39101=CARTESIAN_POINT('Ctrl Pts',(0.1585658204783,1.042463149571,-1.73077193799));
#39102=CARTESIAN_POINT('Ctrl Pts',(0.7983245141496,0.6888762627836,-1.781472211566));
#39103=CARTESIAN_POINT('Ctrl Pts',(1.054445113962,0.004247084557393,-1.832172485142));
#39104=CARTESIAN_POINT('Ctrl Pts',(0.8038478213541,-0.6824230477092,-1.882872758718));
#39105=CARTESIAN_POINT('Ctrl Pts',(0.1669581858966,-1.041152006244,-1.933573032294));
#39106=CARTESIAN_POINT('Ctrl Pts',(-0.5501638854909,-0.8995511297614,-1.98427330587));
#39107=CARTESIAN_POINT('Ctrl Pts',(-1.00290246203,-0.3256672958743,-2.034973579446));
#39108=CARTESIAN_POINT('Ctrl Pts',(-0.9736921777191,0.4047172828064,-2.085673853022));
#39109=CARTESIAN_POINT('Ctrl Pts',(-0.4765701535821,0.9406133236668,-2.136374126598));
#39110=CARTESIAN_POINT('Ctrl Pts',(0.2495695979012,1.024493802687,-2.187074400174));
#39111=CARTESIAN_POINT('Ctrl Pts',(0.8557776632566,0.6160496142012,-2.23777467375));
#39112=CARTESIAN_POINT('Ctrl Pts',(1.050738288296,-0.0884397242642,-2.288474947326));
#39113=CARTESIAN_POINT('Ctrl Pts',(0.7407623530892,-0.7504289932324,-2.339175220902));
#39114=CARTESIAN_POINT('Ctrl Pts',(0.07481004734727,-1.051796554468,-2.389875494478));
#39115=CARTESIAN_POINT('Ctrl Pts',(-0.6270925081245,-0.847719000077,-2.440575768054));
#39116=CARTESIAN_POINT('Ctrl Pts',(-1.02764329207,-0.2362666277473,-2.49127604163));
#39117=CARTESIAN_POINT('Ctrl Pts',(-0.9343555872731,0.4887246289065,-2.541976315206));
#39118=CARTESIAN_POINT('Ctrl Pts',(-0.3920607004213,0.9788572959625,-2.592676588782));
#39119=CARTESIAN_POINT('Ctrl Pts',(0.3386450271169,0.9985960285533,-2.643376862358));
#39120=CARTESIAN_POINT('Ctrl Pts',(0.9065968071483,0.5384556582503,-2.694077135934));
#39121=CARTESIAN_POINT('Ctrl Pts',(1.038942130304,-0.1804428298701,-2.74477740951));
#39122=CARTESIAN_POINT('Ctrl Pts',(0.6717869665382,-0.8126248283907,-2.795477683086));
#39123=CARTESIAN_POINT('Ctrl Pts',(0.212375641378,-0.9737492166778,-2.82927786547));
#39124=CARTESIAN_POINT('Ctrl Pts',(-0.01648200808866,-0.9698599607208,-2.846177956662));
#39125=CARTESIAN_POINT('Ctrl Pts',(-0.5831303237782,0.7751509694829,-1.277128566989));
#39126=CARTESIAN_POINT('Ctrl Pts',(-0.400218113725,0.9127521084488,-1.294028658181));
#39127=CARTESIAN_POINT('Ctrl Pts',(0.06620921823847,1.052270487825,-1.327828840565));
#39128=CARTESIAN_POINT('Ctrl Pts',(0.7347269571914,0.7563971597966,-1.378529114141));
#39129=CARTESIAN_POINT('Ctrl Pts',(1.049982749214,0.09689423608854,-1.429229387717));
#39130=CARTESIAN_POINT('Ctrl Pts',(0.8607148729301,-0.6091341314935,-1.479929661293));
#39131=CARTESIAN_POINT('Ctrl Pts',(0.2578136123524,-1.022450654046,-1.530629934869));
#39132=CARTESIAN_POINT('Ctrl Pts',(-0.4689774525342,-0.944421661856,-1.581330208445));
#39133=CARTESIAN_POINT('Ctrl Pts',(-0.9704004517988,-0.4125477163584,-1.632030482021));
#39134=CARTESIAN_POINT('Ctrl Pts',(-1.005493306747,0.317577906859,-1.682730755597));
#39135=CARTESIAN_POINT('Ctrl Pts',(-0.5573923286712,0.8950901223419,-1.733431029173));
#39136=CARTESIAN_POINT('Ctrl Pts',(0.1585658204783,1.042463149571,-1.784131302749));
#39137=CARTESIAN_POINT('Ctrl Pts',(0.7983245141496,0.6888762627836,-1.834831576325));
#39138=CARTESIAN_POINT('Ctrl Pts',(1.054445113962,0.004247084557393,-1.885531849901));
#39139=CARTESIAN_POINT('Ctrl Pts',(0.8038478213541,-0.6824230477092,-1.936232123477));
#39140=CARTESIAN_POINT('Ctrl Pts',(0.1669581858966,-1.041152006244,-1.986932397053));
#39141=CARTESIAN_POINT('Ctrl Pts',(-0.5501638854909,-0.8995511297614,-2.037632670629));
#39142=CARTESIAN_POINT('Ctrl Pts',(-1.00290246203,-0.3256672958743,-2.088332944205));
#39143=CARTESIAN_POINT('Ctrl Pts',(-0.9736921777191,0.4047172828064,-2.139033217781));
#39144=CARTESIAN_POINT('Ctrl Pts',(-0.4765701535821,0.9406133236668,-2.189733491357));
#39145=CARTESIAN_POINT('Ctrl Pts',(0.2495695979012,1.024493802687,-2.240433764933));
#39146=CARTESIAN_POINT('Ctrl Pts',(0.8557776632566,0.6160496142012,-2.291134038509));
#39147=CARTESIAN_POINT('Ctrl Pts',(1.050738288296,-0.0884397242642,-2.341834312085));
#39148=CARTESIAN_POINT('Ctrl Pts',(0.7407623530892,-0.7504289932324,-2.392534585661));
#39149=CARTESIAN_POINT('Ctrl Pts',(0.07481004734727,-1.051796554468,-2.443234859237));
#39150=CARTESIAN_POINT('Ctrl Pts',(-0.6270925081245,-0.847719000077,-2.493935132813));
#39151=CARTESIAN_POINT('Ctrl Pts',(-1.02764329207,-0.2362666277473,-2.544635406389));
#39152=CARTESIAN_POINT('Ctrl Pts',(-0.9343555872731,0.4887246289065,-2.595335679965));
#39153=CARTESIAN_POINT('Ctrl Pts',(-0.3920607004213,0.9788572959625,-2.646035953541));
#39154=CARTESIAN_POINT('Ctrl Pts',(0.3386450271169,0.9985960285533,-2.696736227117));
#39155=CARTESIAN_POINT('Ctrl Pts',(0.9065968071483,0.5384556582503,-2.747436500693));
#39156=CARTESIAN_POINT('Ctrl Pts',(1.038942130304,-0.1804428298701,-2.798136774269));
#39157=CARTESIAN_POINT('Ctrl Pts',(0.6717869665382,-0.8126248283907,-2.848837047845));
#39158=CARTESIAN_POINT('Ctrl Pts',(0.212375641378,-0.9737492166778,-2.882637230229));
#39159=CARTESIAN_POINT('Ctrl Pts',(-0.01648200808866,-0.9698599607208,-2.899537321421));
#39160=CARTESIAN_POINT('Ctrl Pts',(-0.5831303237782,0.7751509694829,-1.330487931748));
#39161=CARTESIAN_POINT('Ctrl Pts',(-0.400218113725,0.9127521084488,-1.34738802294));
#39162=CARTESIAN_POINT('Ctrl Pts',(0.06620921823847,1.052270487825,-1.381188205324));
#39163=CARTESIAN_POINT('Ctrl Pts',(0.7347269571914,0.7563971597966,-1.4318884789));
#39164=CARTESIAN_POINT('Ctrl Pts',(1.049982749214,0.09689423608854,-1.482588752476));
#39165=CARTESIAN_POINT('Ctrl Pts',(0.8607148729301,-0.6091341314935,-1.533289026052));
#39166=CARTESIAN_POINT('Ctrl Pts',(0.2578136123524,-1.022450654046,-1.583989299628));
#39167=CARTESIAN_POINT('Ctrl Pts',(-0.4689774525342,-0.944421661856,-1.634689573204));
#39168=CARTESIAN_POINT('Ctrl Pts',(-0.9704004517988,-0.4125477163584,-1.68538984678));
#39169=CARTESIAN_POINT('Ctrl Pts',(-1.005493306747,0.317577906859,-1.736090120356));
#39170=CARTESIAN_POINT('Ctrl Pts',(-0.5573923286712,0.8950901223419,-1.786790393932));
#39171=CARTESIAN_POINT('Ctrl Pts',(0.1585658204783,1.042463149571,-1.837490667508));
#39172=CARTESIAN_POINT('Ctrl Pts',(0.7983245141496,0.6888762627836,-1.888190941084));
#39173=CARTESIAN_POINT('Ctrl Pts',(1.054445113962,0.004247084557393,-1.93889121466));
#39174=CARTESIAN_POINT('Ctrl Pts',(0.8038478213541,-0.6824230477092,-1.989591488236));
#39175=CARTESIAN_POINT('Ctrl Pts',(0.1669581858966,-1.041152006244,-2.040291761812));
#39176=CARTESIAN_POINT('Ctrl Pts',(-0.5501638854909,-0.8995511297614,-2.090992035388));
#39177=CARTESIAN_POINT('Ctrl Pts',(-1.00290246203,-0.3256672958743,-2.141692308964));
#39178=CARTESIAN_POINT('Ctrl Pts',(-0.9736921777191,0.4047172828064,-2.19239258254));
#39179=CARTESIAN_POINT('Ctrl Pts',(-0.4765701535821,0.9406133236668,-2.243092856116));
#39180=CARTESIAN_POINT('Ctrl Pts',(0.2495695979012,1.024493802687,-2.293793129692));
#39181=CARTESIAN_POINT('Ctrl Pts',(0.8557776632566,0.6160496142012,-2.344493403268));
#39182=CARTESIAN_POINT('Ctrl Pts',(1.050738288296,-0.0884397242642,-2.395193676844));
#39183=CARTESIAN_POINT('Ctrl Pts',(0.7407623530892,-0.7504289932324,-2.44589395042));
#39184=CARTESIAN_POINT('Ctrl Pts',(0.07481004734727,-1.051796554468,-2.496594223996));
#39185=CARTESIAN_POINT('Ctrl Pts',(-0.6270925081245,-0.847719000077,-2.547294497572));
#39186=CARTESIAN_POINT('Ctrl Pts',(-1.02764329207,-0.2362666277473,-2.597994771148));
#39187=CARTESIAN_POINT('Ctrl Pts',(-0.9343555872731,0.4887246289065,-2.648695044724));
#39188=CARTESIAN_POINT('Ctrl Pts',(-0.3920607004213,0.9788572959625,-2.6993953183));
#39189=CARTESIAN_POINT('Ctrl Pts',(0.3386450271169,0.9985960285533,-2.750095591876));
#39190=CARTESIAN_POINT('Ctrl Pts',(0.9065968071483,0.5384556582503,-2.800795865452));
#39191=CARTESIAN_POINT('Ctrl Pts',(1.038942130304,-0.1804428298701,-2.851496139028));
#39192=CARTESIAN_POINT('Ctrl Pts',(0.6717869665382,-0.8126248283907,-2.902196412604));
#39193=CARTESIAN_POINT('Ctrl Pts',(0.212375641378,-0.9737492166778,-2.935996594988));
#39194=CARTESIAN_POINT('Ctrl Pts',(-0.01648200808866,-0.9698599607208,-2.95289668618));
#39195=CARTESIAN_POINT('Ctrl Pts',(-0.5831303237782,0.7751509694829,-1.383847296508));
#39196=CARTESIAN_POINT('Ctrl Pts',(-0.400218113725,0.9127521084488,-1.4007473877));
#39197=CARTESIAN_POINT('Ctrl Pts',(0.06620921823847,1.052270487825,-1.434547570084));
#39198=CARTESIAN_POINT('Ctrl Pts',(0.7347269571914,0.7563971597966,-1.48524784366));
#39199=CARTESIAN_POINT('Ctrl Pts',(1.049982749214,0.09689423608854,-1.535948117236));
#39200=CARTESIAN_POINT('Ctrl Pts',(0.8607148729301,-0.6091341314935,-1.586648390812));
#39201=CARTESIAN_POINT('Ctrl Pts',(0.2578136123524,-1.022450654046,-1.637348664388));
#39202=CARTESIAN_POINT('Ctrl Pts',(-0.4689774525342,-0.944421661856,-1.688048937964));
#39203=CARTESIAN_POINT('Ctrl Pts',(-0.9704004517988,-0.4125477163584,-1.73874921154));
#39204=CARTESIAN_POINT('Ctrl Pts',(-1.005493306747,0.317577906859,-1.789449485116));
#39205=CARTESIAN_POINT('Ctrl Pts',(-0.5573923286712,0.8950901223419,-1.840149758692));
#39206=CARTESIAN_POINT('Ctrl Pts',(0.1585658204783,1.042463149571,-1.890850032268));
#39207=CARTESIAN_POINT('Ctrl Pts',(0.7983245141496,0.6888762627836,-1.941550305844));
#39208=CARTESIAN_POINT('Ctrl Pts',(1.054445113962,0.004247084557393,-1.99225057942));
#39209=CARTESIAN_POINT('Ctrl Pts',(0.8038478213541,-0.6824230477092,-2.042950852996));
#39210=CARTESIAN_POINT('Ctrl Pts',(0.1669581858966,-1.041152006244,-2.093651126572));
#39211=CARTESIAN_POINT('Ctrl Pts',(-0.5501638854909,-0.8995511297614,-2.144351400148));
#39212=CARTESIAN_POINT('Ctrl Pts',(-1.00290246203,-0.3256672958743,-2.195051673724));
#39213=CARTESIAN_POINT('Ctrl Pts',(-0.9736921777191,0.4047172828064,-2.2457519473));
#39214=CARTESIAN_POINT('Ctrl Pts',(-0.4765701535821,0.9406133236668,-2.296452220876));
#39215=CARTESIAN_POINT('Ctrl Pts',(0.2495695979012,1.024493802687,-2.347152494452));
#39216=CARTESIAN_POINT('Ctrl Pts',(0.8557776632566,0.6160496142012,-2.397852768028));
#39217=CARTESIAN_POINT('Ctrl Pts',(1.050738288296,-0.0884397242642,-2.448553041604));
#39218=CARTESIAN_POINT('Ctrl Pts',(0.7407623530892,-0.7504289932324,-2.49925331518));
#39219=CARTESIAN_POINT('Ctrl Pts',(0.07481004734727,-1.051796554468,-2.549953588756));
#39220=CARTESIAN_POINT('Ctrl Pts',(-0.6270925081245,-0.847719000077,-2.600653862332));
#39221=CARTESIAN_POINT('Ctrl Pts',(-1.02764329207,-0.2362666277473,-2.651354135908));
#39222=CARTESIAN_POINT('Ctrl Pts',(-0.9343555872731,0.4887246289065,-2.702054409484));
#39223=CARTESIAN_POINT('Ctrl Pts',(-0.3920607004213,0.9788572959625,-2.75275468306));
#39224=CARTESIAN_POINT('Ctrl Pts',(0.3386450271169,0.9985960285533,-2.803454956636));
#39225=CARTESIAN_POINT('Ctrl Pts',(0.9065968071483,0.5384556582503,-2.854155230212));
#39226=CARTESIAN_POINT('Ctrl Pts',(1.038942130304,-0.1804428298701,-2.904855503788));
#39227=CARTESIAN_POINT('Ctrl Pts',(0.6717869665382,-0.8126248283907,-2.955555777364));
#39228=CARTESIAN_POINT('Ctrl Pts',(0.212375641378,-0.9737492166778,-2.989355959748));
#39229=CARTESIAN_POINT('Ctrl Pts',(-0.01648200808866,-0.9698599607208,-3.00625605094));
#39230=CARTESIAN_POINT('',(0.3943262306718,-0.8862318115506,-2.831674910819));
#39231=CARTESIAN_POINT('Ctrl Pts',(0.7314756051133,-0.6370584267743,-2.783777619953));
#39232=CARTESIAN_POINT('Ctrl Pts',(0.581149063108,-0.8096645703499,-2.800677711145));
#39233=CARTESIAN_POINT('Ctrl Pts',(0.1538943548793,-1.043059618461,-2.834477893529));
#39234=CARTESIAN_POINT('Ctrl Pts',(-0.5615125076522,-0.8925604006017,-2.885178167105));
#39235=CARTESIAN_POINT('Ctrl Pts',(-1.006929453025,-0.3129622074044,-2.935878440681));
#39236=CARTESIAN_POINT('Ctrl Pts',(-0.9685032921222,0.4169842392488,-2.986578714257));
#39237=CARTESIAN_POINT('Ctrl Pts',(-0.4646479612591,0.9465598083437,-3.037278987833));
#39238=CARTESIAN_POINT('Ctrl Pts',(0.2624928994603,1.021258833059,-3.087979261409));
#39239=CARTESIAN_POINT('Ctrl Pts',(0.8634925163867,0.6051886724552,-3.138679534985));
#39240=CARTESIAN_POINT('Ctrl Pts',(1.049537078319,-0.1017076106887,-3.189379808561));
#39241=CARTESIAN_POINT('Ctrl Pts',(0.7312223812419,-0.7597278225434,-3.240080082137));
#39242=CARTESIAN_POINT('Ctrl Pts',(0.06151577696635,-1.052657753889,-3.290780355713));
#39243=CARTESIAN_POINT('Ctrl Pts',(-0.6377524802956,-0.8397287116657,-3.341480629289));
#39244=CARTESIAN_POINT('Ctrl Pts',(-1.030546188006,-0.2232646198403,-3.392180902865));
#39245=CARTESIAN_POINT('Ctrl Pts',(-0.9281067295174,0.5004901942744,-3.442881176441));
#39246=CARTESIAN_POINT('Ctrl Pts',(-0.3796618039978,0.98373240799,-3.493581450017));
#39247=CARTESIAN_POINT('Ctrl Pts',(0.3512311470232,0.9942380083834,-3.544281723593));
#39248=CARTESIAN_POINT('Ctrl Pts',(0.9133385405055,0.5269584863877,-3.594981997169));
#39249=CARTESIAN_POINT('Ctrl Pts',(1.036537380232,-0.1935530814404,-3.645682270745));
#39250=CARTESIAN_POINT('Ctrl Pts',(0.6616239622285,-0.8210519280471,-3.696382544321));
#39251=CARTESIAN_POINT('Ctrl Pts',(-0.03123554420463,-1.053990928196,-3.747082817897));
#39252=CARTESIAN_POINT('Ctrl Pts',(-0.7090846828299,-0.7804302971197,-3.797783091473));
#39253=CARTESIAN_POINT('Ctrl Pts',(-1.046180290065,-0.1318307096162,-3.848483365049));
#39254=CARTESIAN_POINT('Ctrl Pts',(-0.8805297016293,0.5801206617478,-3.899183638625));
#39255=CARTESIAN_POINT('Ctrl Pts',(-0.2917369744498,1.013292688671,-3.949883912201));
#39256=CARTESIAN_POINT('Ctrl Pts',(0.4372511207908,0.9595227846198,-4.000584185777));
#39257=CARTESIAN_POINT('Ctrl Pts',(0.9561164944406,0.4446503167462,-4.051284459353));
#39258=CARTESIAN_POINT('Ctrl Pts',(1.015515879006,-0.2839007323944,-4.101984732929));
#39259=CARTESIAN_POINT('Ctrl Pts',(0.5869061509895,-0.8760218996147,-4.152685006505));
#39260=CARTESIAN_POINT('Ctrl Pts',(-0.1237481103043,-1.04716803228,-4.203385280081));
#39261=CARTESIAN_POINT('Ctrl Pts',(-0.7749183178661,-0.7150901112928,-4.254085553657));
#39262=CARTESIAN_POINT('Ctrl Pts',(-1.053759562209,-0.03938464199691,-4.304785827233));
#39263=CARTESIAN_POINT('Ctrl Pts',(-0.8259839985102,0.6552917474932,-4.355486100809));
#39264=CARTESIAN_POINT('Ctrl Pts',(-0.4100818097771,0.9083632859827,-4.389286283193));
#39265=CARTESIAN_POINT('Ctrl Pts',(-0.1854114834362,0.9521147944497,-4.406186374385));
#39266=CARTESIAN_POINT('Ctrl Pts',(0.7314756051133,-0.6370584267743,-2.837136984712));
#39267=CARTESIAN_POINT('Ctrl Pts',(0.581149063108,-0.8096645703499,-2.854037075904));
#39268=CARTESIAN_POINT('Ctrl Pts',(0.1538943548793,-1.043059618461,-2.887837258288));
#39269=CARTESIAN_POINT('Ctrl Pts',(-0.5615125076522,-0.8925604006017,-2.938537531864));
#39270=CARTESIAN_POINT('Ctrl Pts',(-1.006929453025,-0.3129622074044,-2.98923780544));
#39271=CARTESIAN_POINT('Ctrl Pts',(-0.9685032921222,0.4169842392488,-3.039938079016));
#39272=CARTESIAN_POINT('Ctrl Pts',(-0.4646479612591,0.9465598083437,-3.090638352592));
#39273=CARTESIAN_POINT('Ctrl Pts',(0.2624928994603,1.021258833059,-3.141338626168));
#39274=CARTESIAN_POINT('Ctrl Pts',(0.8634925163867,0.6051886724552,-3.192038899744));
#39275=CARTESIAN_POINT('Ctrl Pts',(1.049537078319,-0.1017076106887,-3.24273917332));
#39276=CARTESIAN_POINT('Ctrl Pts',(0.7312223812419,-0.7597278225434,-3.293439446896));
#39277=CARTESIAN_POINT('Ctrl Pts',(0.06151577696635,-1.052657753889,-3.344139720472));
#39278=CARTESIAN_POINT('Ctrl Pts',(-0.6377524802956,-0.8397287116657,-3.394839994048));
#39279=CARTESIAN_POINT('Ctrl Pts',(-1.030546188006,-0.2232646198403,-3.445540267624));
#39280=CARTESIAN_POINT('Ctrl Pts',(-0.9281067295174,0.5004901942744,-3.4962405412));
#39281=CARTESIAN_POINT('Ctrl Pts',(-0.3796618039978,0.98373240799,-3.546940814776));
#39282=CARTESIAN_POINT('Ctrl Pts',(0.3512311470232,0.9942380083834,-3.597641088352));
#39283=CARTESIAN_POINT('Ctrl Pts',(0.9133385405055,0.5269584863877,-3.648341361928));
#39284=CARTESIAN_POINT('Ctrl Pts',(1.036537380232,-0.1935530814404,-3.699041635504));
#39285=CARTESIAN_POINT('Ctrl Pts',(0.6616239622285,-0.8210519280471,-3.74974190908));
#39286=CARTESIAN_POINT('Ctrl Pts',(-0.03123554420463,-1.053990928196,-3.800442182656));
#39287=CARTESIAN_POINT('Ctrl Pts',(-0.7090846828299,-0.7804302971197,-3.851142456232));
#39288=CARTESIAN_POINT('Ctrl Pts',(-1.046180290065,-0.1318307096162,-3.901842729808));
#39289=CARTESIAN_POINT('Ctrl Pts',(-0.8805297016293,0.5801206617478,-3.952543003384));
#39290=CARTESIAN_POINT('Ctrl Pts',(-0.2917369744498,1.013292688671,-4.00324327696));
#39291=CARTESIAN_POINT('Ctrl Pts',(0.4372511207908,0.9595227846198,-4.053943550536));
#39292=CARTESIAN_POINT('Ctrl Pts',(0.9561164944406,0.4446503167462,-4.104643824112));
#39293=CARTESIAN_POINT('Ctrl Pts',(1.015515879006,-0.2839007323944,-4.155344097688));
#39294=CARTESIAN_POINT('Ctrl Pts',(0.5869061509895,-0.8760218996147,-4.206044371264));
#39295=CARTESIAN_POINT('Ctrl Pts',(-0.1237481103043,-1.04716803228,-4.25674464484));
#39296=CARTESIAN_POINT('Ctrl Pts',(-0.7749183178661,-0.7150901112928,-4.307444918416));
#39297=CARTESIAN_POINT('Ctrl Pts',(-1.053759562209,-0.03938464199691,-4.358145191992));
#39298=CARTESIAN_POINT('Ctrl Pts',(-0.8259839985102,0.6552917474932,-4.408845465568));
#39299=CARTESIAN_POINT('Ctrl Pts',(-0.4100818097771,0.9083632859827,-4.442645647952));
#39300=CARTESIAN_POINT('Ctrl Pts',(-0.1854114834362,0.9521147944497,-4.459545739144));
#39301=CARTESIAN_POINT('Ctrl Pts',(0.7314756051133,-0.6370584267743,-2.890496349471));
#39302=CARTESIAN_POINT('Ctrl Pts',(0.581149063108,-0.8096645703499,-2.907396440663));
#39303=CARTESIAN_POINT('Ctrl Pts',(0.1538943548793,-1.043059618461,-2.941196623047));
#39304=CARTESIAN_POINT('Ctrl Pts',(-0.5615125076522,-0.8925604006017,-2.991896896623));
#39305=CARTESIAN_POINT('Ctrl Pts',(-1.006929453025,-0.3129622074044,-3.042597170199));
#39306=CARTESIAN_POINT('Ctrl Pts',(-0.9685032921222,0.4169842392488,-3.093297443775));
#39307=CARTESIAN_POINT('Ctrl Pts',(-0.4646479612591,0.9465598083437,-3.143997717351));
#39308=CARTESIAN_POINT('Ctrl Pts',(0.2624928994603,1.021258833059,-3.194697990927));
#39309=CARTESIAN_POINT('Ctrl Pts',(0.8634925163867,0.6051886724552,-3.245398264503));
#39310=CARTESIAN_POINT('Ctrl Pts',(1.049537078319,-0.1017076106887,-3.29609853808));
#39311=CARTESIAN_POINT('Ctrl Pts',(0.7312223812419,-0.7597278225434,-3.346798811656));
#39312=CARTESIAN_POINT('Ctrl Pts',(0.06151577696635,-1.052657753889,-3.397499085232));
#39313=CARTESIAN_POINT('Ctrl Pts',(-0.6377524802956,-0.8397287116657,-3.448199358808));
#39314=CARTESIAN_POINT('Ctrl Pts',(-1.030546188006,-0.2232646198403,-3.498899632384));
#39315=CARTESIAN_POINT('Ctrl Pts',(-0.9281067295174,0.5004901942744,-3.54959990596));
#39316=CARTESIAN_POINT('Ctrl Pts',(-0.3796618039978,0.98373240799,-3.600300179536));
#39317=CARTESIAN_POINT('Ctrl Pts',(0.3512311470232,0.9942380083834,-3.651000453112));
#39318=CARTESIAN_POINT('Ctrl Pts',(0.9133385405055,0.5269584863877,-3.701700726688));
#39319=CARTESIAN_POINT('Ctrl Pts',(1.036537380232,-0.1935530814404,-3.752401000264));
#39320=CARTESIAN_POINT('Ctrl Pts',(0.6616239622285,-0.8210519280471,-3.80310127384));
#39321=CARTESIAN_POINT('Ctrl Pts',(-0.03123554420463,-1.053990928196,-3.853801547416));
#39322=CARTESIAN_POINT('Ctrl Pts',(-0.7090846828299,-0.7804302971197,-3.904501820992));
#39323=CARTESIAN_POINT('Ctrl Pts',(-1.046180290065,-0.1318307096162,-3.955202094568));
#39324=CARTESIAN_POINT('Ctrl Pts',(-0.8805297016293,0.5801206617478,-4.005902368144));
#39325=CARTESIAN_POINT('Ctrl Pts',(-0.2917369744498,1.013292688671,-4.05660264172));
#39326=CARTESIAN_POINT('Ctrl Pts',(0.4372511207908,0.9595227846198,-4.107302915296));
#39327=CARTESIAN_POINT('Ctrl Pts',(0.9561164944406,0.4446503167462,-4.158003188872));
#39328=CARTESIAN_POINT('Ctrl Pts',(1.015515879006,-0.2839007323944,-4.208703462448));
#39329=CARTESIAN_POINT('Ctrl Pts',(0.5869061509895,-0.8760218996147,-4.259403736024));
#39330=CARTESIAN_POINT('Ctrl Pts',(-0.1237481103043,-1.04716803228,-4.3101040096));
#39331=CARTESIAN_POINT('Ctrl Pts',(-0.7749183178661,-0.7150901112928,-4.360804283176));
#39332=CARTESIAN_POINT('Ctrl Pts',(-1.053759562209,-0.03938464199691,-4.411504556752));
#39333=CARTESIAN_POINT('Ctrl Pts',(-0.8259839985102,0.6552917474932,-4.462204830328));
#39334=CARTESIAN_POINT('Ctrl Pts',(-0.4100818097771,0.9083632859827,-4.496005012712));
#39335=CARTESIAN_POINT('Ctrl Pts',(-0.1854114834362,0.9521147944497,-4.512905103904));
#39336=CARTESIAN_POINT('Ctrl Pts',(0.7314756051133,-0.6370584267743,-2.943855714231));
#39337=CARTESIAN_POINT('Ctrl Pts',(0.581149063108,-0.8096645703499,-2.960755805423));
#39338=CARTESIAN_POINT('Ctrl Pts',(0.1538943548793,-1.043059618461,-2.994555987807));
#39339=CARTESIAN_POINT('Ctrl Pts',(-0.5615125076522,-0.8925604006017,-3.045256261383));
#39340=CARTESIAN_POINT('Ctrl Pts',(-1.006929453025,-0.3129622074044,-3.095956534959));
#39341=CARTESIAN_POINT('Ctrl Pts',(-0.9685032921222,0.4169842392488,-3.146656808535));
#39342=CARTESIAN_POINT('Ctrl Pts',(-0.4646479612591,0.9465598083437,-3.197357082111));
#39343=CARTESIAN_POINT('Ctrl Pts',(0.2624928994603,1.021258833059,-3.248057355687));
#39344=CARTESIAN_POINT('Ctrl Pts',(0.8634925163867,0.6051886724552,-3.298757629263));
#39345=CARTESIAN_POINT('Ctrl Pts',(1.049537078319,-0.1017076106887,-3.349457902839));
#39346=CARTESIAN_POINT('Ctrl Pts',(0.7312223812419,-0.7597278225434,-3.400158176415));
#39347=CARTESIAN_POINT('Ctrl Pts',(0.06151577696635,-1.052657753889,-3.450858449991));
#39348=CARTESIAN_POINT('Ctrl Pts',(-0.6377524802956,-0.8397287116657,-3.501558723567));
#39349=CARTESIAN_POINT('Ctrl Pts',(-1.030546188006,-0.2232646198403,-3.552258997143));
#39350=CARTESIAN_POINT('Ctrl Pts',(-0.9281067295174,0.5004901942744,-3.602959270719));
#39351=CARTESIAN_POINT('Ctrl Pts',(-0.3796618039978,0.98373240799,-3.653659544295));
#39352=CARTESIAN_POINT('Ctrl Pts',(0.3512311470232,0.9942380083834,-3.704359817871));
#39353=CARTESIAN_POINT('Ctrl Pts',(0.9133385405055,0.5269584863877,-3.755060091447));
#39354=CARTESIAN_POINT('Ctrl Pts',(1.036537380232,-0.1935530814404,-3.805760365023));
#39355=CARTESIAN_POINT('Ctrl Pts',(0.6616239622285,-0.8210519280471,-3.856460638599));
#39356=CARTESIAN_POINT('Ctrl Pts',(-0.03123554420463,-1.053990928196,-3.907160912175));
#39357=CARTESIAN_POINT('Ctrl Pts',(-0.7090846828299,-0.7804302971197,-3.957861185751));
#39358=CARTESIAN_POINT('Ctrl Pts',(-1.046180290065,-0.1318307096162,-4.008561459327));
#39359=CARTESIAN_POINT('Ctrl Pts',(-0.8805297016293,0.5801206617478,-4.059261732903));
#39360=CARTESIAN_POINT('Ctrl Pts',(-0.2917369744498,1.013292688671,-4.109962006479));
#39361=CARTESIAN_POINT('Ctrl Pts',(0.4372511207908,0.9595227846198,-4.160662280055));
#39362=CARTESIAN_POINT('Ctrl Pts',(0.9561164944406,0.4446503167462,-4.211362553631));
#39363=CARTESIAN_POINT('Ctrl Pts',(1.015515879006,-0.2839007323944,-4.262062827207));
#39364=CARTESIAN_POINT('Ctrl Pts',(0.5869061509895,-0.8760218996147,-4.312763100783));
#39365=CARTESIAN_POINT('Ctrl Pts',(-0.1237481103043,-1.04716803228,-4.363463374359));
#39366=CARTESIAN_POINT('Ctrl Pts',(-0.7749183178661,-0.7150901112928,-4.414163647935));
#39367=CARTESIAN_POINT('Ctrl Pts',(-1.053759562209,-0.03938464199691,-4.464863921511));
#39368=CARTESIAN_POINT('Ctrl Pts',(-0.8259839985102,0.6552917474932,-4.515564195087));
#39369=CARTESIAN_POINT('Ctrl Pts',(-0.4100818097771,0.9083632859827,-4.549364377471));
#39370=CARTESIAN_POINT('Ctrl Pts',(-0.1854114834362,0.9521147944497,-4.566264468663));
#39371=CARTESIAN_POINT('',(-0.5698749570781,0.784947471679,-4.391683328543));
#39372=CARTESIAN_POINT('Ctrl Pts',(-0.8478876321751,0.4711545003548,-4.343786037676));
#39373=CARTESIAN_POINT('Ctrl Pts',(-0.7367094045404,0.6712303652943,-4.360686128868));
#39374=CARTESIAN_POINT('Ctrl Pts',(-0.3672795254541,0.9883130021961,-4.394486311252));
#39375=CARTESIAN_POINT('Ctrl Pts',(0.3637847024261,0.9897580791551,-4.445186584828));
#39376=CARTESIAN_POINT('Ctrl Pts',(0.9199177062286,0.5153675197374,-4.495886858404));
#39377=CARTESIAN_POINT('Ctrl Pts',(1.034010790836,-0.2066305085619,-4.54658713198));
#39378=CARTESIAN_POINT('Ctrl Pts',(0.6511976671912,-0.8293460055482,-4.597287405556));
#39379=CARTESIAN_POINT('Ctrl Pts',(-0.04454897242399,-1.053511991116,-4.647987679132));
#39380=CARTESIAN_POINT('Ctrl Pts',(-0.7188880044982,-0.771409548886,-4.698687952708));
#39381=CARTESIAN_POINT('Ctrl Pts',(-1.047762323398,-0.1186028267124,-4.749388226284));
#39382=CARTESIAN_POINT('Ctrl Pts',(-0.8731302342653,0.5911988913957,-4.80008849986));
#39383=CARTESIAN_POINT('Ctrl Pts',(-0.2789118454146,1.016897595693,-4.850788773436));
#39384=CARTESIAN_POINT('Ctrl Pts',(0.4493387631725,0.9539220152767,-4.901489047012));
#39385=CARTESIAN_POINT('Ctrl Pts',(0.9616578007037,0.4325353285362,-4.952189320588));
#39386=CARTESIAN_POINT('Ctrl Pts',(1.011848267068,-0.2967079715329,-5.002889594164));
#39387=CARTESIAN_POINT('Ctrl Pts',(0.5757909296073,-0.8833670479063,-5.05358986774));
#39388=CARTESIAN_POINT('Ctrl Pts',(-0.1369650830855,-1.045520493328,-5.104290141316));
#39389=CARTESIAN_POINT('Ctrl Pts',(-0.7839019675243,-0.7052448094529,-5.154990414892));
#39390=CARTESIAN_POINT('Ctrl Pts',(-1.054131570278,-0.02606086140956,-5.205690688468));
#39391=CARTESIAN_POINT('Ctrl Pts',(-0.8177939556507,0.6656467396795,-5.256390962044));
#39392=CARTESIAN_POINT('Ctrl Pts',(-0.1884621264991,1.037475090215,-5.30709123562));
#39393=CARTESIAN_POINT('Ctrl Pts',(0.5314359448635,0.9107405627254,-5.357791509196));
#39394=CARTESIAN_POINT('Ctrl Pts',(0.9959503090853,0.3463459501016,-5.408491782772));
#39395=CARTESIAN_POINT('Ctrl Pts',(0.9818566993762,-0.3844866181393,-5.459192056348));
#39396=CARTESIAN_POINT('Ctrl Pts',(0.4959278500411,-0.9305525792395,-5.509892329924));
#39397=CARTESIAN_POINT('Ctrl Pts',(-0.228321125274,-1.02943770117,-5.5605926035));
#39398=CARTESIAN_POINT('Ctrl Pts',(-0.8428495336144,-0.6336223787161,-5.611292877076));
#39399=CARTESIAN_POINT('Ctrl Pts',(-1.052342871644,0.06668288287484,-5.661993150652));
#39400=CARTESIAN_POINT('Ctrl Pts',(-0.7561296625306,0.7349429448028,-5.712693424228));
#39401=CARTESIAN_POINT('Ctrl Pts',(-0.09655114644213,1.050024932444,-5.763393697804));
#39402=CARTESIAN_POINT('Ctrl Pts',(0.6094100419002,0.860506634178,-5.81409397138));
#39403=CARTESIAN_POINT('Ctrl Pts',(1.022574131124,0.2574927403421,-5.864794244956));
#39404=CARTESIAN_POINT('Ctrl Pts',(0.9441219235678,-0.4693512901507,-5.915494518532));
#39405=CARTESIAN_POINT('Ctrl Pts',(0.5898854717729,-0.8033219032384,-5.949294700916));
#39406=CARTESIAN_POINT('Ctrl Pts',(0.3792106625816,-0.892804162952,-5.966194792108));
#39407=CARTESIAN_POINT('Ctrl Pts',(-0.8478876321751,0.4711545003548,-4.397145402435));
#39408=CARTESIAN_POINT('Ctrl Pts',(-0.7367094045404,0.6712303652943,-4.414045493627));
#39409=CARTESIAN_POINT('Ctrl Pts',(-0.3672795254541,0.9883130021961,-4.447845676011));
#39410=CARTESIAN_POINT('Ctrl Pts',(0.3637847024261,0.9897580791551,-4.498545949587));
#39411=CARTESIAN_POINT('Ctrl Pts',(0.9199177062286,0.5153675197374,-4.549246223163));
#39412=CARTESIAN_POINT('Ctrl Pts',(1.034010790836,-0.2066305085619,-4.599946496739));
#39413=CARTESIAN_POINT('Ctrl Pts',(0.6511976671912,-0.8293460055482,-4.650646770315));
#39414=CARTESIAN_POINT('Ctrl Pts',(-0.04454897242399,-1.053511991116,-4.701347043891));
#39415=CARTESIAN_POINT('Ctrl Pts',(-0.7188880044982,-0.771409548886,-4.752047317467));
#39416=CARTESIAN_POINT('Ctrl Pts',(-1.047762323398,-0.1186028267124,-4.802747591043));
#39417=CARTESIAN_POINT('Ctrl Pts',(-0.8731302342653,0.5911988913957,-4.853447864619));
#39418=CARTESIAN_POINT('Ctrl Pts',(-0.2789118454146,1.016897595693,-4.904148138195));
#39419=CARTESIAN_POINT('Ctrl Pts',(0.4493387631725,0.9539220152767,-4.954848411771));
#39420=CARTESIAN_POINT('Ctrl Pts',(0.9616578007037,0.4325353285362,-5.005548685347));
#39421=CARTESIAN_POINT('Ctrl Pts',(1.011848267068,-0.2967079715329,-5.056248958923));
#39422=CARTESIAN_POINT('Ctrl Pts',(0.5757909296073,-0.8833670479063,-5.106949232499));
#39423=CARTESIAN_POINT('Ctrl Pts',(-0.1369650830855,-1.045520493328,-5.157649506075));
#39424=CARTESIAN_POINT('Ctrl Pts',(-0.7839019675243,-0.7052448094529,-5.208349779651));
#39425=CARTESIAN_POINT('Ctrl Pts',(-1.054131570278,-0.02606086140956,-5.259050053227));
#39426=CARTESIAN_POINT('Ctrl Pts',(-0.8177939556507,0.6656467396795,-5.309750326803));
#39427=CARTESIAN_POINT('Ctrl Pts',(-0.1884621264991,1.037475090215,-5.360450600379));
#39428=CARTESIAN_POINT('Ctrl Pts',(0.5314359448635,0.9107405627254,-5.411150873955));
#39429=CARTESIAN_POINT('Ctrl Pts',(0.9959503090853,0.3463459501016,-5.461851147531));
#39430=CARTESIAN_POINT('Ctrl Pts',(0.9818566993762,-0.3844866181393,-5.512551421107));
#39431=CARTESIAN_POINT('Ctrl Pts',(0.4959278500411,-0.9305525792395,-5.563251694683));
#39432=CARTESIAN_POINT('Ctrl Pts',(-0.228321125274,-1.02943770117,-5.613951968259));
#39433=CARTESIAN_POINT('Ctrl Pts',(-0.8428495336144,-0.6336223787161,-5.664652241835));
#39434=CARTESIAN_POINT('Ctrl Pts',(-1.052342871644,0.06668288287484,-5.715352515411));
#39435=CARTESIAN_POINT('Ctrl Pts',(-0.7561296625306,0.7349429448028,-5.766052788987));
#39436=CARTESIAN_POINT('Ctrl Pts',(-0.09655114644213,1.050024932444,-5.816753062563));
#39437=CARTESIAN_POINT('Ctrl Pts',(0.6094100419002,0.860506634178,-5.867453336139));
#39438=CARTESIAN_POINT('Ctrl Pts',(1.022574131124,0.2574927403421,-5.918153609715));
#39439=CARTESIAN_POINT('Ctrl Pts',(0.9441219235678,-0.4693512901507,-5.968853883291));
#39440=CARTESIAN_POINT('Ctrl Pts',(0.5898854717729,-0.8033219032384,-6.002654065675));
#39441=CARTESIAN_POINT('Ctrl Pts',(0.3792106625816,-0.892804162952,-6.019554156867));
#39442=CARTESIAN_POINT('Ctrl Pts',(-0.8478876321751,0.4711545003548,-4.450504767195));
#39443=CARTESIAN_POINT('Ctrl Pts',(-0.7367094045404,0.6712303652943,-4.467404858387));
#39444=CARTESIAN_POINT('Ctrl Pts',(-0.3672795254541,0.9883130021961,-4.501205040771));
#39445=CARTESIAN_POINT('Ctrl Pts',(0.3637847024261,0.9897580791551,-4.551905314347));
#39446=CARTESIAN_POINT('Ctrl Pts',(0.9199177062286,0.5153675197374,-4.602605587923));
#39447=CARTESIAN_POINT('Ctrl Pts',(1.034010790836,-0.2066305085619,-4.653305861499));
#39448=CARTESIAN_POINT('Ctrl Pts',(0.6511976671912,-0.8293460055482,-4.704006135075));
#39449=CARTESIAN_POINT('Ctrl Pts',(-0.04454897242399,-1.053511991116,-4.754706408651));
#39450=CARTESIAN_POINT('Ctrl Pts',(-0.7188880044982,-0.771409548886,-4.805406682227));
#39451=CARTESIAN_POINT('Ctrl Pts',(-1.047762323398,-0.1186028267124,-4.856106955803));
#39452=CARTESIAN_POINT('Ctrl Pts',(-0.8731302342653,0.5911988913957,-4.906807229379));
#39453=CARTESIAN_POINT('Ctrl Pts',(-0.2789118454146,1.016897595693,-4.957507502955));
#39454=CARTESIAN_POINT('Ctrl Pts',(0.4493387631725,0.9539220152767,-5.008207776531));
#39455=CARTESIAN_POINT('Ctrl Pts',(0.9616578007037,0.4325353285362,-5.058908050107));
#39456=CARTESIAN_POINT('Ctrl Pts',(1.011848267068,-0.2967079715329,-5.109608323683));
#39457=CARTESIAN_POINT('Ctrl Pts',(0.5757909296073,-0.8833670479063,-5.160308597259));
#39458=CARTESIAN_POINT('Ctrl Pts',(-0.1369650830855,-1.045520493328,-5.211008870835));
#39459=CARTESIAN_POINT('Ctrl Pts',(-0.7839019675243,-0.7052448094529,-5.261709144411));
#39460=CARTESIAN_POINT('Ctrl Pts',(-1.054131570278,-0.02606086140956,-5.312409417987));
#39461=CARTESIAN_POINT('Ctrl Pts',(-0.8177939556507,0.6656467396795,-5.363109691563));
#39462=CARTESIAN_POINT('Ctrl Pts',(-0.1884621264991,1.037475090215,-5.413809965139));
#39463=CARTESIAN_POINT('Ctrl Pts',(0.5314359448635,0.9107405627254,-5.464510238715));
#39464=CARTESIAN_POINT('Ctrl Pts',(0.9959503090853,0.3463459501016,-5.515210512291));
#39465=CARTESIAN_POINT('Ctrl Pts',(0.9818566993762,-0.3844866181393,-5.565910785867));
#39466=CARTESIAN_POINT('Ctrl Pts',(0.4959278500411,-0.9305525792395,-5.616611059443));
#39467=CARTESIAN_POINT('Ctrl Pts',(-0.228321125274,-1.02943770117,-5.667311333019));
#39468=CARTESIAN_POINT('Ctrl Pts',(-0.8428495336144,-0.6336223787161,-5.718011606595));
#39469=CARTESIAN_POINT('Ctrl Pts',(-1.052342871644,0.06668288287484,-5.768711880171));
#39470=CARTESIAN_POINT('Ctrl Pts',(-0.7561296625306,0.7349429448028,-5.819412153747));
#39471=CARTESIAN_POINT('Ctrl Pts',(-0.09655114644213,1.050024932444,-5.870112427323));
#39472=CARTESIAN_POINT('Ctrl Pts',(0.6094100419002,0.860506634178,-5.920812700899));
#39473=CARTESIAN_POINT('Ctrl Pts',(1.022574131124,0.2574927403421,-5.971512974475));
#39474=CARTESIAN_POINT('Ctrl Pts',(0.9441219235678,-0.4693512901507,-6.022213248051));
#39475=CARTESIAN_POINT('Ctrl Pts',(0.5898854717729,-0.8033219032384,-6.056013430435));
#39476=CARTESIAN_POINT('Ctrl Pts',(0.3792106625816,-0.892804162952,-6.072913521627));
#39477=CARTESIAN_POINT('Ctrl Pts',(-0.8478876321751,0.4711545003548,-4.503864131954));
#39478=CARTESIAN_POINT('Ctrl Pts',(-0.7367094045404,0.6712303652943,-4.520764223146));
#39479=CARTESIAN_POINT('Ctrl Pts',(-0.3672795254541,0.9883130021961,-4.55456440553));
#39480=CARTESIAN_POINT('Ctrl Pts',(0.3637847024261,0.9897580791551,-4.605264679106));
#39481=CARTESIAN_POINT('Ctrl Pts',(0.9199177062286,0.5153675197374,-4.655964952682));
#39482=CARTESIAN_POINT('Ctrl Pts',(1.034010790836,-0.2066305085619,-4.706665226258));
#39483=CARTESIAN_POINT('Ctrl Pts',(0.6511976671912,-0.8293460055482,-4.757365499834));
#39484=CARTESIAN_POINT('Ctrl Pts',(-0.04454897242399,-1.053511991116,-4.80806577341));
#39485=CARTESIAN_POINT('Ctrl Pts',(-0.7188880044982,-0.771409548886,-4.858766046986));
#39486=CARTESIAN_POINT('Ctrl Pts',(-1.047762323398,-0.1186028267124,-4.909466320562));
#39487=CARTESIAN_POINT('Ctrl Pts',(-0.8731302342653,0.5911988913957,-4.960166594138));
#39488=CARTESIAN_POINT('Ctrl Pts',(-0.2789118454146,1.016897595693,-5.010866867714));
#39489=CARTESIAN_POINT('Ctrl Pts',(0.4493387631725,0.9539220152767,-5.06156714129));
#39490=CARTESIAN_POINT('Ctrl Pts',(0.9616578007037,0.4325353285362,-5.112267414866));
#39491=CARTESIAN_POINT('Ctrl Pts',(1.011848267068,-0.2967079715329,-5.162967688442));
#39492=CARTESIAN_POINT('Ctrl Pts',(0.5757909296073,-0.8833670479063,-5.213667962018));
#39493=CARTESIAN_POINT('Ctrl Pts',(-0.1369650830855,-1.045520493328,-5.264368235594));
#39494=CARTESIAN_POINT('Ctrl Pts',(-0.7839019675243,-0.7052448094529,-5.31506850917));
#39495=CARTESIAN_POINT('Ctrl Pts',(-1.054131570278,-0.02606086140956,-5.365768782746));
#39496=CARTESIAN_POINT('Ctrl Pts',(-0.8177939556507,0.6656467396795,-5.416469056322));
#39497=CARTESIAN_POINT('Ctrl Pts',(-0.1884621264991,1.037475090215,-5.467169329898));
#39498=CARTESIAN_POINT('Ctrl Pts',(0.5314359448635,0.9107405627254,-5.517869603474));
#39499=CARTESIAN_POINT('Ctrl Pts',(0.9959503090853,0.3463459501016,-5.56856987705));
#39500=CARTESIAN_POINT('Ctrl Pts',(0.9818566993762,-0.3844866181393,-5.619270150626));
#39501=CARTESIAN_POINT('Ctrl Pts',(0.4959278500411,-0.9305525792395,-5.669970424202));
#39502=CARTESIAN_POINT('Ctrl Pts',(-0.228321125274,-1.02943770117,-5.720670697778));
#39503=CARTESIAN_POINT('Ctrl Pts',(-0.8428495336144,-0.6336223787161,-5.771370971354));
#39504=CARTESIAN_POINT('Ctrl Pts',(-1.052342871644,0.06668288287484,-5.82207124493));
#39505=CARTESIAN_POINT('Ctrl Pts',(-0.7561296625306,0.7349429448028,-5.872771518506));
#39506=CARTESIAN_POINT('Ctrl Pts',(-0.09655114644213,1.050024932444,-5.923471792082));
#39507=CARTESIAN_POINT('Ctrl Pts',(0.6094100419002,0.860506634178,-5.974172065658));
#39508=CARTESIAN_POINT('Ctrl Pts',(1.022574131124,0.2574927403421,-6.024872339234));
#39509=CARTESIAN_POINT('Ctrl Pts',(0.9441219235678,-0.4693512901507,-6.07557261281));
#39510=CARTESIAN_POINT('Ctrl Pts',(0.5898854717729,-0.8033219032384,-6.109372795194));
#39511=CARTESIAN_POINT('Ctrl Pts',(0.3792106625816,-0.892804162952,-6.126272886386));
#39512=CARTESIAN_POINT('',(0.7205452572168,-0.6493955129983,-5.951691746266));
#39513=CARTESIAN_POINT('Ctrl Pts',(0.9272843286311,-0.2846818818877,-5.903794455399));
#39514=CARTESIAN_POINT('Ctrl Pts',(0.8601080052719,-0.5034929684698,-5.920694546591));
#39515=CARTESIAN_POINT('Ctrl Pts',(0.5646307635317,-0.8904206539615,-5.954494728975));
#39516=CARTESIAN_POINT('Ctrl Pts',(-0.1501755344832,-1.043746939548,-6.005195002551));
#39517=CARTESIAN_POINT('Ctrl Pts',(-0.7927460883193,-0.6952739791533,-6.055895276127));
#39518=CARTESIAN_POINT('Ctrl Pts',(-1.054377577714,-0.01274387096732,-6.106595549703));
#39519=CARTESIAN_POINT('Ctrl Pts',(-0.8093187275974,0.6759263242647,-6.157295823279));
#39520=CARTESIAN_POINT('Ctrl Pts',(-0.1753397818274,1.03977309413,-6.207996096855));
#39521=CARTESIAN_POINT('Ctrl Pts',(0.542899761859,0.903953817237,-6.258696370431));
#39522=CARTESIAN_POINT('Ctrl Pts',(1.000246520579,0.3337355463655,-6.309396644007));
#39523=CARTESIAN_POINT('Ctrl Pts',(0.9769207671901,-0.3968606176082,-6.360096917583));
#39524=CARTESIAN_POINT('Ctrl Pts',(0.4841317554003,-0.9367438182615,-6.410797191159));
#39525=CARTESIAN_POINT('Ctrl Pts',(-0.2413087404899,-1.026470957739,-6.461497464735));
#39526=CARTESIAN_POINT('Ctrl Pts',(-0.8507873392775,-0.6229233013874,-6.512197738311));
#39527=CARTESIAN_POINT('Ctrl Pts',(-1.051416618566,0.07997268373542,-6.562898011887));
#39528=CARTESIAN_POINT('Ctrl Pts',(-0.7467833616144,0.7444374700139,-6.613598285463));
#39529=CARTESIAN_POINT('Ctrl Pts',(-0.08328032014135,1.051159799569,-6.664298559039));
#39530=CARTESIAN_POINT('Ctrl Pts',(0.6202434181993,0.8527430082558,-6.714998832615));
#39531=CARTESIAN_POINT('Ctrl Pts',(1.025706656971,0.2445370928879,-6.765699106191));
#39532=CARTESIAN_POINT('Ctrl Pts',(0.9382623861687,-0.4811821179614,-6.816399379767));
#39533=CARTESIAN_POINT('Ctrl Pts',(0.3999323061365,-0.9756673031565,-6.867099653343));
#39534=CARTESIAN_POINT('Ctrl Pts',(-0.3305868717956,-1.001291594034,-6.917799926919));
#39535=CARTESIAN_POINT('Ctrl Pts',(-0.9022411823332,-0.545741132975,-6.968500200495));
#39536=CARTESIAN_POINT('Ctrl Pts',(-1.040319821114,0.172067450248,-7.019200474071));
#39537=CARTESIAN_POINT('Ctrl Pts',(-0.6784685297463,0.8071883233295,-7.069900747647));
#39538=CARTESIAN_POINT('Ctrl Pts',(0.009423556678434,1.054411548408,-7.120601021223));
#39539=CARTESIAN_POINT('Ctrl Pts',(0.6927871851051,0.7949330608788,-7.171301294799));
#39540=CARTESIAN_POINT('Ctrl Pts',(1.043228848248,0.1534460705006,-7.222001568375));
#39541=CARTESIAN_POINT('Ctrl Pts',(0.8923436237759,-0.5617793657482,-7.272701841951));
#39542=CARTESIAN_POINT('Ctrl Pts',(0.3126353722454,-1.007042008386,-7.323402115527));
#39543=CARTESIAN_POINT('Ctrl Pts',(-0.4172973984221,-0.9683569320779,-7.374102389103));
#39544=CARTESIAN_POINT('Ctrl Pts',(-0.9467472663198,-0.4643597513654,-7.424802662679));
#39545=CARTESIAN_POINT('Ctrl Pts',(-1.021043319681,0.2629208615952,-7.475502936255));
#39546=CARTESIAN_POINT('Ctrl Pts',(-0.7439371296958,0.6632107486247,-7.509303118639));
#39547=CARTESIAN_POINT('Ctrl Pts',(-0.5564550442372,0.7945173275284,-7.526203209831));
#39548=CARTESIAN_POINT('Ctrl Pts',(0.9272843286311,-0.2846818818877,-5.957153820158));
#39549=CARTESIAN_POINT('Ctrl Pts',(0.8601080052719,-0.5034929684698,-5.97405391135));
#39550=CARTESIAN_POINT('Ctrl Pts',(0.5646307635317,-0.8904206539615,-6.007854093734));
#39551=CARTESIAN_POINT('Ctrl Pts',(-0.1501755344832,-1.043746939548,-6.05855436731));
#39552=CARTESIAN_POINT('Ctrl Pts',(-0.7927460883193,-0.6952739791533,-6.109254640886));
#39553=CARTESIAN_POINT('Ctrl Pts',(-1.054377577714,-0.01274387096732,-6.159954914462));
#39554=CARTESIAN_POINT('Ctrl Pts',(-0.8093187275974,0.6759263242647,-6.210655188038));
#39555=CARTESIAN_POINT('Ctrl Pts',(-0.1753397818274,1.03977309413,-6.261355461614));
#39556=CARTESIAN_POINT('Ctrl Pts',(0.542899761859,0.903953817237,-6.31205573519));
#39557=CARTESIAN_POINT('Ctrl Pts',(1.000246520579,0.3337355463655,-6.362756008766));
#39558=CARTESIAN_POINT('Ctrl Pts',(0.9769207671901,-0.3968606176082,-6.413456282342));
#39559=CARTESIAN_POINT('Ctrl Pts',(0.4841317554003,-0.9367438182615,-6.464156555918));
#39560=CARTESIAN_POINT('Ctrl Pts',(-0.2413087404899,-1.026470957739,-6.514856829494));
#39561=CARTESIAN_POINT('Ctrl Pts',(-0.8507873392775,-0.6229233013874,-6.56555710307));
#39562=CARTESIAN_POINT('Ctrl Pts',(-1.051416618566,0.07997268373542,-6.616257376646));
#39563=CARTESIAN_POINT('Ctrl Pts',(-0.7467833616144,0.7444374700139,-6.666957650222));
#39564=CARTESIAN_POINT('Ctrl Pts',(-0.08328032014135,1.051159799569,-6.717657923798));
#39565=CARTESIAN_POINT('Ctrl Pts',(0.6202434181993,0.8527430082558,-6.768358197374));
#39566=CARTESIAN_POINT('Ctrl Pts',(1.025706656971,0.2445370928879,-6.81905847095));
#39567=CARTESIAN_POINT('Ctrl Pts',(0.9382623861687,-0.4811821179614,-6.869758744526));
#39568=CARTESIAN_POINT('Ctrl Pts',(0.3999323061365,-0.9756673031565,-6.920459018102));
#39569=CARTESIAN_POINT('Ctrl Pts',(-0.3305868717956,-1.001291594034,-6.971159291678));
#39570=CARTESIAN_POINT('Ctrl Pts',(-0.9022411823332,-0.545741132975,-7.021859565254));
#39571=CARTESIAN_POINT('Ctrl Pts',(-1.040319821114,0.172067450248,-7.07255983883));
#39572=CARTESIAN_POINT('Ctrl Pts',(-0.6784685297463,0.8071883233295,-7.123260112406));
#39573=CARTESIAN_POINT('Ctrl Pts',(0.009423556678434,1.054411548408,-7.173960385982));
#39574=CARTESIAN_POINT('Ctrl Pts',(0.6927871851051,0.7949330608788,-7.224660659558));
#39575=CARTESIAN_POINT('Ctrl Pts',(1.043228848248,0.1534460705006,-7.275360933134));
#39576=CARTESIAN_POINT('Ctrl Pts',(0.8923436237759,-0.5617793657482,-7.32606120671));
#39577=CARTESIAN_POINT('Ctrl Pts',(0.3126353722454,-1.007042008386,-7.376761480286));
#39578=CARTESIAN_POINT('Ctrl Pts',(-0.4172973984221,-0.9683569320779,-7.427461753862));
#39579=CARTESIAN_POINT('Ctrl Pts',(-0.9467472663198,-0.4643597513654,-7.478162027438));
#39580=CARTESIAN_POINT('Ctrl Pts',(-1.021043319681,0.2629208615952,-7.528862301014));
#39581=CARTESIAN_POINT('Ctrl Pts',(-0.7439371296958,0.6632107486247,-7.562662483398));
#39582=CARTESIAN_POINT('Ctrl Pts',(-0.5564550442372,0.7945173275284,-7.57956257459));
#39583=CARTESIAN_POINT('Ctrl Pts',(0.9272843286311,-0.2846818818877,-6.010513184918));
#39584=CARTESIAN_POINT('Ctrl Pts',(0.8601080052719,-0.5034929684698,-6.02741327611));
#39585=CARTESIAN_POINT('Ctrl Pts',(0.5646307635317,-0.8904206539615,-6.061213458494));
#39586=CARTESIAN_POINT('Ctrl Pts',(-0.1501755344832,-1.043746939548,-6.11191373207));
#39587=CARTESIAN_POINT('Ctrl Pts',(-0.7927460883193,-0.6952739791533,-6.162614005646));
#39588=CARTESIAN_POINT('Ctrl Pts',(-1.054377577714,-0.01274387096732,-6.213314279222));
#39589=CARTESIAN_POINT('Ctrl Pts',(-0.8093187275974,0.6759263242647,-6.264014552798));
#39590=CARTESIAN_POINT('Ctrl Pts',(-0.1753397818274,1.03977309413,-6.314714826374));
#39591=CARTESIAN_POINT('Ctrl Pts',(0.542899761859,0.903953817237,-6.36541509995));
#39592=CARTESIAN_POINT('Ctrl Pts',(1.000246520579,0.3337355463655,-6.416115373526));
#39593=CARTESIAN_POINT('Ctrl Pts',(0.9769207671901,-0.3968606176082,-6.466815647102));
#39594=CARTESIAN_POINT('Ctrl Pts',(0.4841317554003,-0.9367438182615,-6.517515920678));
#39595=CARTESIAN_POINT('Ctrl Pts',(-0.2413087404899,-1.026470957739,-6.568216194254));
#39596=CARTESIAN_POINT('Ctrl Pts',(-0.8507873392775,-0.6229233013874,-6.61891646783));
#39597=CARTESIAN_POINT('Ctrl Pts',(-1.051416618566,0.07997268373542,-6.669616741406));
#39598=CARTESIAN_POINT('Ctrl Pts',(-0.7467833616144,0.7444374700139,-6.720317014982));
#39599=CARTESIAN_POINT('Ctrl Pts',(-0.08328032014135,1.051159799569,-6.771017288558));
#39600=CARTESIAN_POINT('Ctrl Pts',(0.6202434181993,0.8527430082558,-6.821717562134));
#39601=CARTESIAN_POINT('Ctrl Pts',(1.025706656971,0.2445370928879,-6.87241783571));
#39602=CARTESIAN_POINT('Ctrl Pts',(0.9382623861687,-0.4811821179614,-6.923118109286));
#39603=CARTESIAN_POINT('Ctrl Pts',(0.3999323061365,-0.9756673031565,-6.973818382862));
#39604=CARTESIAN_POINT('Ctrl Pts',(-0.3305868717956,-1.001291594034,-7.024518656438));
#39605=CARTESIAN_POINT('Ctrl Pts',(-0.9022411823332,-0.545741132975,-7.075218930014));
#39606=CARTESIAN_POINT('Ctrl Pts',(-1.040319821114,0.172067450248,-7.12591920359));
#39607=CARTESIAN_POINT('Ctrl Pts',(-0.6784685297463,0.8071883233295,-7.176619477166));
#39608=CARTESIAN_POINT('Ctrl Pts',(0.009423556678434,1.054411548408,-7.227319750742));
#39609=CARTESIAN_POINT('Ctrl Pts',(0.6927871851051,0.7949330608788,-7.278020024318));
#39610=CARTESIAN_POINT('Ctrl Pts',(1.043228848248,0.1534460705006,-7.328720297894));
#39611=CARTESIAN_POINT('Ctrl Pts',(0.8923436237759,-0.5617793657482,-7.37942057147));
#39612=CARTESIAN_POINT('Ctrl Pts',(0.3126353722454,-1.007042008386,-7.430120845046));
#39613=CARTESIAN_POINT('Ctrl Pts',(-0.4172973984221,-0.9683569320779,-7.480821118622));
#39614=CARTESIAN_POINT('Ctrl Pts',(-0.9467472663198,-0.4643597513654,-7.531521392198));
#39615=CARTESIAN_POINT('Ctrl Pts',(-1.021043319681,0.2629208615952,-7.582221665774));
#39616=CARTESIAN_POINT('Ctrl Pts',(-0.7439371296958,0.6632107486247,-7.616021848158));
#39617=CARTESIAN_POINT('Ctrl Pts',(-0.5564550442372,0.7945173275284,-7.63292193935));
#39618=CARTESIAN_POINT('Ctrl Pts',(0.9272843286311,-0.2846818818877,-6.063872549677));
#39619=CARTESIAN_POINT('Ctrl Pts',(0.8601080052719,-0.5034929684698,-6.080772640869));
#39620=CARTESIAN_POINT('Ctrl Pts',(0.5646307635317,-0.8904206539615,-6.114572823253));
#39621=CARTESIAN_POINT('Ctrl Pts',(-0.1501755344832,-1.043746939548,-6.165273096829));
#39622=CARTESIAN_POINT('Ctrl Pts',(-0.7927460883193,-0.6952739791533,-6.215973370405));
#39623=CARTESIAN_POINT('Ctrl Pts',(-1.054377577714,-0.01274387096732,-6.266673643981));
#39624=CARTESIAN_POINT('Ctrl Pts',(-0.8093187275974,0.6759263242647,-6.317373917557));
#39625=CARTESIAN_POINT('Ctrl Pts',(-0.1753397818274,1.03977309413,-6.368074191133));
#39626=CARTESIAN_POINT('Ctrl Pts',(0.542899761859,0.903953817237,-6.418774464709));
#39627=CARTESIAN_POINT('Ctrl Pts',(1.000246520579,0.3337355463655,-6.469474738285));
#39628=CARTESIAN_POINT('Ctrl Pts',(0.9769207671901,-0.3968606176082,-6.520175011861));
#39629=CARTESIAN_POINT('Ctrl Pts',(0.4841317554003,-0.9367438182615,-6.570875285437));
#39630=CARTESIAN_POINT('Ctrl Pts',(-0.2413087404899,-1.026470957739,-6.621575559013));
#39631=CARTESIAN_POINT('Ctrl Pts',(-0.8507873392775,-0.6229233013874,-6.672275832589));
#39632=CARTESIAN_POINT('Ctrl Pts',(-1.051416618566,0.07997268373542,-6.722976106165));
#39633=CARTESIAN_POINT('Ctrl Pts',(-0.7467833616144,0.7444374700139,-6.773676379741));
#39634=CARTESIAN_POINT('Ctrl Pts',(-0.08328032014135,1.051159799569,-6.824376653317));
#39635=CARTESIAN_POINT('Ctrl Pts',(0.6202434181993,0.8527430082558,-6.875076926893));
#39636=CARTESIAN_POINT('Ctrl Pts',(1.025706656971,0.2445370928879,-6.925777200469));
#39637=CARTESIAN_POINT('Ctrl Pts',(0.9382623861687,-0.4811821179614,-6.976477474045));
#39638=CARTESIAN_POINT('Ctrl Pts',(0.3999323061365,-0.9756673031565,-7.027177747621));
#39639=CARTESIAN_POINT('Ctrl Pts',(-0.3305868717956,-1.001291594034,-7.077878021197));
#39640=CARTESIAN_POINT('Ctrl Pts',(-0.9022411823332,-0.545741132975,-7.128578294773));
#39641=CARTESIAN_POINT('Ctrl Pts',(-1.040319821114,0.172067450248,-7.179278568349));
#39642=CARTESIAN_POINT('Ctrl Pts',(-0.6784685297463,0.8071883233295,-7.229978841925));
#39643=CARTESIAN_POINT('Ctrl Pts',(0.009423556678434,1.054411548408,-7.280679115501));
#39644=CARTESIAN_POINT('Ctrl Pts',(0.6927871851051,0.7949330608788,-7.331379389077));
#39645=CARTESIAN_POINT('Ctrl Pts',(1.043228848248,0.1534460705006,-7.382079662653));
#39646=CARTESIAN_POINT('Ctrl Pts',(0.8923436237759,-0.5617793657482,-7.432779936229));
#39647=CARTESIAN_POINT('Ctrl Pts',(0.3126353722454,-1.007042008386,-7.483480209805));
#39648=CARTESIAN_POINT('Ctrl Pts',(-0.4172973984221,-0.9683569320779,-7.534180483381));
#39649=CARTESIAN_POINT('Ctrl Pts',(-0.9467472663198,-0.4643597513654,-7.584880756957));
#39650=CARTESIAN_POINT('Ctrl Pts',(-1.021043319681,0.2629208615952,-7.635581030533));
#39651=CARTESIAN_POINT('Ctrl Pts',(-0.7439371296958,0.6632107486247,-7.669381212917));
#39652=CARTESIAN_POINT('Ctrl Pts',(-0.5564550442372,0.7945173275284,-7.686281304109));
#39653=CARTESIAN_POINT('',(-0.8397594776816,0.485493583525,-7.511700163989));
#39654=CARTESIAN_POINT('Ctrl Pts',(-0.9661995571575,0.08578120859872,-7.463802873122));
#39655=CARTESIAN_POINT('Ctrl Pts',(-0.9459577835372,0.313775113412,-7.480702964314));
#39656=CARTESIAN_POINT('Ctrl Pts',(-0.7373325155345,0.7536561561237,-7.514503146698));
#39657=CARTESIAN_POINT('Ctrl Pts',(-0.06998968740697,1.052170047392,-7.565203420274));
#39658=CARTESIAN_POINT('Ctrl Pts',(0.6309663956697,0.8448276002645,-7.61590369385));
#39659=CARTESIAN_POINT('Ctrl Pts',(1.028714521555,0.2315619048451,-7.666603967426));
#39660=CARTESIAN_POINT('Ctrl Pts',(0.932108219137,-0.4929984447149,-7.717304241002));
#39661=CARTESIAN_POINT('Ctrl Pts',(0.3875739132888,-0.9806419265493,-7.768004514578));
#39662=CARTESIAN_POINT('Ctrl Pts',(-0.3432107204247,-0.9970351330367,-7.818704788154));
#39663=CARTESIAN_POINT('Ctrl Pts',(-0.9090640168405,-0.5342987274206,-7.86940506173));
#39664=CARTESIAN_POINT('Ctrl Pts',(-1.03806290686,0.1851970209741,-7.920105335306));
#39665=CARTESIAN_POINT('Ctrl Pts',(-0.668216439086,0.81569561,-7.970805608882));
#39666=CARTESIAN_POINT('Ctrl Pts',(0.02274415819314,1.054208346859,-8.021505882458));
#39667=CARTESIAN_POINT('Ctrl Pts',(0.7027749578096,0.7861169726968,-8.072206156034));
#39668=CARTESIAN_POINT('Ctrl Pts',(1.045084390477,0.1402538866513,-8.12290642961));
#39669=CARTESIAN_POINT('Ctrl Pts',(0.8851742648668,-0.573008775467,-8.173606703186));
#39670=CARTESIAN_POINT('Ctrl Pts',(0.2998900428063,-1.010909737899,-8.224306976762));
#39671=CARTESIAN_POINT('Ctrl Pts',(-0.4295075601491,-0.9630139104517,-8.275007250338));
#39672=CARTESIAN_POINT('Ctrl Pts',(-0.9525035565898,-0.4523378279972,-8.325707523914));
#39673=CARTESIAN_POINT('Ctrl Pts',(-1.017770091349,0.275711039135,-8.37640779749));
#39674=CARTESIAN_POINT('Ctrl Pts',(-0.5939430654806,0.8712658439924,-8.427108071066));
#39675=CARTESIAN_POINT('Ctrl Pts',(0.1153057184743,1.048130300761,-8.477808344642));
#39676=CARTESIAN_POINT('Ctrl Pts',(0.7691438697144,0.7213114743296,-8.528508618218));
#39677=CARTESIAN_POINT('Ctrl Pts',(1.053366804377,0.0478634837261,-8.579208891794));
#39678=CARTESIAN_POINT('Ctrl Pts',(0.8313900288183,-0.6485855033511,-8.62990916537));
#39679=CARTESIAN_POINT('Ctrl Pts',(0.2098854061311,-1.033354069586,-8.680609438946));
#39680=CARTESIAN_POINT('Ctrl Pts',(-0.5124805616198,-0.9215401939611,-8.731309712522));
#39681=CARTESIAN_POINT('Ctrl Pts',(-0.9885716900656,-0.3668761916084,-8.782009986098));
#39682=CARTESIAN_POINT('Ctrl Pts',(-0.9896014863655,0.364090781066,-8.832710259674));
#39683=CARTESIAN_POINT('Ctrl Pts',(-0.5150712073616,0.9200957200099,-8.88341053325));
#39684=CARTESIAN_POINT('Ctrl Pts',(0.2069672452441,1.033932698984,-8.934110806826));
#39685=CARTESIAN_POINT('Ctrl Pts',(0.8295892607691,0.6509547014876,-8.984811080402));
#39686=CARTESIAN_POINT('Ctrl Pts',(1.053390111087,-0.04501237598842,-9.035511353978));
#39687=CARTESIAN_POINT('Ctrl Pts',(0.8655115137905,-0.494146506137,-9.069311536362));
#39688=CARTESIAN_POINT('Ctrl Pts',(0.7094068585195,-0.6615450922541,-9.086211627554));
#39689=CARTESIAN_POINT('Ctrl Pts',(-0.9661995571575,0.08578120859872,-7.517162237882));
#39690=CARTESIAN_POINT('Ctrl Pts',(-0.9459577835372,0.313775113412,-7.534062329074));
#39691=CARTESIAN_POINT('Ctrl Pts',(-0.7373325155345,0.7536561561237,-7.567862511458));
#39692=CARTESIAN_POINT('Ctrl Pts',(-0.06998968740697,1.052170047392,-7.618562785034));
#39693=CARTESIAN_POINT('Ctrl Pts',(0.6309663956697,0.8448276002645,-7.66926305861));
#39694=CARTESIAN_POINT('Ctrl Pts',(1.028714521555,0.2315619048451,-7.719963332186));
#39695=CARTESIAN_POINT('Ctrl Pts',(0.932108219137,-0.4929984447149,-7.770663605762));
#39696=CARTESIAN_POINT('Ctrl Pts',(0.3875739132888,-0.9806419265493,-7.821363879338));
#39697=CARTESIAN_POINT('Ctrl Pts',(-0.3432107204247,-0.9970351330367,-7.872064152914));
#39698=CARTESIAN_POINT('Ctrl Pts',(-0.9090640168405,-0.5342987274206,-7.92276442649));
#39699=CARTESIAN_POINT('Ctrl Pts',(-1.03806290686,0.1851970209741,-7.973464700066));
#39700=CARTESIAN_POINT('Ctrl Pts',(-0.668216439086,0.81569561,-8.024164973642));
#39701=CARTESIAN_POINT('Ctrl Pts',(0.02274415819314,1.054208346859,-8.074865247218));
#39702=CARTESIAN_POINT('Ctrl Pts',(0.7027749578096,0.7861169726968,-8.125565520794));
#39703=CARTESIAN_POINT('Ctrl Pts',(1.045084390477,0.1402538866513,-8.17626579437));
#39704=CARTESIAN_POINT('Ctrl Pts',(0.8851742648668,-0.573008775467,-8.226966067946));
#39705=CARTESIAN_POINT('Ctrl Pts',(0.2998900428063,-1.010909737899,-8.277666341522));
#39706=CARTESIAN_POINT('Ctrl Pts',(-0.4295075601491,-0.9630139104517,-8.328366615098));
#39707=CARTESIAN_POINT('Ctrl Pts',(-0.9525035565898,-0.4523378279972,-8.379066888674));
#39708=CARTESIAN_POINT('Ctrl Pts',(-1.017770091349,0.275711039135,-8.42976716225));
#39709=CARTESIAN_POINT('Ctrl Pts',(-0.5939430654806,0.8712658439924,-8.480467435826));
#39710=CARTESIAN_POINT('Ctrl Pts',(0.1153057184743,1.048130300761,-8.531167709402));
#39711=CARTESIAN_POINT('Ctrl Pts',(0.7691438697144,0.7213114743296,-8.581867982978));
#39712=CARTESIAN_POINT('Ctrl Pts',(1.053366804377,0.0478634837261,-8.632568256554));
#39713=CARTESIAN_POINT('Ctrl Pts',(0.8313900288183,-0.6485855033511,-8.68326853013));
#39714=CARTESIAN_POINT('Ctrl Pts',(0.2098854061311,-1.033354069586,-8.733968803706));
#39715=CARTESIAN_POINT('Ctrl Pts',(-0.5124805616198,-0.9215401939611,-8.784669077282));
#39716=CARTESIAN_POINT('Ctrl Pts',(-0.9885716900656,-0.3668761916084,-8.835369350858));
#39717=CARTESIAN_POINT('Ctrl Pts',(-0.9896014863655,0.364090781066,-8.886069624434));
#39718=CARTESIAN_POINT('Ctrl Pts',(-0.5150712073616,0.9200957200099,-8.93676989801));
#39719=CARTESIAN_POINT('Ctrl Pts',(0.2069672452441,1.033932698984,-8.987470171586));
#39720=CARTESIAN_POINT('Ctrl Pts',(0.8295892607691,0.6509547014876,-9.038170445162));
#39721=CARTESIAN_POINT('Ctrl Pts',(1.053390111087,-0.04501237598842,-9.088870718738));
#39722=CARTESIAN_POINT('Ctrl Pts',(0.8655115137905,-0.494146506137,-9.122670901122));
#39723=CARTESIAN_POINT('Ctrl Pts',(0.7094068585195,-0.6615450922541,-9.139570992314));
#39724=CARTESIAN_POINT('Ctrl Pts',(-0.9661995571575,0.08578120859872,-7.570521602641));
#39725=CARTESIAN_POINT('Ctrl Pts',(-0.9459577835372,0.313775113412,-7.587421693833));
#39726=CARTESIAN_POINT('Ctrl Pts',(-0.7373325155345,0.7536561561237,-7.621221876217));
#39727=CARTESIAN_POINT('Ctrl Pts',(-0.06998968740697,1.052170047392,-7.671922149793));
#39728=CARTESIAN_POINT('Ctrl Pts',(0.6309663956697,0.8448276002645,-7.722622423369));
#39729=CARTESIAN_POINT('Ctrl Pts',(1.028714521555,0.2315619048451,-7.773322696945));
#39730=CARTESIAN_POINT('Ctrl Pts',(0.932108219137,-0.4929984447149,-7.824022970521));
#39731=CARTESIAN_POINT('Ctrl Pts',(0.3875739132888,-0.9806419265493,-7.874723244097));
#39732=CARTESIAN_POINT('Ctrl Pts',(-0.3432107204247,-0.9970351330367,-7.925423517673));
#39733=CARTESIAN_POINT('Ctrl Pts',(-0.9090640168405,-0.5342987274206,-7.976123791249));
#39734=CARTESIAN_POINT('Ctrl Pts',(-1.03806290686,0.1851970209741,-8.026824064825));
#39735=CARTESIAN_POINT('Ctrl Pts',(-0.668216439086,0.81569561,-8.077524338401));
#39736=CARTESIAN_POINT('Ctrl Pts',(0.02274415819314,1.054208346859,-8.128224611977));
#39737=CARTESIAN_POINT('Ctrl Pts',(0.7027749578096,0.7861169726968,-8.178924885553));
#39738=CARTESIAN_POINT('Ctrl Pts',(1.045084390477,0.1402538866513,-8.229625159129));
#39739=CARTESIAN_POINT('Ctrl Pts',(0.8851742648668,-0.573008775467,-8.280325432705));
#39740=CARTESIAN_POINT('Ctrl Pts',(0.2998900428063,-1.010909737899,-8.331025706281));
#39741=CARTESIAN_POINT('Ctrl Pts',(-0.4295075601491,-0.9630139104517,-8.381725979857));
#39742=CARTESIAN_POINT('Ctrl Pts',(-0.9525035565898,-0.4523378279972,-8.432426253433));
#39743=CARTESIAN_POINT('Ctrl Pts',(-1.017770091349,0.275711039135,-8.483126527009));
#39744=CARTESIAN_POINT('Ctrl Pts',(-0.5939430654806,0.8712658439924,-8.533826800585));
#39745=CARTESIAN_POINT('Ctrl Pts',(0.1153057184743,1.048130300761,-8.584527074161));
#39746=CARTESIAN_POINT('Ctrl Pts',(0.7691438697144,0.7213114743296,-8.635227347737));
#39747=CARTESIAN_POINT('Ctrl Pts',(1.053366804377,0.0478634837261,-8.685927621313));
#39748=CARTESIAN_POINT('Ctrl Pts',(0.8313900288183,-0.6485855033511,-8.736627894889));
#39749=CARTESIAN_POINT('Ctrl Pts',(0.2098854061311,-1.033354069586,-8.787328168465));
#39750=CARTESIAN_POINT('Ctrl Pts',(-0.5124805616198,-0.9215401939611,-8.838028442041));
#39751=CARTESIAN_POINT('Ctrl Pts',(-0.9885716900656,-0.3668761916084,-8.888728715617));
#39752=CARTESIAN_POINT('Ctrl Pts',(-0.9896014863655,0.364090781066,-8.939428989193));
#39753=CARTESIAN_POINT('Ctrl Pts',(-0.5150712073616,0.9200957200099,-8.990129262769));
#39754=CARTESIAN_POINT('Ctrl Pts',(0.2069672452441,1.033932698984,-9.040829536345));
#39755=CARTESIAN_POINT('Ctrl Pts',(0.8295892607691,0.6509547014876,-9.091529809921));
#39756=CARTESIAN_POINT('Ctrl Pts',(1.053390111087,-0.04501237598842,-9.142230083497));
#39757=CARTESIAN_POINT('Ctrl Pts',(0.8655115137905,-0.494146506137,-9.176030265881));
#39758=CARTESIAN_POINT('Ctrl Pts',(0.7094068585195,-0.6615450922541,-9.192930357073));
#39759=CARTESIAN_POINT('Ctrl Pts',(-0.9661995571575,0.08578120859872,-7.6238809674));
#39760=CARTESIAN_POINT('Ctrl Pts',(-0.9459577835372,0.313775113412,-7.640781058592));
#39761=CARTESIAN_POINT('Ctrl Pts',(-0.7373325155345,0.7536561561237,-7.674581240976));
#39762=CARTESIAN_POINT('Ctrl Pts',(-0.06998968740697,1.052170047392,-7.725281514552));
#39763=CARTESIAN_POINT('Ctrl Pts',(0.6309663956697,0.8448276002645,-7.775981788128));
#39764=CARTESIAN_POINT('Ctrl Pts',(1.028714521555,0.2315619048451,-7.826682061704));
#39765=CARTESIAN_POINT('Ctrl Pts',(0.932108219137,-0.4929984447149,-7.87738233528));
#39766=CARTESIAN_POINT('Ctrl Pts',(0.3875739132888,-0.9806419265493,-7.928082608856));
#39767=CARTESIAN_POINT('Ctrl Pts',(-0.3432107204247,-0.9970351330367,-7.978782882432));
#39768=CARTESIAN_POINT('Ctrl Pts',(-0.9090640168405,-0.5342987274206,-8.029483156008));
#39769=CARTESIAN_POINT('Ctrl Pts',(-1.03806290686,0.1851970209741,-8.080183429584));
#39770=CARTESIAN_POINT('Ctrl Pts',(-0.668216439086,0.81569561,-8.13088370316));
#39771=CARTESIAN_POINT('Ctrl Pts',(0.02274415819314,1.054208346859,-8.181583976736));
#39772=CARTESIAN_POINT('Ctrl Pts',(0.7027749578096,0.7861169726968,-8.232284250312));
#39773=CARTESIAN_POINT('Ctrl Pts',(1.045084390477,0.1402538866513,-8.282984523888));
#39774=CARTESIAN_POINT('Ctrl Pts',(0.8851742648668,-0.573008775467,-8.333684797464));
#39775=CARTESIAN_POINT('Ctrl Pts',(0.2998900428063,-1.010909737899,-8.38438507104));
#39776=CARTESIAN_POINT('Ctrl Pts',(-0.4295075601491,-0.9630139104517,-8.435085344616));
#39777=CARTESIAN_POINT('Ctrl Pts',(-0.9525035565898,-0.4523378279972,-8.485785618192));
#39778=CARTESIAN_POINT('Ctrl Pts',(-1.017770091349,0.275711039135,-8.536485891768));
#39779=CARTESIAN_POINT('Ctrl Pts',(-0.5939430654806,0.8712658439924,-8.587186165344));
#39780=CARTESIAN_POINT('Ctrl Pts',(0.1153057184743,1.048130300761,-8.63788643892));
#39781=CARTESIAN_POINT('Ctrl Pts',(0.7691438697144,0.7213114743296,-8.688586712496));
#39782=CARTESIAN_POINT('Ctrl Pts',(1.053366804377,0.0478634837261,-8.739286986072));
#39783=CARTESIAN_POINT('Ctrl Pts',(0.8313900288183,-0.6485855033511,-8.789987259648));
#39784=CARTESIAN_POINT('Ctrl Pts',(0.2098854061311,-1.033354069586,-8.840687533224));
#39785=CARTESIAN_POINT('Ctrl Pts',(-0.5124805616198,-0.9215401939611,-8.8913878068));
#39786=CARTESIAN_POINT('Ctrl Pts',(-0.9885716900656,-0.3668761916084,-8.942088080376));
#39787=CARTESIAN_POINT('Ctrl Pts',(-0.9896014863655,0.364090781066,-8.992788353952));
#39788=CARTESIAN_POINT('Ctrl Pts',(-0.5150712073616,0.9200957200099,-9.043488627528));
#39789=CARTESIAN_POINT('Ctrl Pts',(0.2069672452441,1.033932698984,-9.094188901104));
#39790=CARTESIAN_POINT('Ctrl Pts',(0.8295892607691,0.6509547014876,-9.14488917468));
#39791=CARTESIAN_POINT('Ctrl Pts',(1.053390111087,-0.04501237598842,-9.195589448256));
#39792=CARTESIAN_POINT('Ctrl Pts',(0.8655115137905,-0.494146506137,-9.22938963064));
#39793=CARTESIAN_POINT('Ctrl Pts',(0.7094068585195,-0.6615450922541,-9.246289721832));
#39794=CARTESIAN_POINT('Ctrl Pts',(0.92175594885483,-0.300215476254899,
-9.07172448818857));
#39795=CARTESIAN_POINT('Ctrl Pts',(0.92175594885483,-0.300215476254899,
-9.09283316090538));
#39796=CARTESIAN_POINT('Ctrl Pts',(0.92175594885483,-0.300215476254899,
-9.11394183362219));
#39797=CARTESIAN_POINT('Ctrl Pts',(0.92175594885483,-0.300215476254899,
-9.15616978382025));
#39798=CARTESIAN_POINT('Ctrl Pts',(0.921755948854829,-0.300215476254899,
-9.17728906130151));
#39799=CARTESIAN_POINT('Ctrl Pts',(0.921755948854829,-0.300215476254899,
-9.19840833878276));
#39800=CARTESIAN_POINT('Origin',(1.188547950716,-0.3871095049826,-9.360050506339));
#39801=CARTESIAN_POINT('Origin',(-2.019557620655,-2.019557620655,-27.6432));
#39802=CARTESIAN_POINT('',(-0.5440622782918,-0.2950136037689,-10.8));
#39803=CARTESIAN_POINT('',(-0.6490486745229,-0.4,-12.));
#39804=CARTESIAN_POINT('',(-0.2950136037689,-0.5440622782918,-10.8));
#39805=CARTESIAN_POINT('Origin',(-0.545968563155165,-0.545968563155165,
-10.8));
#39806=CARTESIAN_POINT('',(-0.4,-0.6490486745229,-12.));
#39807=CARTESIAN_POINT('Origin',(-0.4,-0.4,-12.));
#39808=CARTESIAN_POINT('',(-0.995964929246,-0.2950136037689,-10.8));
#39809=CARTESIAN_POINT('',(-0.995964929246,-0.2950136037689,-10.8));
#39810=CARTESIAN_POINT('',(-0.995964929246,-0.2950136037689,-10.8));
#39811=CARTESIAN_POINT('Origin',(0.,0.,-10.8));
#39812=CARTESIAN_POINT('',(0.2950136037689,-0.5440622782918,-10.8));
#39813=CARTESIAN_POINT('',(0.2950136037689,-0.995964929246,-10.8));
#39814=CARTESIAN_POINT('',(0.2950136037689,-0.5440622782918,-10.8));
#39815=CARTESIAN_POINT('',(0.04596492924595,-1.245013603769,-10.8));
#39816=CARTESIAN_POINT('Origin',(0.0440586443834295,-0.99405864438343,-10.8));
#39817=CARTESIAN_POINT('',(-0.04596492924595,-1.245013603769,-10.8));
#39818=CARTESIAN_POINT('',(0.04596492924595,-1.245013603769,-10.8));
#39819=CARTESIAN_POINT('',(-0.2950136037689,-0.995964929246,-10.8));
#39820=CARTESIAN_POINT('Origin',(-0.0440586443826807,-0.994058644382681,
-10.8));
#39821=CARTESIAN_POINT('',(-0.2950136037689,-0.5440622782918,-10.8));
#39822=CARTESIAN_POINT('',(-1.245013603769,-0.04596492924595,-10.8));
#39823=CARTESIAN_POINT('Origin',(-0.994058644383262,-0.0440586443832619,
-10.8));
#39824=CARTESIAN_POINT('',(-1.245013603769,0.04596492924595,-10.8));
#39825=CARTESIAN_POINT('',(-1.245013603769,0.04596492924595,-10.8));
#39826=CARTESIAN_POINT('',(-0.995964929246,0.2950136037689,-10.8));
#39827=CARTESIAN_POINT('Origin',(-0.994058644383421,0.0440586443834207,
-10.8));
#39828=CARTESIAN_POINT('',(-0.5440622782918,0.2950136037689,-10.8));
#39829=CARTESIAN_POINT('',(-0.995964929246,0.2950136037689,-10.8));
#39830=CARTESIAN_POINT('',(-0.2950136037689,0.5440622782918,-10.8));
#39831=CARTESIAN_POINT('Origin',(-0.545968563155165,0.545968563155165,-10.8));
#39832=CARTESIAN_POINT('',(-0.2950136037689,0.995964929246,-10.8));
#39833=CARTESIAN_POINT('',(-0.2950136037689,0.995964929246,-10.8));
#39834=CARTESIAN_POINT('',(-0.04596492924595,1.245013603769,-10.8));
#39835=CARTESIAN_POINT('Origin',(-0.0440586443832125,0.994058644383213,
-10.8));
#39836=CARTESIAN_POINT('',(0.04596492924595,1.245013603769,-10.8));
#39837=CARTESIAN_POINT('',(-0.04596492924595,1.245013603769,-10.8));
#39838=CARTESIAN_POINT('',(0.2950136037689,0.995964929246,-10.8));
#39839=CARTESIAN_POINT('Origin',(0.0440586443829719,0.994058644382972,-10.8));
#39840=CARTESIAN_POINT('',(0.2950136037689,0.5440622782918,-10.8));
#39841=CARTESIAN_POINT('',(0.2950136037689,0.995964929246,-10.8));
#39842=CARTESIAN_POINT('',(0.5440622782918,0.2950136037689,-10.8));
#39843=CARTESIAN_POINT('Origin',(0.545968563155165,0.545968563155165,-10.8));
#39844=CARTESIAN_POINT('',(0.995964929246,0.2950136037689,-10.8));
#39845=CARTESIAN_POINT('',(0.5440622782918,0.2950136037689,-10.8));
#39846=CARTESIAN_POINT('',(1.245013603769,0.04596492924595,-10.8));
#39847=CARTESIAN_POINT('Origin',(0.994058644383084,0.0440586443830834,-10.8));
#39848=CARTESIAN_POINT('',(1.245013603769,-0.04596492924595,-10.8));
#39849=CARTESIAN_POINT('',(1.245013603769,-0.04596492924595,-10.8));
#39850=CARTESIAN_POINT('',(0.995964929246,-0.2950136037689,-10.8));
#39851=CARTESIAN_POINT('Origin',(0.994058644382849,-0.0440586443828492,
-10.8));
#39852=CARTESIAN_POINT('',(0.5440622782918,-0.2950136037689,-10.8));
#39853=CARTESIAN_POINT('',(0.995964929246,-0.2950136037689,-10.8));
#39854=CARTESIAN_POINT('Origin',(0.545968563155165,-0.545968563155165,-10.8));
#39855=CARTESIAN_POINT('Origin',(0.4,-0.4,-12.));
#39856=CARTESIAN_POINT('',(0.4,-0.6490486745229,-12.));
#39857=CARTESIAN_POINT('',(0.2950136037689,-0.995964929246,-10.8));
#39858=CARTESIAN_POINT('Origin',(2.019557620655,-2.019557620655,-27.6432));
#39859=CARTESIAN_POINT('',(0.6490486745229,-0.4,-12.));
#39860=CARTESIAN_POINT('Origin',(1.35,-0.4,-12.));
#39861=CARTESIAN_POINT('',(0.995964929246,-0.2950136037689,-10.8));
#39862=CARTESIAN_POINT('Origin',(-1.167126683436,2.117126683436,13.90246133293));
#39863=CARTESIAN_POINT('',(1.245013603769,-0.04596492924595,-10.8));
#39864=CARTESIAN_POINT('Origin',(1.35,0.4,-12.));
#39865=CARTESIAN_POINT('',(1.245013603769,0.04596492924595,-10.8));
#39866=CARTESIAN_POINT('Origin',(-1.164769817959,-2.114769817959,13.87552223726));
#39867=CARTESIAN_POINT('',(0.995964929246,0.2950136037689,-10.8));
#39868=CARTESIAN_POINT('Origin',(0.4,0.4,-12.));
#39869=CARTESIAN_POINT('',(0.6490486745229,0.4,-12.));
#39870=CARTESIAN_POINT('Origin',(2.019557620655,2.019557620655,-27.6432));
#39871=CARTESIAN_POINT('',(0.4,0.6490486745229,-12.));
#39872=CARTESIAN_POINT('Origin',(0.4,1.35,-12.));
#39873=CARTESIAN_POINT('',(0.2950136037689,0.995964929246,-10.8));
#39874=CARTESIAN_POINT('Origin',(-2.113404067612,-1.163404067612,13.85991163936));
#39875=CARTESIAN_POINT('',(0.04596492924595,1.245013603769,-10.8));
#39876=CARTESIAN_POINT('Origin',(-0.4,1.35,-12.));
#39877=CARTESIAN_POINT('',(-0.04596492924595,1.245013603769,-10.8));
#39878=CARTESIAN_POINT('Origin',(2.115813258549,-1.165813258549,13.88744881778));
#39879=CARTESIAN_POINT('',(-0.2950136037689,0.995964929246,-10.8));
#39880=CARTESIAN_POINT('Origin',(-0.4,0.4,-12.));
#39881=CARTESIAN_POINT('',(-0.4,0.6490486745229,-12.));
#39882=CARTESIAN_POINT('Origin',(-2.019557620655,2.019557620655,-27.6432));
#39883=CARTESIAN_POINT('',(-0.6490486745229,0.4,-12.));
#39884=CARTESIAN_POINT('Origin',(-1.35,0.4,-12.));
#39885=CARTESIAN_POINT('',(-0.995964929246,0.2950136037689,-10.8));
#39886=CARTESIAN_POINT('Origin',(1.229404966539,-2.179404966539,14.61430536613));
#39887=CARTESIAN_POINT('',(-1.245013603769,0.04596492924595,-10.8));
#39888=CARTESIAN_POINT('Origin',(-1.35,-0.4,-12.));
#39889=CARTESIAN_POINT('',(-1.245013603769,-0.04596492924595,-10.8));
#39890=CARTESIAN_POINT('Origin',(1.25220562464,2.20220562464,14.87491808076));
#39891=CARTESIAN_POINT('Origin',(-2.18078482228,1.23078482228,14.63007718942));
#39892=CARTESIAN_POINT('',(0.04596492924595,-1.245013603769,-10.8));
#39893=CARTESIAN_POINT('Origin',(0.4,-1.35,-12.));
#39894=CARTESIAN_POINT('',(-0.04596492924595,-1.245013603769,-10.8));
#39895=CARTESIAN_POINT('Origin',(2.202175235882,1.252175235882,14.87457073566));
#39896=CARTESIAN_POINT('',(-0.2950136037689,-0.995964929246,-10.8));
#39897=CARTESIAN_POINT('Origin',(-0.4,-1.35,-12.));
#39898=CARTESIAN_POINT('',(0.,0.,0.));
#39899=CARTESIAN_POINT('Origin',(-4.6,0.,0.));
#39900=CARTESIAN_POINT('',(-4.6,10.41,7.5));
#39901=CARTESIAN_POINT('',(-4.6,1.41,7.5));
#39902=CARTESIAN_POINT('',(-4.6,10.40999999984,7.5));
#39903=CARTESIAN_POINT('',(-4.6000000442632,10.4099999970609,-7.98856626783461));
#39904=CARTESIAN_POINT('',(-4.6,10.40999999984,7.5));
#39905=CARTESIAN_POINT('',(-4.599999995006,5.31268601529799,-7.988586197742));
#39906=CARTESIAN_POINT('',(-4.599999995006,5.312686015298,-7.988586197742));
#39907=CARTESIAN_POINT('',(-4.60000008479568,3.59647899566988,-7.50000015263407));
#39908=CARTESIAN_POINT('Ctrl Pts',(-4.60000005087721,3.59647899566978,-7.50000015263649));
#39909=CARTESIAN_POINT('Ctrl Pts',(-4.59999986298528,3.70619272292874,-7.50000123432406));
#39910=CARTESIAN_POINT('Ctrl Pts',(-4.60000006358096,3.91406362288072,-7.51418484353807));
#39911=CARTESIAN_POINT('Ctrl Pts',(-4.599999982988,4.189476771086,-7.561416026773));
#39912=CARTESIAN_POINT('Ctrl Pts',(-4.600000004468,4.434127618739,-7.624029192647));
#39913=CARTESIAN_POINT('Ctrl Pts',(-4.599999999139,4.650710856925,-7.694659592193));
#39914=CARTESIAN_POINT('Ctrl Pts',(-4.599999998977,4.843005160611,-7.768527138287));
#39915=CARTESIAN_POINT('Ctrl Pts',(-4.600000004953,5.015100702816,-7.842916001697));
#39916=CARTESIAN_POINT('Ctrl Pts',(-4.599999981211,5.170593933842,-7.916289820707));
#39917=CARTESIAN_POINT('Ctrl Pts',(-4.60000004054,5.266673416514,-7.964776668264));
#39918=CARTESIAN_POINT('Ctrl Pts',(-4.599999995006,5.312686015298,-7.988586197742));
#39919=CARTESIAN_POINT('',(-4.6,1.41,-7.5));
#39920=CARTESIAN_POINT('',(-4.6,1.41,-7.5));
#39921=CARTESIAN_POINT('Origin',(-4.6,1.41,0.));
#39922=CARTESIAN_POINT('',(-4.6,7.40960552762211,0.0688005299851782));
#39923=CARTESIAN_POINT('Origin',(-4.6,1.41,0.));
#39924=CARTESIAN_POINT('Origin',(-5.6,1.41,0.));
#39925=CARTESIAN_POINT('',(-5.6,-3.59,0.));
#39926=CARTESIAN_POINT('',(-5.6,6.40967127301842,0.0573337749876485));
#39927=CARTESIAN_POINT('Origin',(-5.6,1.41,0.));
#39928=CARTESIAN_POINT('Origin',(-5.6,1.41,0.));
#39929=CARTESIAN_POINT('Origin',(-5.6,7.40960552762211,0.0688005299851782));
#39930=CARTESIAN_POINT('Origin',(-4.6,1.41,0.));
#39931=CARTESIAN_POINT('',(-14.6,-3.59,6.12323399573677E-16));
#39932=CARTESIAN_POINT('Origin',(-14.6,1.41,0.));
#39933=CARTESIAN_POINT('',(-4.6,-3.59,6.12323399573677E-16));
#39934=CARTESIAN_POINT('Origin',(-14.6,0.,0.));
#39935=CARTESIAN_POINT('',(-14.6,1.41,4.));
#39936=CARTESIAN_POINT('Origin',(-14.6,1.41,0.));
#39937=CARTESIAN_POINT('Origin',(-14.6,1.41,0.));
#39938=CARTESIAN_POINT('',(-12.599955217472,-2.05311064648514,2.00006051196135));
#39939=CARTESIAN_POINT('',(-12.6,1.41,4.));
#39940=CARTESIAN_POINT('Origin',(-12.6,1.41,0.));
#39941=CARTESIAN_POINT('Origin',(-12.6,1.41,0.));
#39942=CARTESIAN_POINT('',(-14.6,1.41,4.));
#39943=CARTESIAN_POINT('Origin',(-14.6,1.41,0.));
#39944=CARTESIAN_POINT('',(-3.1,1.41,4.));
#39945=CARTESIAN_POINT('Origin',(-3.1,1.41,0.));
#39946=CARTESIAN_POINT('',(-4.47396821277762,1.41,4.));
#39947=CARTESIAN_POINT('',(-14.6,1.41,4.));
#39948=CARTESIAN_POINT('',(-4.59999337538372,4.87352195157167,1.99964693648141));
#39949=CARTESIAN_POINT('Ctrl Pts',(-4.47396821277762,1.41,4.));
#39950=CARTESIAN_POINT('Ctrl Pts',(-4.47802321474399,1.55267489674965,4.));
#39951=CARTESIAN_POINT('Ctrl Pts',(-4.48213222009309,1.69531596101135,3.99236651952116));
#39952=CARTESIAN_POINT('Ctrl Pts',(-4.4906681550104,1.98294016555199,3.96146336088247));
#39953=CARTESIAN_POINT('Ctrl Pts',(-4.49509226438512,2.12759535602225,3.93783030862076));
#39954=CARTESIAN_POINT('Ctrl Pts',(-4.50494469986381,2.43962006156562,3.86908618594094));
#39955=CARTESIAN_POINT('Ctrl Pts',(-4.51040173745819,2.606018396681,3.82092707313125));
#39956=CARTESIAN_POINT('Ctrl Pts',(-4.52038860740983,2.90457634300073,3.71309713998014));
#39957=CARTESIAN_POINT('Ctrl Pts',(-4.5249123165038,3.03762834249849,3.65673024246835));
#39958=CARTESIAN_POINT('Ctrl Pts',(-4.53190546949731,3.24531722210745,3.55515752690714));
#39959=CARTESIAN_POINT('Ctrl Pts',(-4.53446142185042,3.32202920690643,3.51449549885797));
#39960=CARTESIAN_POINT('Ctrl Pts',(-4.54034315694366,3.49849701357434,3.41346772535774));
#39961=CARTESIAN_POINT('Ctrl Pts',(-4.54363691334612,3.59705824950081,3.35117270985553));
#39962=CARTESIAN_POINT('Ctrl Pts',(-4.55372497360401,3.89061373063259,3.1471588930267));
#39963=CARTESIAN_POINT('Ctrl Pts',(-4.56051176646417,4.07563514531634,2.99206294673198));
#39964=CARTESIAN_POINT('Ctrl Pts',(-4.57194713221524,4.34894837595383,2.71736344368141));
#39965=CARTESIAN_POINT('Ctrl Pts',(-4.57637475970776,4.44653251476823,2.60786314180913));
#39966=CARTESIAN_POINT('Ctrl Pts',(-4.58703999719547,4.66209483283886,2.33743206191275));
#39967=CARTESIAN_POINT('Ctrl Pts',(-4.59334861861747,4.77448463373213,2.1725445592894));
#39968=CARTESIAN_POINT('Ctrl Pts',(-4.59960196669704,4.87411610028898,1.99997491077231));
#39969=CARTESIAN_POINT('',(-3.84878783026703,4.87410161478956,1.99999999974644));
#39970=CARTESIAN_POINT('',(-3.85,4.874101615138,2.));
#39971=CARTESIAN_POINT('Ctrl Pts',(-3.84878782952482,4.87410161517191,1.99999999994084));
#39972=CARTESIAN_POINT('Ctrl Pts',(-3.85713541463281,5.00988343647519,1.76481898669005));
#39973=CARTESIAN_POINT('Ctrl Pts',(-3.86579655320577,5.12135499796743,1.516438340068));
#39974=CARTESIAN_POINT('Ctrl Pts',(-3.87700357702665,5.23571314511595,1.17147723100828));
#39975=CARTESIAN_POINT('Ctrl Pts',(-3.87979301326392,5.2616099576731,1.08330147408813));
#39976=CARTESIAN_POINT('Ctrl Pts',(-3.8875324253198,5.3267758384964,0.829374396988071));
#39977=CARTESIAN_POINT('Ctrl Pts',(-3.89232372159689,5.35852935393098,0.661901534699769));
#39978=CARTESIAN_POINT('Ctrl Pts',(-3.90164445511241,5.39933068569783,0.33332088901751));
#39979=CARTESIAN_POINT('Ctrl Pts',(-3.90616577556016,5.40950533665437,0.172680457019602));
#39980=CARTESIAN_POINT('Ctrl Pts',(-3.91485918785644,5.4103998948561,-0.128868547334375));
#39981=CARTESIAN_POINT('Ctrl Pts',(-3.91899728472511,5.403389775243,-0.269523734791878));
#39982=CARTESIAN_POINT('Ctrl Pts',(-3.92949010169241,5.36774660483486,-0.61584506126014));
#39983=CARTESIAN_POINT('Ctrl Pts',(-3.93596171182252,5.33049500919419,-0.820205843112968));
#39984=CARTESIAN_POINT('Ctrl Pts',(-3.94678581469179,5.2428813894696,-1.15216962797743));
#39985=CARTESIAN_POINT('Ctrl Pts',(-3.95108720632083,5.20151982219127,-1.28173804047728));
#39986=CARTESIAN_POINT('Ctrl Pts',(-3.95815429399473,5.12128476646775,-1.49492622583711));
#39987=CARTESIAN_POINT('Ctrl Pts',(-3.96096131409489,5.08597329433121,-1.57976605202262));
#39988=CARTESIAN_POINT('Ctrl Pts',(-3.96807606494566,4.98634724012396,-1.7976538191658));
#39989=CARTESIAN_POINT('Ctrl Pts',(-3.97227914857057,4.91752868463037,-1.92848733538));
#39990=CARTESIAN_POINT('Ctrl Pts',(-3.98146324970479,4.75069385577068,-2.20705429926935));
#39991=CARTESIAN_POINT('Ctrl Pts',(-3.98642774730493,4.6497812556587,-2.35268808037349));
#39992=CARTESIAN_POINT('Ctrl Pts',(-3.99578896820218,4.44727408042526,-2.60709077350989));
#39993=CARTESIAN_POINT('Ctrl Pts',(-4.00013752226369,4.34862331805883,-2.71780196259597));
#39994=CARTESIAN_POINT('Ctrl Pts',(-4.01175666237124,4.07623497223659,-2.99127849459317));
#39995=CARTESIAN_POINT('Ctrl Pts',(-4.01920284314558,3.8937221440456,-3.14446714373292));
#39996=CARTESIAN_POINT('Ctrl Pts',(-4.03039684119057,3.60194021417812,-3.34803162291242));
#39997=CARTESIAN_POINT('Ctrl Pts',(-4.03410508977674,3.50224692417008,-3.41121985721898));
#39998=CARTESIAN_POINT('Ctrl Pts',(-4.04043259544245,3.32413614929383,-3.51336192411137));
#39999=CARTESIAN_POINT('Ctrl Pts',(-4.04307908412172,3.24696082787826,-3.5543220716129));
#40000=CARTESIAN_POINT('Ctrl Pts',(-4.04985989702705,3.04053940671477,-3.65535752920676));
#40001=CARTESIAN_POINT('Ctrl Pts',(-4.05390375534371,2.90931869158175,-3.71111069265977));
#40002=CARTESIAN_POINT('Ctrl Pts',(-4.06284193540848,2.6119042658904,-3.81912070415939));
#40003=CARTESIAN_POINT('Ctrl Pts',(-4.06772160347664,2.44470973556781,-3.86776837074836));
#40004=CARTESIAN_POINT('Ctrl Pts',(-4.07694932757382,2.1317539852889,-3.937075200695));
#40005=CARTESIAN_POINT('Ctrl Pts',(-4.08125169467157,1.98699651538995,-3.9608791166392));
#40006=CARTESIAN_POINT('Ctrl Pts',(-4.09301151892351,1.59860160398172,-4.00299962462465));
#40007=CARTESIAN_POINT('Ctrl Pts',(-4.10066579918578,1.35404823912446,-4.00704862421727));
#40008=CARTESIAN_POINT('Ctrl Pts',(-4.11198140633078,0.995637385022808,
-3.98015192630208));
#40009=CARTESIAN_POINT('Ctrl Pts',(-4.11560712496378,0.881036526030751,
-3.96654810079726));
#40010=CARTESIAN_POINT('Ctrl Pts',(-4.12182572942684,0.681857405149143,
-3.93411767562979));
#40011=CARTESIAN_POINT('Ctrl Pts',(-4.12444412527263,0.597001844273346,
-3.9174620287807));
#40012=CARTESIAN_POINT('Ctrl Pts',(-4.13110257820161,0.377059353180721,
-3.86683599508181));
#40013=CARTESIAN_POINT('Ctrl Pts',(-4.13505818047302,0.243090662860835,
-3.82853903941916));
#40014=CARTESIAN_POINT('Ctrl Pts',(-4.14394891611014,-0.054486106748681,
-3.72639733363896));
#40015=CARTESIAN_POINT('Ctrl Pts',(-4.14886701052946,-0.21643691126297,
-3.65861438934144));
#40016=CARTESIAN_POINT('Ctrl Pts',(-4.15814707995622,-0.505052760626267,
-3.51485425923717));
#40017=CARTESIAN_POINT('Ctrl Pts',(-4.16246184930138,-0.632970335824287,
-3.44207759098763));
#40018=CARTESIAN_POINT('Ctrl Pts',(-4.17427317410496,-0.962885856764186,
-3.22949556864293));
#40019=CARTESIAN_POINT('Ctrl Pts',(-4.18196943446053,-1.15650713704172,
-3.07786656994227));
#40020=CARTESIAN_POINT('Ctrl Pts',(-4.19330963588578,-1.41854072582884,
-2.8306444192109));
#40021=CARTESIAN_POINT('Ctrl Pts',(-4.19691868971951,-1.49864594316486,
-2.74826667233921));
#40022=CARTESIAN_POINT('Ctrl Pts',(-4.2031172102864,-1.63257299550026,-2.59811580101652));
#40023=CARTESIAN_POINT('Ctrl Pts',(-4.20573170133228,-1.68795019061716,
-2.5318297690859));
#40024=CARTESIAN_POINT('Ctrl Pts',(-4.21379853036606,-1.85641204159948,
-2.31637107637409));
#40025=CARTESIAN_POINT('Ctrl Pts',(-4.21904724525982,-1.96119737707697,
-2.16103083840407));
#40026=CARTESIAN_POINT('Ctrl Pts',(-4.2304429640341,-2.16303601414209,-1.81118493732632));
#40027=CARTESIAN_POINT('Ctrl Pts',(-4.23659162406759,-2.25590822224409,
-1.61495872649002));
#40028=CARTESIAN_POINT('Ctrl Pts',(-4.24737437252633,-2.38473453489288,
-1.27355504778905));
#40029=CARTESIAN_POINT('Ctrl Pts',(-4.25185779501106,-2.4292993041449,-1.13213589537751));
#40030=CARTESIAN_POINT('Ctrl Pts',(-4.26197854844312,-2.5102892524769,-0.814597428677815));
#40031=CARTESIAN_POINT('Ctrl Pts',(-4.26765100744546,-2.54289827053674,
-0.637832512510027));
#40032=CARTESIAN_POINT('Ctrl Pts',(-4.27774887369803,-2.5798033346779,-0.318682236892733));
#40033=CARTESIAN_POINT('Ctrl Pts',(-4.28217494180975,-2.58858978675153,
-0.177116159811553));
#40034=CARTESIAN_POINT('Ctrl Pts',(-4.28926655321653,-2.59067481180548,
0.0585969388013058));
#40035=CARTESIAN_POINT('Ctrl Pts',(-4.29201068090646,-2.58819377611921,
0.152574799179403));
#40036=CARTESIAN_POINT('Ctrl Pts',(-4.29878578355939,-2.57367560802579,
0.387832894517081));
#40037=CARTESIAN_POINT('Ctrl Pts',(-4.30276284383635,-2.55743444386133,
0.52872530002292));
#40038=CARTESIAN_POINT('Ctrl Pts',(-4.31230255643117,-2.50096633200525,
0.861873716315035));
#40039=CARTESIAN_POINT('Ctrl Pts',(-4.31788348855111,-2.453999722358,1.05261009223179));
#40040=CARTESIAN_POINT('Ctrl Pts',(-4.327967578155,-2.34806572404957,1.37775114719943));
#40041=CARTESIAN_POINT('Ctrl Pts',(-4.33236795299842,-2.29535704235641,
1.51379776175824));
#40042=CARTESIAN_POINT('Ctrl Pts',(-4.34211297525343,-2.16517264423272,
1.80199710714394));
#40043=CARTESIAN_POINT('Ctrl Pts',(-4.34748378207211,-2.08514825905764,
1.95268789156043));
#40044=CARTESIAN_POINT('Ctrl Pts',(-4.35757777991757,-1.9169318958898,2.22578408856121));
#40045=CARTESIAN_POINT('Ctrl Pts',(-4.36229212032352,-1.83095405365336,
2.34921451452121));
#40046=CARTESIAN_POINT('Ctrl Pts',(-4.36947139588852,-1.68449076055774,
2.53608297090013));
#40047=CARTESIAN_POINT('Ctrl Pts',(-4.37203545870452,-1.62852322666058,
2.6028765715856));
#40048=CARTESIAN_POINT('Ctrl Pts',(-4.37795854739217,-1.49190155599502,
2.75550846278849));
#40049=CARTESIAN_POINT('Ctrl Pts',(-4.3812844372048,-1.40954893698499,2.83971899317701));
#40050=CARTESIAN_POINT('Ctrl Pts',(-4.39131853259455,-1.1499424513066,3.08273888832691));
#40051=CARTESIAN_POINT('Ctrl Pts',(-4.39802228460691,-0.962132639711373,
3.22948431899847));
#40052=CARTESIAN_POINT('Ctrl Pts',(-4.40935447792384,-0.639598163602044,
3.43810075559831));
#40053=CARTESIAN_POINT('Ctrl Pts',(-4.41377098264549,-0.512534997877063,
3.51073309565376));
#40054=CARTESIAN_POINT('Ctrl Pts',(-4.4235888209087,-0.22781721186987,3.65338347748354));
#40055=CARTESIAN_POINT('Ctrl Pts',(-4.4290180390454,-0.069032505004638,
3.72049959394663));
#40056=CARTESIAN_POINT('Ctrl Pts',(-4.43903876498291,0.231704694822792,
3.82531257514947));
#40057=CARTESIAN_POINT('Ctrl Pts',(-4.44362315896157,0.372369284968778,
3.86584013175734));
#40058=CARTESIAN_POINT('Ctrl Pts',(-4.45067549964498,0.599632867071186,
3.91801688464264));
#40059=CARTESIAN_POINT('Ctrl Pts',(-4.45323391251286,0.684937018050481,
3.93469628057976));
#40060=CARTESIAN_POINT('Ctrl Pts',(-4.45912820200206,0.886115422586876,
3.9672674116583));
#40061=CARTESIAN_POINT('Ctrl Pts',(-4.46243171505446,1.00227842112557,3.98088300670763));
#40062=CARTESIAN_POINT('Ctrl Pts',(-4.46847307119201,1.21580144485612,3.99646497806116));
#40063=CARTESIAN_POINT('Ctrl Pts',(-4.47120875000575,1.31290853880528,4.));
#40064=CARTESIAN_POINT('Ctrl Pts',(-4.47396821277762,1.41,4.));
#40065=CARTESIAN_POINT('Origin',(-12.6,0.,0.));
#40066=CARTESIAN_POINT('',(-12.5998293715479,4.2015986146261,2.27233586799447));
#40067=CARTESIAN_POINT('Ctrl Pts',(-12.6,-2.05373368417785,2.00041480624693));
#40068=CARTESIAN_POINT('Ctrl Pts',(-12.6,-1.86194821019491,2.29644101354744));
#40069=CARTESIAN_POINT('Ctrl Pts',(-12.6,-1.6337237691026,2.56258505139432));
#40070=CARTESIAN_POINT('Ctrl Pts',(-12.6,-1.11617616238642,3.02636049189356));
#40071=CARTESIAN_POINT('Ctrl Pts',(-12.6,-0.82928342253897,3.22307976599948));
#40072=CARTESIAN_POINT('Ctrl Pts',(-12.6,-0.123052762143918,3.5775029713655));
#40073=CARTESIAN_POINT('Ctrl Pts',(-12.6,0.359088891234675,3.7349719142707));
#40074=CARTESIAN_POINT('Ctrl Pts',(-12.6,1.34810068326337,3.8116791096069));
#40075=CARTESIAN_POINT('Ctrl Pts',(-12.6,1.84369675616155,3.77282245092087));
#40076=CARTESIAN_POINT('Ctrl Pts',(-12.6,2.72178118022736,3.49119653737293));
#40077=CARTESIAN_POINT('Ctrl Pts',(-12.5999999999996,3.07511507231026,3.31288578245549));
#40078=CARTESIAN_POINT('Ctrl Pts',(-12.5999999999996,3.75009162428244,2.82374222223055));
#40079=CARTESIAN_POINT('Ctrl Pts',(-12.6,4.01274809895788,2.53388433006154));
#40080=CARTESIAN_POINT('Ctrl Pts',(-12.6,4.20183229445798,2.27251622505692));
#40081=CARTESIAN_POINT('',(-12.6000166008662,0.83772686667478,-3.55358061870878));
#40082=CARTESIAN_POINT('Ctrl Pts',(-12.6,0.837723077840343,-3.55360908009661));
#40083=CARTESIAN_POINT('Ctrl Pts',(-12.6,0.496521059253182,-3.51949309243697));
#40084=CARTESIAN_POINT('Ctrl Pts',(-12.5999999999999,0.146329052235482,
-3.43525773297163));
#40085=CARTESIAN_POINT('Ctrl Pts',(-12.5999999999999,-0.553018328867865,
-3.134995004088));
#40086=CARTESIAN_POINT('Ctrl Pts',(-12.5999999999999,-0.871307034171167,
-2.93779118035574));
#40087=CARTESIAN_POINT('Ctrl Pts',(-12.5999999999999,-1.53424447284485,
-2.37755905857722));
#40088=CARTESIAN_POINT('Ctrl Pts',(-12.6,-1.83990405226507,-1.98879992581603));
#40089=CARTESIAN_POINT('Ctrl Pts',(-12.6,-2.29324808716915,-1.09713296481856));
#40090=CARTESIAN_POINT('Ctrl Pts',(-12.6000000000002,-2.43367803893011,
-0.602366737831792));
#40091=CARTESIAN_POINT('Ctrl Pts',(-12.6000000000002,-2.50222265717766,
0.237740648443177));
#40092=CARTESIAN_POINT('Ctrl Pts',(-12.6000000000001,-2.48645615185202,
0.59285266331533));
#40093=CARTESIAN_POINT('Ctrl Pts',(-12.6000000000001,-2.33846043510994,
1.32747957975342));
#40094=CARTESIAN_POINT('Ctrl Pts',(-12.6,-2.21733170155652,1.67484059027454));
#40095=CARTESIAN_POINT('Ctrl Pts',(-12.6,-2.05238345558469,1.99966421701685));
#40096=CARTESIAN_POINT('Ctrl Pts',(-12.6,4.20136030793409,2.27216120781755));
#40097=CARTESIAN_POINT('Ctrl Pts',(-12.6,4.24991321932181,2.21237988743208));
#40098=CARTESIAN_POINT('Ctrl Pts',(-12.6,4.29624720254232,2.15145486239861));
#40099=CARTESIAN_POINT('Ctrl Pts',(-12.6,4.34045738936432,2.08940595404779));
#40100=CARTESIAN_POINT('Ctrl Pts',(-12.6,4.3850853028298,2.02677076719239));
#40101=CARTESIAN_POINT('Ctrl Pts',(-12.6,4.42754941898348,1.96298989968627));
#40102=CARTESIAN_POINT('Ctrl Pts',(-12.6,4.4679095774266,1.89804670263138));
#40103=CARTESIAN_POINT('Ctrl Pts',(-12.6,4.50538330437375,1.83774803861745));
#40104=CARTESIAN_POINT('Ctrl Pts',(-12.6,4.54104318206744,1.77644645371704));
#40105=CARTESIAN_POINT('Ctrl Pts',(-12.6,4.57490409351515,1.71410627284305));
#40106=CARTESIAN_POINT('Ctrl Pts',(-12.6,4.63217999330126,1.60865754746247));
#40107=CARTESIAN_POINT('Ctrl Pts',(-12.6,4.68429586644297,1.50024999578326));
#40108=CARTESIAN_POINT('Ctrl Pts',(-12.6,4.73090070615598,1.38925781853925));
#40109=CARTESIAN_POINT('Ctrl Pts',(-12.6,4.76695274428081,1.3033977612963));
#40110=CARTESIAN_POINT('Ctrl Pts',(-12.6,4.79970608847906,1.21599067617616));
#40111=CARTESIAN_POINT('Ctrl Pts',(-12.6,4.82897683811643,1.12720778050039));
#40112=CARTESIAN_POINT('Ctrl Pts',(-12.6,4.85313221137757,1.05394064485055));
#40113=CARTESIAN_POINT('Ctrl Pts',(-12.6,4.87491474427738,0.979727992501767));
#40114=CARTESIAN_POINT('Ctrl Pts',(-12.6,4.8942662152241,0.904841310809496));
#40115=CARTESIAN_POINT('Ctrl Pts',(-12.6,4.91634804391075,0.819388640023172));
#40116=CARTESIAN_POINT('Ctrl Pts',(-12.6,4.93526322302942,0.733059052030427));
#40117=CARTESIAN_POINT('Ctrl Pts',(-12.6,4.95097297319694,0.646271284840811));
#40118=CARTESIAN_POINT('Ctrl Pts',(-12.6,4.96214115241793,0.584573210216633));
#40119=CARTESIAN_POINT('Ctrl Pts',(-12.6,4.97169041730954,0.522643909668857));
#40120=CARTESIAN_POINT('Ctrl Pts',(-12.6,4.97962272537674,0.460635682766227));
#40121=CARTESIAN_POINT('Ctrl Pts',(-12.6,4.99040979052231,0.376311325026525));
#40122=CARTESIAN_POINT('Ctrl Pts',(-12.6,4.99821257200861,0.291844226308379));
#40123=CARTESIAN_POINT('Ctrl Pts',(-12.6,5.00307142381211,0.207270573524764));
#40124=CARTESIAN_POINT('Ctrl Pts',(-12.6,5.00810941634383,0.11957877959151));
#40125=CARTESIAN_POINT('Ctrl Pts',(-12.6,5.00998274524699,0.0317718262261336));
#40126=CARTESIAN_POINT('Ctrl Pts',(-12.6,5.00867893574776,-0.0561151865291535));
#40127=CARTESIAN_POINT('Ctrl Pts',(-12.6,5.00792611094464,-0.106861498097263));
#40128=CARTESIAN_POINT('Ctrl Pts',(-12.6,5.00611296071654,-0.157634547885469));
#40129=CARTESIAN_POINT('Ctrl Pts',(-12.6,5.00322813990553,-0.208426976174122));
#40130=CARTESIAN_POINT('Ctrl Pts',(-12.6,4.99817808622467,-0.297342200461094));
#40131=CARTESIAN_POINT('Ctrl Pts',(-12.6,4.98983826675716,-0.386322571517995));
#40132=CARTESIAN_POINT('Ctrl Pts',(-12.6,4.97817114946835,-0.474964333428603));
#40133=CARTESIAN_POINT('Ctrl Pts',(-12.6,4.96609764893234,-0.566693621259453));
#40134=CARTESIAN_POINT('Ctrl Pts',(-12.6,4.95046069958265,-0.658059603697444));
#40135=CARTESIAN_POINT('Ctrl Pts',(-12.6,4.93126873595277,-0.748617385727737));
#40136=CARTESIAN_POINT('Ctrl Pts',(-12.6,4.92455646675259,-0.780289403395168));
#40137=CARTESIAN_POINT('Ctrl Pts',(-12.6,4.91740980403444,-0.811862632160295));
#40138=CARTESIAN_POINT('Ctrl Pts',(-12.6,4.9098305906043,-0.843318348590614));
#40139=CARTESIAN_POINT('Ctrl Pts',(-12.6,4.89642338914026,-0.898961738404567));
#40140=CARTESIAN_POINT('Ctrl Pts',(-12.6,4.8816647095724,-0.95423026124531));
#40141=CARTESIAN_POINT('Ctrl Pts',(-12.6,4.86559189236515,-1.00907338768238));
#40142=CARTESIAN_POINT('Ctrl Pts',(-12.6,4.83077712152216,-1.12786717812997));
#40143=CARTESIAN_POINT('Ctrl Pts',(-12.6,4.78979779688126,-1.24467503826931));
#40144=CARTESIAN_POINT('Ctrl Pts',(-12.6,4.74297831680097,-1.35904511124462));
#40145=CARTESIAN_POINT('Ctrl Pts',(-12.6,4.69520358782485,-1.47574865494059));
#40146=CARTESIAN_POINT('Ctrl Pts',(-12.6,4.64134719657638,-1.58991571958614));
#40147=CARTESIAN_POINT('Ctrl Pts',(-12.6,4.58170281408354,-1.70104801874762));
#40148=CARTESIAN_POINT('Ctrl Pts',(-12.6,4.53894557569914,-1.78071537397632));
#40149=CARTESIAN_POINT('Ctrl Pts',(-12.6,4.49321317213389,-1.85882199777155));
#40150=CARTESIAN_POINT('Ctrl Pts',(-12.6,4.44460131475763,-1.9351736094758));
#40151=CARTESIAN_POINT('Ctrl Pts',(-12.6,4.40703843688988,-1.99417127836253));
#40152=CARTESIAN_POINT('Ctrl Pts',(-12.6,4.36775615962475,-2.05212081170236));
#40153=CARTESIAN_POINT('Ctrl Pts',(-12.6,4.32679409915763,-2.10892946550827));
#40154=CARTESIAN_POINT('Ctrl Pts',(-12.6,4.26552386323019,-2.19390272080146));
#40155=CARTESIAN_POINT('Ctrl Pts',(-12.6,4.20049767569927,-2.27631129829982));
#40156=CARTESIAN_POINT('Ctrl Pts',(-12.6,4.13199412674128,-2.35567648544826));
#40157=CARTESIAN_POINT('Ctrl Pts',(-12.6,4.07080391109937,-2.42656876752625));
#40158=CARTESIAN_POINT('Ctrl Pts',(-12.6,4.00683995756574,-2.49503280234516));
#40159=CARTESIAN_POINT('Ctrl Pts',(-12.6,3.94032724264284,-2.5607506800043));
#40160=CARTESIAN_POINT('Ctrl Pts',(-12.6,3.90748575173575,-2.5931997099992));
#40161=CARTESIAN_POINT('Ctrl Pts',(-12.6,3.87402616911567,-2.62497698489842));
#40162=CARTESIAN_POINT('Ctrl Pts',(-12.6,3.83998007956055,-2.65606989143867));
#40163=CARTESIAN_POINT('Ctrl Pts',(-12.6,3.75997804822116,-2.72913248734819));
#40164=CARTESIAN_POINT('Ctrl Pts',(-12.6,3.67673002715616,-2.79842887040651));
#40165=CARTESIAN_POINT('Ctrl Pts',(-12.6,3.59053368325527,-2.86385313140299));
#40166=CARTESIAN_POINT('Ctrl Pts',(-12.6,3.53048820079388,-2.90942851358777));
#40167=CARTESIAN_POINT('Ctrl Pts',(-12.6,3.4690111015832,-2.95312415191365));
#40168=CARTESIAN_POINT('Ctrl Pts',(-12.6,3.40619362993573,-2.9948927862738));
#40169=CARTESIAN_POINT('Ctrl Pts',(-12.6,3.33281523122669,-3.04368359916757));
#40170=CARTESIAN_POINT('Ctrl Pts',(-12.6,3.25759896657405,-3.08984861095697));
#40171=CARTESIAN_POINT('Ctrl Pts',(-12.6,3.18077002699366,-3.13324970066485));
#40172=CARTESIAN_POINT('Ctrl Pts',(-12.6,3.07483187106991,-3.193094746475));
#40173=CARTESIAN_POINT('Ctrl Pts',(-12.6,2.96582853574357,-3.24768272390825));
#40174=CARTESIAN_POINT('Ctrl Pts',(-12.6,2.85437152516411,-3.29666597621036));
#40175=CARTESIAN_POINT('Ctrl Pts',(-12.6,2.76538543218785,-3.33577368438387));
#40176=CARTESIAN_POINT('Ctrl Pts',(-12.6,2.6748342422647,-3.37131051831734));
#40177=CARTESIAN_POINT('Ctrl Pts',(-12.6,2.58301134616202,-3.40311631283128));
#40178=CARTESIAN_POINT('Ctrl Pts',(-12.6,2.46115060033201,-3.44532667653894));
#40179=CARTESIAN_POINT('Ctrl Pts',(-12.6,2.33705407145644,-3.48096305732652));
#40180=CARTESIAN_POINT('Ctrl Pts',(-12.6,2.2114307992263,-3.50965933874659));
#40181=CARTESIAN_POINT('Ctrl Pts',(-12.6,2.11981415277956,-3.53058744404528));
#40182=CARTESIAN_POINT('Ctrl Pts',(-12.6,2.02738809550088,-3.5478233034159));
#40183=CARTESIAN_POINT('Ctrl Pts',(-12.6,1.93449359128411,-3.56138533330371));
#40184=CARTESIAN_POINT('Ctrl Pts',(-12.6,1.84382361703015,-3.57462259541225));
#40185=CARTESIAN_POINT('Ctrl Pts',(-12.6,1.75270509672104,-3.58436050971007));
#40186=CARTESIAN_POINT('Ctrl Pts',(-12.6,1.66144632445628,-3.59062972534713));
#40187=CARTESIAN_POINT('Ctrl Pts',(-12.6,1.61183505842739,-3.59403787688198));
#40188=CARTESIAN_POINT('Ctrl Pts',(-12.6,1.56218231482985,-3.59642109941458));
#40189=CARTESIAN_POINT('Ctrl Pts',(-12.6,1.51253728145747,-3.59778572530998));
#40190=CARTESIAN_POINT('Ctrl Pts',(-12.6,1.44328272851095,-3.59968937105066));
#40191=CARTESIAN_POINT('Ctrl Pts',(-12.6,1.37405002548623,-3.59961389113362));
#40192=CARTESIAN_POINT('Ctrl Pts',(-12.6,1.30479205521246,-3.59756529266946));
#40193=CARTESIAN_POINT('Ctrl Pts',(-12.6,1.22725669285759,-3.59527185519777));
#40194=CARTESIAN_POINT('Ctrl Pts',(-12.6,1.14968867032937,-3.59050647284628));
#40195=CARTESIAN_POINT('Ctrl Pts',(-12.6,1.07202485443785,-3.58322209629984));
#40196=CARTESIAN_POINT('Ctrl Pts',(-12.6,0.994361038546337,-3.57593771975341));
#40197=CARTESIAN_POINT('Ctrl Pts',(-12.6,0.916600758134591,-3.56613439828602));
#40198=CARTESIAN_POINT('Ctrl Pts',(-12.6,0.838694895738728,-3.55370611520755));
#40199=CARTESIAN_POINT('Ctrl Pts',(-12.87044835945,4.833816836034,2.150398813705));
#40200=CARTESIAN_POINT('Ctrl Pts',(-12.85461132379,4.548510437562,2.604657272318));
#40201=CARTESIAN_POINT('Ctrl Pts',(-12.82293725246,3.794830979319,3.397883596158));
#40202=CARTESIAN_POINT('Ctrl Pts',(-12.77542614546,2.291343487621,4.056653234419));
#40203=CARTESIAN_POINT('Ctrl Pts',(-12.72791503846,0.6500910845242,4.081135185525));
#40204=CARTESIAN_POINT('Ctrl Pts',(-12.68040393146,-0.8723606288515,3.467561272573));
#40205=CARTESIAN_POINT('Ctrl Pts',(-12.63289282446,-2.037972680177,2.31184527703));
#40206=CARTESIAN_POINT('Ctrl Pts',(-12.58538171746,-2.664509177573,0.7946828350227));
#40207=CARTESIAN_POINT('Ctrl Pts',(-12.53787061046,-2.654013040306,-0.8467251880981));
#40208=CARTESIAN_POINT('Ctrl Pts',(-12.49035950346,-2.008125483935,-2.355751205884));
#40209=CARTESIAN_POINT('Ctrl Pts',(-12.44284839646,-0.827828292971,-3.496465367642));
#40210=CARTESIAN_POINT('Ctrl Pts',(-12.39533728947,0.7023440434848,-4.090521836345));
#40211=CARTESIAN_POINT('Ctrl Pts',(-12.34782618247,2.343155260531,-4.045042082342));
#40212=CARTESIAN_POINT('Ctrl Pts',(-12.30031507547,3.838072193312,-3.367137752342));
#40213=CARTESIAN_POINT('Ctrl Pts',(-12.25280396847,4.953367790708,-2.162792329864));
#40214=CARTESIAN_POINT('Ctrl Pts',(-12.20529286147,5.51468157619,-0.6203152146922));
#40215=CARTESIAN_POINT('Ctrl Pts',(-12.15778175447,5.434212202017,1.019189818483));
#40216=CARTESIAN_POINT('Ctrl Pts',(-12.12610768314,4.961203081187,2.005852424555));
#40217=CARTESIAN_POINT('Ctrl Pts',(-12.11027064747,4.638247898493,2.434163571038));
#40218=CARTESIAN_POINT('Ctrl Pts',(-12.77687535715,4.696568786966,2.0641973444));
#40219=CARTESIAN_POINT('Ctrl Pts',(-12.76103832148,4.422699258062,2.5002462754));
#40220=CARTESIAN_POINT('Ctrl Pts',(-12.72936425015,3.699231998725,3.261675113968));
#40221=CARTESIAN_POINT('Ctrl Pts',(-12.68185314315,2.256013713854,3.894037134075));
#40222=CARTESIAN_POINT('Ctrl Pts',(-12.63434203615,0.6805529991396,3.917537695058));
#40223=CARTESIAN_POINT('Ctrl Pts',(-12.58683092915,-0.780869302481,3.328559672174));
#40224=CARTESIAN_POINT('Ctrl Pts',(-12.53931982215,-1.899756313399,2.219172021067));
#40225=CARTESIAN_POINT('Ctrl Pts',(-12.49180871515,-2.501177299056,0.7628269636494));
#40226=CARTESIAN_POINT('Ctrl Pts',(-12.44429760815,-2.49110191279,-0.8127831328632));
#40227=CARTESIAN_POINT('Ctrl Pts',(-12.39678650115,-1.871105579949,-2.261317924964));
#40228=CARTESIAN_POINT('Ctrl Pts',(-12.34927539416,-0.7381221018787,-3.356305109859));
#40229=CARTESIAN_POINT('Ctrl Pts',(-12.30176428716,0.730711331834,-3.926548070051));
#40230=CARTESIAN_POINT('Ctrl Pts',(-12.25425318016,2.305748546002,-3.882891429786));
#40231=CARTESIAN_POINT('Ctrl Pts',(-12.20674207316,3.740739833701,-3.232161756375));
#40232=CARTESIAN_POINT('Ctrl Pts',(-12.15923096616,4.81132738969,-2.076094050713));
#40233=CARTESIAN_POINT('Ctrl Pts',(-12.11171985916,5.350140198729,-0.5954490909769));
#40234=CARTESIAN_POINT('Ctrl Pts',(-12.06420875216,5.272896541685,0.9783342993609));
#40235=CARTESIAN_POINT('Ctrl Pts',(-12.03253468083,4.818848592592,1.925445280958));
#40236=CARTESIAN_POINT('Ctrl Pts',(-12.01669764516,4.508839478827,2.33658703081));
#40237=CARTESIAN_POINT('Ctrl Pts',(-12.68330235484,4.559320737899,1.977995875095));
#40238=CARTESIAN_POINT('Ctrl Pts',(-12.66746531917,4.296888078562,2.395835278482));
#40239=CARTESIAN_POINT('Ctrl Pts',(-12.63579124784,3.60363301813,3.125466631779));
#40240=CARTESIAN_POINT('Ctrl Pts',(-12.58828014084,2.220683940088,3.731421033731));
#40241=CARTESIAN_POINT('Ctrl Pts',(-12.54076903384,0.711014913755,3.753940204591));
#40242=CARTESIAN_POINT('Ctrl Pts',(-12.49325792684,-0.6893779761106,3.189558071774));
#40243=CARTESIAN_POINT('Ctrl Pts',(-12.44574681984,-1.76153994662,2.126498765103));
#40244=CARTESIAN_POINT('Ctrl Pts',(-12.39823571284,-2.337845420538,0.7309710922762));
#40245=CARTESIAN_POINT('Ctrl Pts',(-12.35072460584,-2.328190785274,-0.7788410776284));
#40246=CARTESIAN_POINT('Ctrl Pts',(-12.30321349885,-1.734085675964,-2.166884644044));
#40247=CARTESIAN_POINT('Ctrl Pts',(-12.25570239185,-0.6484159107864,-3.216144852076));
#40248=CARTESIAN_POINT('Ctrl Pts',(-12.20819128485,0.7590786201833,-3.762574303757));
#40249=CARTESIAN_POINT('Ctrl Pts',(-12.16068017785,2.268341831473,-3.720740777229));
#40250=CARTESIAN_POINT('Ctrl Pts',(-12.11316907085,3.64340747409,-3.097185760409));
#40251=CARTESIAN_POINT('Ctrl Pts',(-12.06565796385,4.669286988672,-1.989395771562));
#40252=CARTESIAN_POINT('Ctrl Pts',(-12.01814685685,5.185598821268,-0.5705829672616));
#40253=CARTESIAN_POINT('Ctrl Pts',(-11.97063574985,5.111580881353,0.9374787802385));
#40254=CARTESIAN_POINT('Ctrl Pts',(-11.93896167852,4.676494103997,1.84503813736));
#40255=CARTESIAN_POINT('Ctrl Pts',(-11.92312464285,4.379431059162,2.239010490582));
#40256=CARTESIAN_POINT('Ctrl Pts',(-12.58972935253,4.422072688831,1.89179440579));
#40257=CARTESIAN_POINT('Ctrl Pts',(-12.57389231686,4.171076899062,2.291424281564));
#40258=CARTESIAN_POINT('Ctrl Pts',(-12.54221824553,3.508034037536,2.98925814959));
#40259=CARTESIAN_POINT('Ctrl Pts',(-12.49470713853,2.185354166322,3.568804933387));
#40260=CARTESIAN_POINT('Ctrl Pts',(-12.44719603153,0.7414768283704,3.590342714124));
#40261=CARTESIAN_POINT('Ctrl Pts',(-12.39968492453,-0.5978866497401,3.050556471375));
#40262=CARTESIAN_POINT('Ctrl Pts',(-12.35217381753,-1.623323579841,2.03382550914));
#40263=CARTESIAN_POINT('Ctrl Pts',(-12.30466271053,-2.174513542021,0.699115220903));
#40264=CARTESIAN_POINT('Ctrl Pts',(-12.25715160354,-2.165279657758,-0.7448990223935));
#40265=CARTESIAN_POINT('Ctrl Pts',(-12.20964049654,-1.597065771978,-2.072451363124));
#40266=CARTESIAN_POINT('Ctrl Pts',(-12.16212938954,-0.5587097196941,-3.075984594292));
#40267=CARTESIAN_POINT('Ctrl Pts',(-12.11461828254,0.7874459085325,-3.598600537463));
#40268=CARTESIAN_POINT('Ctrl Pts',(-12.06710717554,2.230935116944,-3.558590124673));
#40269=CARTESIAN_POINT('Ctrl Pts',(-12.01959606854,3.546075114479,-2.962209764442));
#40270=CARTESIAN_POINT('Ctrl Pts',(-11.97208496154,4.527246587654,-1.902697492411));
#40271=CARTESIAN_POINT('Ctrl Pts',(-11.92457385454,5.021057443807,-0.5457168435463));
#40272=CARTESIAN_POINT('Ctrl Pts',(-11.87706274754,4.950265221021,0.8966232611161));
#40273=CARTESIAN_POINT('Ctrl Pts',(-11.84538867621,4.534139615403,1.764630993762));
#40274=CARTESIAN_POINT('Ctrl Pts',(-11.82955164055,4.250022639497,2.141433950353));
#40275=CARTESIAN_POINT('',(-11.868972894178,4.52769007505164,1.79999920916443));
#40276=CARTESIAN_POINT('Ctrl Pts',(-12.5996587430957,4.20136493479422,2.27215551093202));
#40277=CARTESIAN_POINT('Ctrl Pts',(-12.5943977786613,4.09860310341828,2.39868269823106));
#40278=CARTESIAN_POINT('Ctrl Pts',(-12.5891758755894,3.98732502091615,2.51830284549381));
#40279=CARTESIAN_POINT('Ctrl Pts',(-12.5785334644535,3.75015247715258,2.74049997081469));
#40280=CARTESIAN_POINT('Ctrl Pts',(-12.5730829185006,3.62515140958853,2.84237580960055));
#40281=CARTESIAN_POINT('Ctrl Pts',(-12.556572201564,3.22841147029478,3.12311372977992));
#40282=CARTESIAN_POINT('Ctrl Pts',(-12.5457361202519,2.93796003113066,3.27451147511612));
#40283=CARTESIAN_POINT('Ctrl Pts',(-12.5280760942906,2.43253160915354,3.45764998533339));
#40284=CARTESIAN_POINT('Ctrl Pts',(-12.5211823286344,2.22577086567203,3.51265613920689));
#40285=CARTESIAN_POINT('Ctrl Pts',(-12.4992511023973,1.56189787140324,3.62639865061708));
#40286=CARTESIAN_POINT('Ctrl Pts',(-12.484922380463,1.15006165872664,3.60587160724037));
#40287=CARTESIAN_POINT('Ctrl Pts',(-12.4639364419627,0.523509741436324,
3.50053912987217));
#40288=CARTESIAN_POINT('Ctrl Pts',(-12.4548990117254,0.241048622196361,
3.41743552208491));
#40289=CARTESIAN_POINT('Ctrl Pts',(-12.4375181030687,-0.238498909654585,
3.20870288645154));
#40290=CARTESIAN_POINT('Ctrl Pts',(-12.4294229188578,-0.440818259230192,
3.09578061643052));
#40291=CARTESIAN_POINT('Ctrl Pts',(-12.4071928908363,-0.984372392936457,
2.72079031597198));
#40292=CARTESIAN_POINT('Ctrl Pts',(-12.3928585057436,-1.31725659785877,
2.39882366289928));
#40293=CARTESIAN_POINT('Ctrl Pts',(-12.3611843204163,-1.84416734655621,
1.60897918648557));
#40294=CARTESIAN_POINT('Ctrl Pts',(-12.3450246572973,-2.02638844346352,
1.1670536115216));
#40295=CARTESIAN_POINT('Ctrl Pts',(-12.3261340790523,-2.14180721490078,
0.595506606229493));
#40296=CARTESIAN_POINT('Ctrl Pts',(-12.3224922447298,-2.15912086449384,
0.482401799479392));
#40297=CARTESIAN_POINT('Ctrl Pts',(-12.3029528758476,-2.2218564421081,-0.120504474255441));
#40298=CARTESIAN_POINT('Ctrl Pts',(-12.2886922857574,-2.1616248015831,-0.521999727125013));
#40299=CARTESIAN_POINT('Ctrl Pts',(-12.2682288883678,-2.02587956750989,
-1.12474793886592));
#40300=CARTESIAN_POINT('Ctrl Pts',(-12.2575770430017,-1.9034310571764,-1.44871120196594));
#40301=CARTESIAN_POINT('Ctrl Pts',(-12.2422350361894,-1.68078614497929,
-1.84942730753048));
#40302=CARTESIAN_POINT('Ctrl Pts',(-12.2382762535475,-1.61966717685923,
-1.94766303165829));
#40303=CARTESIAN_POINT('Ctrl Pts',(-12.218472214655,-1.28838939160236,-2.42686360279675));
#40304=CARTESIAN_POINT('Ctrl Pts',(-12.2031328728078,-0.947551774547012,
-2.75945540978527));
#40305=CARTESIAN_POINT('Ctrl Pts',(-12.180436080769,-0.363277372009374,
-3.14160848430859));
#40306=CARTESIAN_POINT('Ctrl Pts',(-12.1728536629882,-0.159300414696784,
-3.24797575371841));
#40307=CARTESIAN_POINT('Ctrl Pts',(-12.1571553863382,0.26932015198446,-3.42157278122556));
#40308=CARTESIAN_POINT('Ctrl Pts',(-12.14918351821,0.493308904608057,-3.48800886339262));
#40309=CARTESIAN_POINT('Ctrl Pts',(-12.1275974487476,1.13532477107718,-3.61349967260649));
#40310=CARTESIAN_POINT('Ctrl Pts',(-12.1148683059215,1.54872569242995,-3.62168563678726));
#40311=CARTESIAN_POINT('Ctrl Pts',(-12.0846045416093,2.42015504579482,-3.48538716709611));
#40312=CARTESIAN_POINT('Ctrl Pts',(-12.0696896115077,2.86579441032513,-3.32442554417545));
#40313=CARTESIAN_POINT('Ctrl Pts',(-12.0352911704397,3.76528393057223,-2.78522738984507));
#40314=CARTESIAN_POINT('Ctrl Pts',(-12.0189478704682,4.08895246372873,-2.42514526884088));
#40315=CARTESIAN_POINT('Ctrl Pts',(-12.0003638630839,4.42709248004169,-1.97674525807511));
#40316=CARTESIAN_POINT('Ctrl Pts',(-11.9928408103346,4.55088803313591,-1.77452838689738));
#40317=CARTESIAN_POINT('Ctrl Pts',(-11.9685369634296,4.87639280789863,-1.099887590332));
#40318=CARTESIAN_POINT('Ctrl Pts',(-11.9522024910297,4.97231142635138,-0.644603860682317));
#40319=CARTESIAN_POINT('Ctrl Pts',(-11.9337752540346,5.01281190989049,-0.0762115415695516));
#40320=CARTESIAN_POINT('Ctrl Pts',(-11.9281519807879,5.01253713121989,0.101078384455938));
#40321=CARTESIAN_POINT('Ctrl Pts',(-11.9136267266903,4.97870465316466,0.546027495964662));
#40322=CARTESIAN_POINT('Ctrl Pts',(-11.904380454833,4.92766437497361,0.809675408134278));
#40323=CARTESIAN_POINT('Ctrl Pts',(-11.8863722838056,4.76870972989004,1.32058258936207));
#40324=CARTESIAN_POINT('Ctrl Pts',(-11.8775396760734,4.66075207090338,1.5675594124826));
#40325=CARTESIAN_POINT('Ctrl Pts',(-11.8687770177641,4.52712046807184,1.79966253176968));
#40326=CARTESIAN_POINT('',(-12.099082574484,4.87271762261516,1.99920743468592));
#40327=CARTESIAN_POINT('',(-12.1,4.874101615138,2.));
#40328=CARTESIAN_POINT('',(-12.1620549971849,5.40898507946903,-1.21540908076623E-5));
#40329=CARTESIAN_POINT('Ctrl Pts',(-12.1620549971849,5.40898507946903,-1.21540908101445E-5));
#40330=CARTESIAN_POINT('Ctrl Pts',(-12.1569738930589,5.40917196074869,0.174930914237154));
#40331=CARTESIAN_POINT('Ctrl Pts',(-12.1519119116125,5.3979768036158,0.349893835687258));
#40332=CARTESIAN_POINT('Ctrl Pts',(-12.1416589980365,5.35271339118928,0.696450564633029));
#40333=CARTESIAN_POINT('Ctrl Pts',(-12.1364520209065,5.31874370082235,0.867680261306424));
#40334=CARTESIAN_POINT('Ctrl Pts',(-12.120579344798,5.18256318174135,1.37317087302075));
#40335=CARTESIAN_POINT('Ctrl Pts',(-12.1098370351016,5.04719145687279,1.69755110551158));
#40336=CARTESIAN_POINT('Ctrl Pts',(-12.0993394760039,4.87295253544702,1.99931610218236));
#40337=CARTESIAN_POINT('',(-12.5375049769753,-2.58973741874834,-1.59154708263292E-8));
#40338=CARTESIAN_POINT('Ctrl Pts',(-12.5375049769753,-2.58973741874834,
-1.59154705386966E-8));
#40339=CARTESIAN_POINT('Ctrl Pts',(-12.5229809386071,-2.58925208028242,
-0.477750600220128));
#40340=CARTESIAN_POINT('Ctrl Pts',(-12.5081812696076,-2.50269412720891,
-0.95241726371786));
#40341=CARTESIAN_POINT('Ctrl Pts',(-12.4828898262183,-2.20080335467406,
-1.76103220854594));
#40342=CARTESIAN_POINT('Ctrl Pts',(-12.4678568782273,-1.96397912807987,
-2.2454221394074));
#40343=CARTESIAN_POINT('Ctrl Pts',(-12.4378211477566,-1.29369923449151,
-2.96535211887595));
#40344=CARTESIAN_POINT('Ctrl Pts',(-12.4274807844472,-1.0352545554023,-3.18146576343454));
#40345=CARTESIAN_POINT('Ctrl Pts',(-12.4099857148573,-0.539434250315809,
-3.50087276770335));
#40346=CARTESIAN_POINT('Ctrl Pts',(-12.4026593404811,-0.311416064037279,
-3.61872249168621));
#40347=CARTESIAN_POINT('Ctrl Pts',(-12.378286903758,0.467325590917832,-3.93113010406675));
#40348=CARTESIAN_POINT('Ctrl Pts',(-12.3623752784994,0.981654375399767,
-4.00030241540116));
#40349=CARTESIAN_POINT('Ctrl Pts',(-12.3410980017126,1.68519871182383,-3.99775483161553));
#40350=CARTESIAN_POINT('Ctrl Pts',(-12.3332033087745,1.94933834976081,-3.9709602694738));
#40351=CARTESIAN_POINT('Ctrl Pts',(-12.3180516147445,2.45704356521002,-3.8682399238872));
#40352=CARTESIAN_POINT('Ctrl Pts',(-12.3108611512601,2.70001301347965,-3.79447138319196));
#40353=CARTESIAN_POINT('Ctrl Pts',(-12.2944726507626,3.21386326258636,-3.58290739661591));
#40354=CARTESIAN_POINT('Ctrl Pts',(-12.2850438758018,3.47926772047201,-3.43580922523939));
#40355=CARTESIAN_POINT('Ctrl Pts',(-12.2597967792659,4.15128057484633,-2.95764610397139));
#40356=CARTESIAN_POINT('Ctrl Pts',(-12.2445865801277,4.5179805244572,-2.57036434011953));
#40357=CARTESIAN_POINT('Ctrl Pts',(-12.2185641240652,4.99311961089714,-1.81620680963327));
#40358=CARTESIAN_POINT('Ctrl Pts',(-12.2075070265642,5.1435641225043,-1.47995601386522));
#40359=CARTESIAN_POINT('Ctrl Pts',(-12.1845278121184,5.35388368311229,-0.762341942254753));
#40360=CARTESIAN_POINT('Ctrl Pts',(-12.1731517423075,5.40857694496182,-0.382074515354316));
#40361=CARTESIAN_POINT('Ctrl Pts',(-12.1620549971849,5.40898507946903,-1.2154090805426E-5));
#40362=CARTESIAN_POINT('Ctrl Pts',(-12.5995521747198,-2.05308781517742,
1.9999870693724));
#40363=CARTESIAN_POINT('Ctrl Pts',(-12.5888604919629,-2.22886541883401,
1.69465508600805));
#40364=CARTESIAN_POINT('Ctrl Pts',(-12.5783563691698,-2.36455856972317,
1.36606660230804));
#40365=CARTESIAN_POINT('Ctrl Pts',(-12.5578742591034,-2.54469535699154,
0.691070574695697));
#40366=CARTESIAN_POINT('Ctrl Pts',(-12.5480600623093,-2.59009012980526,
0.347196683644455));
#40367=CARTESIAN_POINT('Ctrl Pts',(-12.5375049769753,-2.58973741874834,
-1.59154708263292E-8));
#40368=CARTESIAN_POINT('Ctrl Pts',(-12.8808295573,-1.233284553369,2.380024102084));
#40369=CARTESIAN_POINT('Ctrl Pts',(-12.85374622397,-1.773294892526,1.78028186128));
#40370=CARTESIAN_POINT('Ctrl Pts',(-12.7995795573,-2.426733796392,0.2014420016719));
#40371=CARTESIAN_POINT('Ctrl Pts',(-12.7183295573,-1.698583059424,-2.258550295837));
#40372=CARTESIAN_POINT('Ctrl Pts',(-12.6370795573,0.4155582784152,-3.711366470425));
#40373=CARTESIAN_POINT('Ctrl Pts',(-12.5558295573,2.972804381698,-3.510136505478));
#40374=CARTESIAN_POINT('Ctrl Pts',(-12.4745795573,4.833529694393,-1.744372868486));
#40375=CARTESIAN_POINT('Ctrl Pts',(-12.3933295573,5.168351131249,0.7988617992865));
#40376=CARTESIAN_POINT('Ctrl Pts',(-12.3120795573,3.828047522757,2.986040015375));
#40377=CARTESIAN_POINT('Ctrl Pts',(-12.2308295573,1.41,3.842315305328));
#40378=CARTESIAN_POINT('Ctrl Pts',(-12.1495795573,-1.008047522757,2.986040015375));
#40379=CARTESIAN_POINT('Ctrl Pts',(-12.0683295573,-2.348351131249,0.7988617992864));
#40380=CARTESIAN_POINT('Ctrl Pts',(-11.9870795573,-2.013529694393,-1.744372868486));
#40381=CARTESIAN_POINT('Ctrl Pts',(-11.9058295573,-0.1528043816976,-3.510136505478));
#40382=CARTESIAN_POINT('Ctrl Pts',(-11.8245795573,2.404441721585,-3.711366470425));
#40383=CARTESIAN_POINT('Ctrl Pts',(-11.7433295573,4.518583059424,-2.258550295837));
#40384=CARTESIAN_POINT('Ctrl Pts',(-11.6620795573,5.246733796392,0.2014420016719));
#40385=CARTESIAN_POINT('Ctrl Pts',(-11.60791289063,4.593294892526,1.78028186128));
#40386=CARTESIAN_POINT('Ctrl Pts',(-11.5808295573,4.053284553369,2.380024102084));
#40387=CARTESIAN_POINT('Ctrl Pts',(-12.78725655499,-1.353728408999,2.488472236804));
#40388=CARTESIAN_POINT('Ctrl Pts',(-12.76017322166,-1.918344849396,1.86140215202));
#40389=CARTESIAN_POINT('Ctrl Pts',(-12.70600655499,-2.601558338409,0.210620904237));
#40390=CARTESIAN_POINT('Ctrl Pts',(-12.62475655499,-1.840228698273,-2.361463357323));
#40391=CARTESIAN_POINT('Ctrl Pts',(-12.54350655499,0.3702455651116,-3.880478527159));
#40392=CARTESIAN_POINT('Ctrl Pts',(-12.46225655499,3.04401509758,-3.670079321308));
#40393=CARTESIAN_POINT('Ctrl Pts',(-12.38100655499,4.989526185852,-1.823856930718));
#40394=CARTESIAN_POINT('Ctrl Pts',(-12.29975655499,5.339604090179,0.8352627214266));
#40395=CARTESIAN_POINT('Ctrl Pts',(-12.21850655499,3.938228231968,3.12210186012));
#40396=CARTESIAN_POINT('Ctrl Pts',(-12.13725655499,1.41,4.017394174279));
#40397=CARTESIAN_POINT('Ctrl Pts',(-12.05600655499,-1.118228231968,3.12210186012));
#40398=CARTESIAN_POINT('Ctrl Pts',(-11.97475655499,-2.519604090179,0.8352627214266));
#40399=CARTESIAN_POINT('Ctrl Pts',(-11.89350655499,-2.169526185852,-1.823856930718));
#40400=CARTESIAN_POINT('Ctrl Pts',(-11.81225655499,-0.2240150975802,-3.670079321308));
#40401=CARTESIAN_POINT('Ctrl Pts',(-11.73100655499,2.449754434888,-3.880478527159));
#40402=CARTESIAN_POINT('Ctrl Pts',(-11.64975655499,4.660228698273,-2.361463357323));
#40403=CARTESIAN_POINT('Ctrl Pts',(-11.56850655499,5.421558338409,0.210620904237));
#40404=CARTESIAN_POINT('Ctrl Pts',(-11.51433988833,4.738344849396,1.86140215202));
#40405=CARTESIAN_POINT('Ctrl Pts',(-11.48725655499,4.173728408999,2.488472236804));
#40406=CARTESIAN_POINT('Ctrl Pts',(-12.69368355268,-1.474172264629,2.596920371524));
#40407=CARTESIAN_POINT('Ctrl Pts',(-12.66660021935,-2.063394806267,1.942522442761));
#40408=CARTESIAN_POINT('Ctrl Pts',(-12.61243355268,-2.776382880425,0.219799806802));
#40409=CARTESIAN_POINT('Ctrl Pts',(-12.53118355268,-1.981874337123,-2.464376418808));
#40410=CARTESIAN_POINT('Ctrl Pts',(-12.44993355268,0.3249328518079,-4.049590583892));
#40411=CARTESIAN_POINT('Ctrl Pts',(-12.36868355268,3.115225813463,-3.830022137138));
#40412=CARTESIAN_POINT('Ctrl Pts',(-12.28743355268,5.145522677312,-1.90334099295));
#40413=CARTESIAN_POINT('Ctrl Pts',(-12.20618355268,5.510857049109,0.8716636435667));
#40414=CARTESIAN_POINT('Ctrl Pts',(-12.12493355268,4.048408941179,3.258163704864));
#40415=CARTESIAN_POINT('Ctrl Pts',(-12.04368355268,1.41,4.192473043229));
#40416=CARTESIAN_POINT('Ctrl Pts',(-11.96243355268,-1.228408941179,3.258163704864));
#40417=CARTESIAN_POINT('Ctrl Pts',(-11.88118355268,-2.690857049109,0.8716636435667));
#40418=CARTESIAN_POINT('Ctrl Pts',(-11.79993355268,-2.325522677312,-1.90334099295));
#40419=CARTESIAN_POINT('Ctrl Pts',(-11.71868355268,-0.2952258134628,-3.830022137138));
#40420=CARTESIAN_POINT('Ctrl Pts',(-11.63743355268,2.495067148192,-4.049590583892));
#40421=CARTESIAN_POINT('Ctrl Pts',(-11.55618355268,4.801874337123,-2.464376418808));
#40422=CARTESIAN_POINT('Ctrl Pts',(-11.47493355268,5.596382880425,0.2197998068021));
#40423=CARTESIAN_POINT('Ctrl Pts',(-11.42076688602,4.883394806267,1.942522442761));
#40424=CARTESIAN_POINT('Ctrl Pts',(-11.39368355268,4.294172264629,2.596920371524));
#40425=CARTESIAN_POINT('Ctrl Pts',(-12.60011055037,-1.594616120259,2.705368506244));
#40426=CARTESIAN_POINT('Ctrl Pts',(-12.57302721704,-2.208444763137,2.023642733502));
#40427=CARTESIAN_POINT('Ctrl Pts',(-12.51886055037,-2.951207422442,0.2289787093671));
#40428=CARTESIAN_POINT('Ctrl Pts',(-12.43761055037,-2.123519975972,-2.567289480294));
#40429=CARTESIAN_POINT('Ctrl Pts',(-12.35636055037,0.2796201385043,-4.218702640626));
#40430=CARTESIAN_POINT('Ctrl Pts',(-12.27511055037,3.186436529345,-3.989964952968));
#40431=CARTESIAN_POINT('Ctrl Pts',(-12.19386055037,5.301519168772,-1.982825055182));
#40432=CARTESIAN_POINT('Ctrl Pts',(-12.11261055037,5.682110008039,0.9080645657069));
#40433=CARTESIAN_POINT('Ctrl Pts',(-12.03136055037,4.15858965039,3.394225549609));
#40434=CARTESIAN_POINT('Ctrl Pts',(-11.95011055037,1.41,4.36755191218));
#40435=CARTESIAN_POINT('Ctrl Pts',(-11.86886055037,-1.33858965039,3.394225549609));
#40436=CARTESIAN_POINT('Ctrl Pts',(-11.78761055037,-2.862110008039,0.9080645657069));
#40437=CARTESIAN_POINT('Ctrl Pts',(-11.70636055037,-2.481519168772,-1.982825055182));
#40438=CARTESIAN_POINT('Ctrl Pts',(-11.62511055037,-0.3664365293454,-3.989964952968));
#40439=CARTESIAN_POINT('Ctrl Pts',(-11.54386055037,2.540379861496,-4.218702640626));
#40440=CARTESIAN_POINT('Ctrl Pts',(-11.46261055037,4.943519975972,-2.567289480294));
#40441=CARTESIAN_POINT('Ctrl Pts',(-11.38136055037,5.771207422442,0.2289787093671));
#40442=CARTESIAN_POINT('Ctrl Pts',(-11.32719388371,5.028444763137,2.023642733502));
#40443=CARTESIAN_POINT('Ctrl Pts',(-11.30011055037,4.414616120259,2.705368506244));
#40444=CARTESIAN_POINT('',(-11.7876832506661,-2.5878486596569,-5.29887179826593E-6));
#40445=CARTESIAN_POINT('Ctrl Pts',(-12.0998894289566,4.87211890517844,1.99885431481197));
#40446=CARTESIAN_POINT('Ctrl Pts',(-12.0937922082008,4.77211154257748,2.17227988360039));
#40447=CARTESIAN_POINT('Ctrl Pts',(-12.0877133919531,4.65930703924313,2.33838315054028));
#40448=CARTESIAN_POINT('Ctrl Pts',(-12.0778119832033,4.45330143339801,2.59767923140541));
#40449=CARTESIAN_POINT('Ctrl Pts',(-12.0739356077645,4.366803567629,2.69623016690284));
#40450=CARTESIAN_POINT('Ctrl Pts',(-12.0646933833101,4.14612896190159,2.92357123365445));
#40451=CARTESIAN_POINT('Ctrl Pts',(-12.0594268420084,4.00772376869921,3.04716776291446));
#40452=CARTESIAN_POINT('Ctrl Pts',(-12.0453586268293,3.62722368060808,3.34101391083137));
#40453=CARTESIAN_POINT('Ctrl Pts',(-12.0364406835168,3.3736320493554,3.49487937456582));
#40454=CARTESIAN_POINT('Ctrl Pts',(-12.0188158713715,2.84936850747311,3.74003251133475));
#40455=CARTESIAN_POINT('Ctrl Pts',(-12.0101105720752,2.57938532281085,3.83352968685924));
#40456=CARTESIAN_POINT('Ctrl Pts',(-11.9900579652248,1.92897432069873,3.98426672819469));
#40457=CARTESIAN_POINT('Ctrl Pts',(-11.9793233272875,1.54723787739652,4.01629370329876));
#40458=CARTESIAN_POINT('Ctrl Pts',(-11.9600255472479,0.897272788894044,
3.97448380750347));
#40459=CARTESIAN_POINT('Ctrl Pts',(-11.9519430676385,0.633424037211266,
3.93066159074889));
#40460=CARTESIAN_POINT('Ctrl Pts',(-11.9323441145713,0.0119592206589963,
3.76396287315103));
#40461=CARTESIAN_POINT('Ctrl Pts',(-11.920802393218,-0.339284915436861,
3.61553825063958));
#40462=CARTESIAN_POINT('Ctrl Pts',(-11.9038095250028,-0.834646334145461,
3.31676895563602));
#40463=CARTESIAN_POINT('Ctrl Pts',(-11.8981176061492,-0.997843132716873,
3.20032165284924));
#40464=CARTESIAN_POINT('Ctrl Pts',(-11.8822880191012,-1.41301077947756,
2.85282643357032));
#40465=CARTESIAN_POINT('Ctrl Pts',(-11.8719415770262,-1.6455713910264,2.6002496039973));
#40466=CARTESIAN_POINT('Ctrl Pts',(-11.8496715525867,-2.07002341478387,
2.00537709549404));
#40467=CARTESIAN_POINT('Ctrl Pts',(-11.8377430377454,-2.25134971269181,
1.65483885383838));
#40468=CARTESIAN_POINT('Ctrl Pts',(-11.8210815019123,-2.43545043539192,
1.11533876887965));
#40469=CARTESIAN_POINT('Ctrl Pts',(-11.8159746586501,-2.48156811278056,
0.941863227818844));
#40470=CARTESIAN_POINT('Ctrl Pts',(-11.8032039756127,-2.564338138036,0.513344128743086));
#40471=CARTESIAN_POINT('Ctrl Pts',(-11.7954775775326,-2.58823907296245,
0.25661899120969));
#40472=CARTESIAN_POINT('Ctrl Pts',(-11.7876832506661,-2.5878486596569,-5.29887179842592E-6));
#40473=CARTESIAN_POINT('',(-11.3504675579642,4.87339933796339,1.9995945247564));
#40474=CARTESIAN_POINT('Ctrl Pts',(-11.7876832506661,-2.5878486596569,-5.29887179766264E-6));
#40475=CARTESIAN_POINT('Ctrl Pts',(-11.7846103880981,-2.58769474175568,
-0.101177752701668));
#40476=CARTESIAN_POINT('Ctrl Pts',(-11.7815269200527,-2.58376505817935,
-0.202352194944832));
#40477=CARTESIAN_POINT('Ctrl Pts',(-11.767159506054,-2.5479823868286,-0.67239604341351));
#40478=CARTESIAN_POINT('Ctrl Pts',(-11.7558727561899,-2.46962625916423,
-1.03803395302266));
#40479=CARTESIAN_POINT('Ctrl Pts',(-11.739409292753,-2.27534410088687,-1.5668017565316));
#40480=CARTESIAN_POINT('Ctrl Pts',(-11.7339326675503,-2.19566098586759,
-1.74228097956641));
#40481=CARTESIAN_POINT('Ctrl Pts',(-11.7180626751072,-1.93625154170422,
-2.21673614762035));
#40482=CARTESIAN_POINT('Ctrl Pts',(-11.7074698492726,-1.72910546764613,
-2.4994911803966));
#40483=CARTESIAN_POINT('Ctrl Pts',(-11.6858313890525,-1.24044482313432,
-3.0145296654611));
#40484=CARTESIAN_POINT('Ctrl Pts',(-11.674783142645,-0.95557542103658,-3.24457334198693));
#40485=CARTESIAN_POINT('Ctrl Pts',(-11.6591031158707,-0.496171389039835,
-3.52073443840331));
#40486=CARTESIAN_POINT('Ctrl Pts',(-11.6541761409979,-0.342265379603299,
-3.59982216006299));
#40487=CARTESIAN_POINT('Ctrl Pts',(-11.6342954682843,0.28277475538326,-3.87012213900222));
#40488=CARTESIAN_POINT('Ctrl Pts',(-11.6185640184131,0.78827110550862,-3.98091451149757));
#40489=CARTESIAN_POINT('Ctrl Pts',(-11.5968772493773,1.50366150222837,-4.00270758437244));
#40490=CARTESIAN_POINT('Ctrl Pts',(-11.5906341406035,1.71201481316968,-3.99305911453475));
#40491=CARTESIAN_POINT('Ctrl Pts',(-11.5793022612875,2.09485364618809,-3.94477507739172));
#40492=CARTESIAN_POINT('Ctrl Pts',(-11.5742512658516,2.26873754843006,-3.91066826854337));
#40493=CARTESIAN_POINT('Ctrl Pts',(-11.5609178711529,2.71142962776187,-3.79206837519196));
#40494=CARTESIAN_POINT('Ctrl Pts',(-11.5524721273212,2.97482797321889,-3.69004855288624));
#40495=CARTESIAN_POINT('Ctrl Pts',(-11.5294668643449,3.64940532079589,-3.34508319864017));
#40496=CARTESIAN_POINT('Ctrl Pts',(-11.5147555724654,4.0363775014314,-3.05299883030842));
#40497=CARTESIAN_POINT('Ctrl Pts',(-11.4954218216117,4.48438384752746,-2.56551816049437));
#40498=CARTESIAN_POINT('Ctrl Pts',(-11.4901560986607,4.59955745382197,-2.42076314139875));
#40499=CARTESIAN_POINT('Ctrl Pts',(-11.4788786389411,4.81671518935305,-2.10396141487377));
#40500=CARTESIAN_POINT('Ctrl Pts',(-11.4729223802691,4.91653276679171,-1.93170504376533));
#40501=CARTESIAN_POINT('Ctrl Pts',(-11.454290380336,5.18511036695413,-1.37827510867305));
#40502=CARTESIAN_POINT('Ctrl Pts',(-11.4414116708394,5.30941688375091,-0.974916313639125));
#40503=CARTESIAN_POINT('Ctrl Pts',(-11.4254481468296,5.38618076919228,-0.444564438851801));
#40504=CARTESIAN_POINT('Ctrl Pts',(-11.4219320593781,5.39797400151891,-0.325769559551178));
#40505=CARTESIAN_POINT('Ctrl Pts',(-11.4132876883655,5.41375293817565,-0.0287785142314743));
#40506=CARTESIAN_POINT('Ctrl Pts',(-11.4082243127921,5.41103538845619,0.1491799232229));
#40507=CARTESIAN_POINT('Ctrl Pts',(-11.3969631519055,5.37887832285405,0.532063032413717));
#40508=CARTESIAN_POINT('Ctrl Pts',(-11.3908068906373,5.34561745234865,0.735498453917561));
#40509=CARTESIAN_POINT('Ctrl Pts',(-11.3729998567251,5.206885987424,1.30744332532291));
#40510=CARTESIAN_POINT('Ctrl Pts',(-11.3611849998154,5.06375854791249,1.66721385919644));
#40511=CARTESIAN_POINT('Ctrl Pts',(-11.3497104489445,4.87307889585977,1.99938442467927));
#40512=CARTESIAN_POINT('',(-11.5809291742107,4.52769053405903,1.79999903547473));
#40513=CARTESIAN_POINT('',(-11.58094010768,4.527691453624,1.8));
#40514=CARTESIAN_POINT('Ctrl Pts',(-12.6,0.838694895738739,-3.55370611520755));
#40515=CARTESIAN_POINT('Ctrl Pts',(-12.5887641272916,1.16499951264074,-3.60576132676612));
#40516=CARTESIAN_POINT('Ctrl Pts',(-12.5770742688352,1.49857342709415,-3.61324189296731));
#40517=CARTESIAN_POINT('Ctrl Pts',(-12.5560586802186,2.12250050976799,-3.54138859102167));
#40518=CARTESIAN_POINT('Ctrl Pts',(-12.5471373056311,2.41003699969147,-3.47088661950422));
#40519=CARTESIAN_POINT('Ctrl Pts',(-12.5312999768489,2.8830601113705,-3.29055077504967));
#40520=CARTESIAN_POINT('Ctrl Pts',(-12.524252509136,3.07239137138561,-3.198855098942));
#40521=CARTESIAN_POINT('Ctrl Pts',(-12.5082823089597,3.46377174158328,-2.96588999220409));
#40522=CARTESIAN_POINT('Ctrl Pts',(-12.4993793701387,3.66244680102222,-2.81868848700558));
#40523=CARTESIAN_POINT('Ctrl Pts',(-12.4831637232564,4.01591068624947,-2.49492966001599));
#40524=CARTESIAN_POINT('Ctrl Pts',(-12.4760198719274,4.17110662319851,-2.32115475123233));
#40525=CARTESIAN_POINT('Ctrl Pts',(-12.4618210233891,4.44431682999554,-1.9491374193044));
#40526=CARTESIAN_POINT('Ctrl Pts',(-12.4546689448442,4.56280004195252,-1.75079245288425));
#40527=CARTESIAN_POINT('Ctrl Pts',(-12.439931361403,4.74718694464032,-1.36317401846108));
#40528=CARTESIAN_POINT('Ctrl Pts',(-12.4326747765561,4.81801285202238,-1.17619073207302));
#40529=CARTESIAN_POINT('Ctrl Pts',(-12.4063576468406,5.02342418869175,-0.456144231739891));
#40530=CARTESIAN_POINT('Ctrl Pts',(-12.3930138478682,5.02303169369089,0.00540451688270611));
#40531=CARTESIAN_POINT('Ctrl Pts',(-12.37109085781,4.96184573029325,0.688264102970618));
#40532=CARTESIAN_POINT('Ctrl Pts',(-12.3543545405096,4.86578260011855,1.15343937537345));
#40533=CARTESIAN_POINT('Ctrl Pts',(-12.3206718840845,4.40018540009682,2.05344488795971));
#40534=CARTESIAN_POINT('Ctrl Pts',(-12.3062079707334,4.11491495355461,2.41840678256053));
#40535=CARTESIAN_POINT('Ctrl Pts',(-12.283569485576,3.59309018571064,2.87243781592095));
#40536=CARTESIAN_POINT('Ctrl Pts',(-12.275620302287,3.39923678060795,3.00919228251818));
#40537=CARTESIAN_POINT('Ctrl Pts',(-12.2534491391618,2.83406207826439,3.33094760909004));
#40538=CARTESIAN_POINT('Ctrl Pts',(-12.2391421736313,2.43815303451555,3.47455698907783));
#40539=CARTESIAN_POINT('Ctrl Pts',(-12.2186112866935,1.80552823142804,3.58555148501812));
#40540=CARTESIAN_POINT('Ctrl Pts',(-12.2118094564931,1.57887832476874,3.60279712409267));
#40541=CARTESIAN_POINT('Ctrl Pts',(-12.1967053454351,1.11819157379905,3.59487576428567));
#40542=CARTESIAN_POINT('Ctrl Pts',(-12.1884339995617,0.883728304608525,
3.56799950559569));
#40543=CARTESIAN_POINT('Ctrl Pts',(-12.1722270298538,0.432344853464027,
3.47150505751602));
#40544=CARTESIAN_POINT('Ctrl Pts',(-12.1642973895436,0.214991410747773,
3.40335864083117));
#40545=CARTESIAN_POINT('Ctrl Pts',(-12.1413962581675,-0.432776918877695,
3.12926318578167));
#40546=CARTESIAN_POINT('Ctrl Pts',(-12.1276221440261,-0.83238108666093,
2.85440993772082));
#40547=CARTESIAN_POINT('Ctrl Pts',(-12.1035229055086,-1.30750875863012,
2.36934701595707));
#40548=CARTESIAN_POINT('Ctrl Pts',(-12.0961332943923,-1.43818770144354,
2.21124520291547));
#40549=CARTESIAN_POINT('Ctrl Pts',(-12.0822316782666,-1.67166744080994,
1.87248163943021));
#40550=CARTESIAN_POINT('Ctrl Pts',(-12.0757345443886,-1.77402337804945,
1.69164908071361));
#40551=CARTESIAN_POINT('Ctrl Pts',(-12.0620387872348,-1.95744861598317,
1.29133779792592));
#40552=CARTESIAN_POINT('Ctrl Pts',(-12.0548421196046,-2.03419661200844,
1.06982132872298));
#40553=CARTESIAN_POINT('Ctrl Pts',(-12.039453828938,-2.14304564689331,0.620278177587838));
#40554=CARTESIAN_POINT('Ctrl Pts',(-12.0311096529585,-2.17593528060915,
0.39226898784849));
#40555=CARTESIAN_POINT('Ctrl Pts',(-12.0116777247531,-2.20122601942365,
-0.166762796223493));
#40556=CARTESIAN_POINT('Ctrl Pts',(-12.0010460127369,-2.16959750059823,
-0.498536652134289));
#40557=CARTESIAN_POINT('Ctrl Pts',(-11.982907187648,-2.04047221966708,-1.05040640404938));
#40558=CARTESIAN_POINT('Ctrl Pts',(-11.9753521045416,-1.96414069249687,
-1.2756375235216));
#40559=CARTESIAN_POINT('Ctrl Pts',(-11.9479778753788,-1.62246649619555,
-2.02905179992013));
#40560=CARTESIAN_POINT('Ctrl Pts',(-11.9315011260785,-1.29930195159514,
-2.38930315827996));
#40561=CARTESIAN_POINT('Ctrl Pts',(-11.9132185835915,-0.902958965596291,
-2.76771196422866));
#40562=CARTESIAN_POINT('Ctrl Pts',(-11.905424226119,-0.715482172972858,
-2.9147589836845));
#40563=CARTESIAN_POINT('Ctrl Pts',(-11.8904653614941,-0.322663964575563,
-3.16399053807984));
#40564=CARTESIAN_POINT('Ctrl Pts',(-11.8834656399808,-0.119818097506157,
-3.26644888114137));
#40565=CARTESIAN_POINT('Ctrl Pts',(-11.8652109162172,0.391579322848854,
-3.46696903218546));
#40566=CARTESIAN_POINT('Ctrl Pts',(-11.8537230404663,0.707961006519751,
-3.54453244225553));
#40567=CARTESIAN_POINT('Ctrl Pts',(-11.8225903406543,1.61087350736643,-3.64197055765598));
#40568=CARTESIAN_POINT('Ctrl Pts',(-11.8090370118831,2.08903835372752,-3.5521639461965));
#40569=CARTESIAN_POINT('Ctrl Pts',(-11.7902657153263,2.62742750160701,-3.39322567344847));
#40570=CARTESIAN_POINT('Ctrl Pts',(-11.7827937637485,2.82255766322573,-3.31694616519985));
#40571=CARTESIAN_POINT('Ctrl Pts',(-11.7550408274743,3.52456462877589,-2.96994954477919));
#40572=CARTESIAN_POINT('Ctrl Pts',(-11.7410967124665,3.87591355900122,-2.64504773860041));
#40573=CARTESIAN_POINT('Ctrl Pts',(-11.7183255536125,4.35390464591097,-2.10338343352835));
#40574=CARTESIAN_POINT('Ctrl Pts',(-11.7045749484314,4.55763281573061,-1.78643682230267));
#40575=CARTESIAN_POINT('Ctrl Pts',(-11.6831068936867,4.80739207862655,-1.216534200417));
#40576=CARTESIAN_POINT('Ctrl Pts',(-11.675103963254,4.88319244853192,-0.977067848119014));
#40577=CARTESIAN_POINT('Ctrl Pts',(-11.6603829587993,4.97755178908749,-0.520997395951846));
#40578=CARTESIAN_POINT('Ctrl Pts',(-11.6536275474061,5.00250569713179,-0.305637573116578));
#40579=CARTESIAN_POINT('Ctrl Pts',(-11.6358967036407,5.01682165540191,0.238560233254273));
#40580=CARTESIAN_POINT('Ctrl Pts',(-11.6243174248663,4.98075713161062,0.565332704537782));
#40581=CARTESIAN_POINT('Ctrl Pts',(-11.6020225327239,4.81746533012486,1.20508148978053));
#40582=CARTESIAN_POINT('Ctrl Pts',(-11.5911778370602,4.69177805388506,1.51366930157276));
#40583=CARTESIAN_POINT('Ctrl Pts',(-11.5804418130255,4.52712444913299,1.79965561709499));
#40584=CARTESIAN_POINT('Ctrl Pts',(-12.95827988175,0.2420117051536,-3.405261127007));
#40585=CARTESIAN_POINT('Ctrl Pts',(-12.93620025074,0.871896082256,-3.62130845851));
#40586=CARTESIAN_POINT('Ctrl Pts',(-12.89204098874,2.25346886898,-3.694399003235));
#40587=CARTESIAN_POINT('Ctrl Pts',(-12.82580209574,4.073599630528,-2.695596833396));
#40588=CARTESIAN_POINT('Ctrl Pts',(-12.75956320274,5.094096064764,-0.8877177432058));
#40589=CARTESIAN_POINT('Ctrl Pts',(-12.69332430974,5.008999654046,1.18655771469));
#40590=CARTESIAN_POINT('Ctrl Pts',(-12.62708541674,3.843766347756,2.904733567434));
#40591=CARTESIAN_POINT('Ctrl Pts',(-12.56084652374,1.948124164015,3.751149176974));
#40592=CARTESIAN_POINT('Ctrl Pts',(-12.49460763074,-0.1090192521286,3.47178325432));
#40593=CARTESIAN_POINT('Ctrl Pts',(-12.42836873774,-1.710279489762,2.150477565921));
#40594=CARTESIAN_POINT('Ctrl Pts',(-12.36212984474,-2.375092347213,0.1837780628467));
#40595=CARTESIAN_POINT('Ctrl Pts',(-12.29589095173,-1.903936076344,-1.838076561439));
#40596=CARTESIAN_POINT('Ctrl Pts',(-12.22965205873,-0.4382135835323,-3.308292956026));
#40597=CARTESIAN_POINT('Ctrl Pts',(-12.16341316573,1.582191580049,-3.785639679087));
#40598=CARTESIAN_POINT('Ctrl Pts',(-12.09717427273,3.550907349452,-3.126839031206));
#40599=CARTESIAN_POINT('Ctrl Pts',(-12.03093537973,4.877145604737,-1.529675336636));
#40600=CARTESIAN_POINT('Ctrl Pts',(-11.96469648673,5.162671017333,0.5267674664513));
#40601=CARTESIAN_POINT('Ctrl Pts',(-11.92053722473,4.602606137466,1.79184174217));
#40602=CARTESIAN_POINT('Ctrl Pts',(-11.89845759373,4.176505297397,2.303572972466));
#40603=CARTESIAN_POINT('Ctrl Pts',(-12.8290540207,0.2420117051536,-3.405261127007));
#40604=CARTESIAN_POINT('Ctrl Pts',(-12.8069743897,0.871896082256,-3.62130845851));
#40605=CARTESIAN_POINT('Ctrl Pts',(-12.76281512769,2.25346886898,-3.694399003235));
#40606=CARTESIAN_POINT('Ctrl Pts',(-12.69657623469,4.073599630528,-2.695596833396));
#40607=CARTESIAN_POINT('Ctrl Pts',(-12.63033734169,5.094096064764,-0.8877177432058));
#40608=CARTESIAN_POINT('Ctrl Pts',(-12.56409844869,5.008999654046,1.18655771469));
#40609=CARTESIAN_POINT('Ctrl Pts',(-12.49785955569,3.843766347756,2.904733567434));
#40610=CARTESIAN_POINT('Ctrl Pts',(-12.43162066269,1.948124164015,3.751149176974));
#40611=CARTESIAN_POINT('Ctrl Pts',(-12.36538176969,-0.1090192521286,3.47178325432));
#40612=CARTESIAN_POINT('Ctrl Pts',(-12.29914287669,-1.710279489762,2.150477565921));
#40613=CARTESIAN_POINT('Ctrl Pts',(-12.23290398369,-2.375092347213,0.1837780628467));
#40614=CARTESIAN_POINT('Ctrl Pts',(-12.16666509068,-1.903936076344,-1.838076561439));
#40615=CARTESIAN_POINT('Ctrl Pts',(-12.10042619768,-0.4382135835323,-3.308292956026));
#40616=CARTESIAN_POINT('Ctrl Pts',(-12.03418730468,1.582191580049,-3.785639679087));
#40617=CARTESIAN_POINT('Ctrl Pts',(-11.96794841168,3.550907349452,-3.126839031206));
#40618=CARTESIAN_POINT('Ctrl Pts',(-11.90170951868,4.877145604737,-1.529675336636));
#40619=CARTESIAN_POINT('Ctrl Pts',(-11.83547062568,5.162671017333,0.5267674664513));
#40620=CARTESIAN_POINT('Ctrl Pts',(-11.79131136368,4.602606137466,1.79184174217));
#40621=CARTESIAN_POINT('Ctrl Pts',(-11.76923173268,4.176505297397,2.303572972466));
#40622=CARTESIAN_POINT('Ctrl Pts',(-12.69982815965,0.2420117051536,-3.405261127007));
#40623=CARTESIAN_POINT('Ctrl Pts',(-12.67774852865,0.871896082256,-3.62130845851));
#40624=CARTESIAN_POINT('Ctrl Pts',(-12.63358926664,2.25346886898,-3.694399003235));
#40625=CARTESIAN_POINT('Ctrl Pts',(-12.56735037364,4.073599630528,-2.695596833396));
#40626=CARTESIAN_POINT('Ctrl Pts',(-12.50111148064,5.094096064764,-0.8877177432058));
#40627=CARTESIAN_POINT('Ctrl Pts',(-12.43487258764,5.008999654046,1.18655771469));
#40628=CARTESIAN_POINT('Ctrl Pts',(-12.36863369464,3.843766347756,2.904733567434));
#40629=CARTESIAN_POINT('Ctrl Pts',(-12.30239480164,1.948124164015,3.751149176974));
#40630=CARTESIAN_POINT('Ctrl Pts',(-12.23615590864,-0.1090192521286,3.47178325432));
#40631=CARTESIAN_POINT('Ctrl Pts',(-12.16991701564,-1.710279489762,2.150477565921));
#40632=CARTESIAN_POINT('Ctrl Pts',(-12.10367812264,-2.375092347213,0.1837780628467));
#40633=CARTESIAN_POINT('Ctrl Pts',(-12.03743922964,-1.903936076344,-1.838076561439));
#40634=CARTESIAN_POINT('Ctrl Pts',(-11.97120033663,-0.4382135835323,-3.308292956026));
#40635=CARTESIAN_POINT('Ctrl Pts',(-11.90496144363,1.582191580049,-3.785639679087));
#40636=CARTESIAN_POINT('Ctrl Pts',(-11.83872255063,3.550907349452,-3.126839031206));
#40637=CARTESIAN_POINT('Ctrl Pts',(-11.77248365763,4.877145604737,-1.529675336636));
#40638=CARTESIAN_POINT('Ctrl Pts',(-11.70624476463,5.162671017333,0.5267674664513));
#40639=CARTESIAN_POINT('Ctrl Pts',(-11.66208550263,4.602606137466,1.79184174217));
#40640=CARTESIAN_POINT('Ctrl Pts',(-11.64000587163,4.176505297397,2.303572972466));
#40641=CARTESIAN_POINT('Ctrl Pts',(-12.5706022986,0.2420117051536,-3.405261127007));
#40642=CARTESIAN_POINT('Ctrl Pts',(-12.5485226676,0.871896082256,-3.62130845851));
#40643=CARTESIAN_POINT('Ctrl Pts',(-12.5043634056,2.25346886898,-3.694399003235));
#40644=CARTESIAN_POINT('Ctrl Pts',(-12.43812451259,4.073599630528,-2.695596833396));
#40645=CARTESIAN_POINT('Ctrl Pts',(-12.37188561959,5.094096064764,-0.8877177432058));
#40646=CARTESIAN_POINT('Ctrl Pts',(-12.30564672659,5.008999654046,1.18655771469));
#40647=CARTESIAN_POINT('Ctrl Pts',(-12.23940783359,3.843766347756,2.904733567434));
#40648=CARTESIAN_POINT('Ctrl Pts',(-12.17316894059,1.948124164015,3.751149176974));
#40649=CARTESIAN_POINT('Ctrl Pts',(-12.10693004759,-0.1090192521286,3.47178325432));
#40650=CARTESIAN_POINT('Ctrl Pts',(-12.04069115459,-1.710279489762,2.150477565921));
#40651=CARTESIAN_POINT('Ctrl Pts',(-11.97445226159,-2.375092347213,0.1837780628467));
#40652=CARTESIAN_POINT('Ctrl Pts',(-11.90821336859,-1.903936076344,-1.838076561439));
#40653=CARTESIAN_POINT('Ctrl Pts',(-11.84197447558,-0.4382135835323,-3.308292956026));
#40654=CARTESIAN_POINT('Ctrl Pts',(-11.77573558258,1.582191580049,-3.785639679087));
#40655=CARTESIAN_POINT('Ctrl Pts',(-11.70949668958,3.550907349452,-3.126839031206));
#40656=CARTESIAN_POINT('Ctrl Pts',(-11.64325779658,4.877145604737,-1.529675336636));
#40657=CARTESIAN_POINT('Ctrl Pts',(-11.57701890358,5.162671017333,0.5267674664513));
#40658=CARTESIAN_POINT('Ctrl Pts',(-11.53285964158,4.602606137466,1.79184174217));
#40659=CARTESIAN_POINT('Ctrl Pts',(-11.51078001058,4.176505297397,2.303572972466));
#40660=CARTESIAN_POINT('',(-11.86905989232,4.527691453624,1.8));
#40661=CARTESIAN_POINT('Ctrl Pts',(-11.96883879157,4.990278823326,0.3763024677636));
#40662=CARTESIAN_POINT('Ctrl Pts',(-11.94175545824,4.90489850173,1.188641964648));
#40663=CARTESIAN_POINT('Ctrl Pts',(-11.88758879157,4.159906564498,2.74938154341));
#40664=CARTESIAN_POINT('Ctrl Pts',(-11.80633879157,1.816485745292,3.867708124722));
#40665=CARTESIAN_POINT('Ctrl Pts',(-11.72508879157,-0.7080347390856,3.261458897656));
#40666=CARTESIAN_POINT('Ctrl Pts',(-11.64383879157,-2.288549945275,1.201740552274));
#40667=CARTESIAN_POINT('Ctrl Pts',(-11.56258879157,-2.220586231791,-1.393654028254));
#40668=CARTESIAN_POINT('Ctrl Pts',(-11.48133879157,-0.5344423398995,-3.367872149436));
#40669=CARTESIAN_POINT('Ctrl Pts',(-11.40008879157,2.018355591389,-3.841006095744));
#40670=CARTESIAN_POINT('Ctrl Pts',(-11.31883879157,4.300004419211,-2.602171624442));
#40671=CARTESIAN_POINT('Ctrl Pts',(-11.23758879157,5.293554962079,-0.2035285038406));
#40672=CARTESIAN_POINT('Ctrl Pts',(-11.15633879157,4.556173683172,2.285828984956));
#40673=CARTESIAN_POINT('Ctrl Pts',(-11.07508879157,2.416517383734,3.756374013533));
#40674=CARTESIAN_POINT('Ctrl Pts',(-10.99383879157,-0.1717518438912,3.552672808756));
#40675=CARTESIAN_POINT('Ctrl Pts',(-10.91258879157,-2.055021498606,1.765516636523));
#40676=CARTESIAN_POINT('Ctrl Pts',(-10.83133879157,-2.393903084153,-0.8085445604757));
#40677=CARTESIAN_POINT('Ctrl Pts',(-10.75008879157,-1.037354340631,-3.022230916284));
#40678=CARTESIAN_POINT('Ctrl Pts',(-10.66883879157,1.41,-3.888884541858));
#40679=CARTESIAN_POINT('Ctrl Pts',(-10.58758879157,3.857354340631,-3.022230916284));
#40680=CARTESIAN_POINT('Ctrl Pts',(-10.50633879157,5.213903084153,-0.8085445604757));
#40681=CARTESIAN_POINT('Ctrl Pts',(-10.42508879157,4.875021498606,1.765516636523));
#40682=CARTESIAN_POINT('Ctrl Pts',(-10.34383879157,2.991751843891,3.552672808756));
#40683=CARTESIAN_POINT('Ctrl Pts',(-10.26258879157,0.4034826162665,3.756374013533));
#40684=CARTESIAN_POINT('Ctrl Pts',(-10.18133879157,-1.736173683172,2.285828984956));
#40685=CARTESIAN_POINT('Ctrl Pts',(-10.10008879157,-2.473554962079,-0.2035285038406));
#40686=CARTESIAN_POINT('Ctrl Pts',(-10.01883879157,-1.480004419211,-2.602171624442));
#40687=CARTESIAN_POINT('Ctrl Pts',(-9.937588791574,0.8016444086106,-3.841006095744));
#40688=CARTESIAN_POINT('Ctrl Pts',(-9.856338791574,3.3544423399,-3.367872149436));
#40689=CARTESIAN_POINT('Ctrl Pts',(-9.775088791574,5.040586231791,-1.393654028254));
#40690=CARTESIAN_POINT('Ctrl Pts',(-9.693838791574,5.108549945275,1.201740552274));
#40691=CARTESIAN_POINT('Ctrl Pts',(-9.612588791574,3.528034739086,3.261458897656));
#40692=CARTESIAN_POINT('Ctrl Pts',(-9.531338791574,1.003514254708,3.867708124722));
#40693=CARTESIAN_POINT('Ctrl Pts',(-9.450088791574,-1.339906564498,2.74938154341));
#40694=CARTESIAN_POINT('Ctrl Pts',(-9.395922124908,-2.08489850173,1.188641964648));
#40695=CARTESIAN_POINT('Ctrl Pts',(-9.368838791574,-2.170278823326,0.3763024677635));
#40696=CARTESIAN_POINT('Ctrl Pts',(-11.83961293052,4.990278823326,0.3763024677636));
#40697=CARTESIAN_POINT('Ctrl Pts',(-11.81252959719,4.90489850173,1.188641964648));
#40698=CARTESIAN_POINT('Ctrl Pts',(-11.75836293052,4.159906564498,2.74938154341));
#40699=CARTESIAN_POINT('Ctrl Pts',(-11.67711293052,1.816485745292,3.867708124722));
#40700=CARTESIAN_POINT('Ctrl Pts',(-11.59586293052,-0.7080347390856,3.261458897656));
#40701=CARTESIAN_POINT('Ctrl Pts',(-11.51461293052,-2.288549945275,1.201740552274));
#40702=CARTESIAN_POINT('Ctrl Pts',(-11.43336293052,-2.220586231791,-1.393654028254));
#40703=CARTESIAN_POINT('Ctrl Pts',(-11.35211293052,-0.5344423398995,-3.367872149436));
#40704=CARTESIAN_POINT('Ctrl Pts',(-11.27086293052,2.018355591389,-3.841006095744));
#40705=CARTESIAN_POINT('Ctrl Pts',(-11.18961293052,4.300004419211,-2.602171624442));
#40706=CARTESIAN_POINT('Ctrl Pts',(-11.10836293052,5.293554962079,-0.2035285038406));
#40707=CARTESIAN_POINT('Ctrl Pts',(-11.02711293052,4.556173683172,2.285828984956));
#40708=CARTESIAN_POINT('Ctrl Pts',(-10.94586293052,2.416517383734,3.756374013533));
#40709=CARTESIAN_POINT('Ctrl Pts',(-10.86461293052,-0.1717518438912,3.552672808756));
#40710=CARTESIAN_POINT('Ctrl Pts',(-10.78336293052,-2.055021498606,1.765516636523));
#40711=CARTESIAN_POINT('Ctrl Pts',(-10.70211293052,-2.393903084153,-0.8085445604757));
#40712=CARTESIAN_POINT('Ctrl Pts',(-10.62086293052,-1.037354340631,-3.022230916284));
#40713=CARTESIAN_POINT('Ctrl Pts',(-10.53961293052,1.41,-3.888884541858));
#40714=CARTESIAN_POINT('Ctrl Pts',(-10.45836293052,3.857354340631,-3.022230916284));
#40715=CARTESIAN_POINT('Ctrl Pts',(-10.37711293052,5.213903084153,-0.8085445604757));
#40716=CARTESIAN_POINT('Ctrl Pts',(-10.29586293052,4.875021498606,1.765516636523));
#40717=CARTESIAN_POINT('Ctrl Pts',(-10.21461293052,2.991751843891,3.552672808756));
#40718=CARTESIAN_POINT('Ctrl Pts',(-10.13336293052,0.4034826162665,3.756374013533));
#40719=CARTESIAN_POINT('Ctrl Pts',(-10.05211293052,-1.736173683172,2.285828984956));
#40720=CARTESIAN_POINT('Ctrl Pts',(-9.970862930525,-2.473554962079,-0.2035285038406));
#40721=CARTESIAN_POINT('Ctrl Pts',(-9.889612930525,-1.480004419211,-2.602171624442));
#40722=CARTESIAN_POINT('Ctrl Pts',(-9.808362930525,0.8016444086106,-3.841006095744));
#40723=CARTESIAN_POINT('Ctrl Pts',(-9.727112930525,3.3544423399,-3.367872149436));
#40724=CARTESIAN_POINT('Ctrl Pts',(-9.645862930525,5.040586231791,-1.393654028254));
#40725=CARTESIAN_POINT('Ctrl Pts',(-9.564612930525,5.108549945275,1.201740552274));
#40726=CARTESIAN_POINT('Ctrl Pts',(-9.483362930525,3.528034739086,3.261458897656));
#40727=CARTESIAN_POINT('Ctrl Pts',(-9.402112930525,1.003514254708,3.867708124722));
#40728=CARTESIAN_POINT('Ctrl Pts',(-9.320862930525,-1.339906564498,2.74938154341));
#40729=CARTESIAN_POINT('Ctrl Pts',(-9.266696263858,-2.08489850173,1.188641964648));
#40730=CARTESIAN_POINT('Ctrl Pts',(-9.239612930525,-2.170278823326,0.3763024677635));
#40731=CARTESIAN_POINT('Ctrl Pts',(-11.71038706948,4.990278823326,0.3763024677636));
#40732=CARTESIAN_POINT('Ctrl Pts',(-11.68330373614,4.90489850173,1.188641964648));
#40733=CARTESIAN_POINT('Ctrl Pts',(-11.62913706948,4.159906564498,2.74938154341));
#40734=CARTESIAN_POINT('Ctrl Pts',(-11.54788706948,1.816485745292,3.867708124722));
#40735=CARTESIAN_POINT('Ctrl Pts',(-11.46663706948,-0.7080347390856,3.261458897656));
#40736=CARTESIAN_POINT('Ctrl Pts',(-11.38538706948,-2.288549945275,1.201740552274));
#40737=CARTESIAN_POINT('Ctrl Pts',(-11.30413706948,-2.220586231791,-1.393654028254));
#40738=CARTESIAN_POINT('Ctrl Pts',(-11.22288706948,-0.5344423398995,-3.367872149436));
#40739=CARTESIAN_POINT('Ctrl Pts',(-11.14163706948,2.018355591389,-3.841006095744));
#40740=CARTESIAN_POINT('Ctrl Pts',(-11.06038706948,4.300004419211,-2.602171624442));
#40741=CARTESIAN_POINT('Ctrl Pts',(-10.97913706948,5.293554962079,-0.2035285038406));
#40742=CARTESIAN_POINT('Ctrl Pts',(-10.89788706948,4.556173683172,2.285828984956));
#40743=CARTESIAN_POINT('Ctrl Pts',(-10.81663706948,2.416517383734,3.756374013533));
#40744=CARTESIAN_POINT('Ctrl Pts',(-10.73538706948,-0.1717518438912,3.552672808756));
#40745=CARTESIAN_POINT('Ctrl Pts',(-10.65413706948,-2.055021498606,1.765516636523));
#40746=CARTESIAN_POINT('Ctrl Pts',(-10.57288706948,-2.393903084153,-0.8085445604757));
#40747=CARTESIAN_POINT('Ctrl Pts',(-10.49163706948,-1.037354340631,-3.022230916284));
#40748=CARTESIAN_POINT('Ctrl Pts',(-10.41038706948,1.41,-3.888884541858));
#40749=CARTESIAN_POINT('Ctrl Pts',(-10.32913706948,3.857354340631,-3.022230916284));
#40750=CARTESIAN_POINT('Ctrl Pts',(-10.24788706948,5.213903084153,-0.8085445604757));
#40751=CARTESIAN_POINT('Ctrl Pts',(-10.16663706948,4.875021498606,1.765516636523));
#40752=CARTESIAN_POINT('Ctrl Pts',(-10.08538706948,2.991751843891,3.552672808756));
#40753=CARTESIAN_POINT('Ctrl Pts',(-10.00413706948,0.4034826162665,3.756374013533));
#40754=CARTESIAN_POINT('Ctrl Pts',(-9.922887069475,-1.736173683172,2.285828984956));
#40755=CARTESIAN_POINT('Ctrl Pts',(-9.841637069475,-2.473554962079,-0.2035285038406));
#40756=CARTESIAN_POINT('Ctrl Pts',(-9.760387069475,-1.480004419211,-2.602171624442));
#40757=CARTESIAN_POINT('Ctrl Pts',(-9.679137069475,0.8016444086106,-3.841006095744));
#40758=CARTESIAN_POINT('Ctrl Pts',(-9.597887069475,3.3544423399,-3.367872149436));
#40759=CARTESIAN_POINT('Ctrl Pts',(-9.516637069475,5.040586231791,-1.393654028254));
#40760=CARTESIAN_POINT('Ctrl Pts',(-9.435387069475,5.108549945275,1.201740552274));
#40761=CARTESIAN_POINT('Ctrl Pts',(-9.354137069475,3.528034739086,3.261458897656));
#40762=CARTESIAN_POINT('Ctrl Pts',(-9.272887069475,1.003514254708,3.867708124722));
#40763=CARTESIAN_POINT('Ctrl Pts',(-9.191637069475,-1.339906564498,2.74938154341));
#40764=CARTESIAN_POINT('Ctrl Pts',(-9.137470402809,-2.08489850173,1.188641964648));
#40765=CARTESIAN_POINT('Ctrl Pts',(-9.110387069475,-2.170278823326,0.3763024677635));
#40766=CARTESIAN_POINT('Ctrl Pts',(-11.58116120843,4.990278823326,0.3763024677636));
#40767=CARTESIAN_POINT('Ctrl Pts',(-11.55407787509,4.90489850173,1.188641964648));
#40768=CARTESIAN_POINT('Ctrl Pts',(-11.49991120843,4.159906564498,2.74938154341));
#40769=CARTESIAN_POINT('Ctrl Pts',(-11.41866120843,1.816485745292,3.867708124722));
#40770=CARTESIAN_POINT('Ctrl Pts',(-11.33741120843,-0.7080347390856,3.261458897656));
#40771=CARTESIAN_POINT('Ctrl Pts',(-11.25616120843,-2.288549945275,1.201740552274));
#40772=CARTESIAN_POINT('Ctrl Pts',(-11.17491120843,-2.220586231791,-1.393654028254));
#40773=CARTESIAN_POINT('Ctrl Pts',(-11.09366120843,-0.5344423398995,-3.367872149436));
#40774=CARTESIAN_POINT('Ctrl Pts',(-11.01241120843,2.018355591389,-3.841006095744));
#40775=CARTESIAN_POINT('Ctrl Pts',(-10.93116120843,4.300004419211,-2.602171624442));
#40776=CARTESIAN_POINT('Ctrl Pts',(-10.84991120843,5.293554962079,-0.2035285038406));
#40777=CARTESIAN_POINT('Ctrl Pts',(-10.76866120843,4.556173683172,2.285828984956));
#40778=CARTESIAN_POINT('Ctrl Pts',(-10.68741120843,2.416517383734,3.756374013533));
#40779=CARTESIAN_POINT('Ctrl Pts',(-10.60616120843,-0.1717518438912,3.552672808756));
#40780=CARTESIAN_POINT('Ctrl Pts',(-10.52491120843,-2.055021498606,1.765516636523));
#40781=CARTESIAN_POINT('Ctrl Pts',(-10.44366120843,-2.393903084153,-0.8085445604757));
#40782=CARTESIAN_POINT('Ctrl Pts',(-10.36241120843,-1.037354340631,-3.022230916284));
#40783=CARTESIAN_POINT('Ctrl Pts',(-10.28116120843,1.41,-3.888884541858));
#40784=CARTESIAN_POINT('Ctrl Pts',(-10.19991120843,3.857354340631,-3.022230916284));
#40785=CARTESIAN_POINT('Ctrl Pts',(-10.11866120843,5.213903084153,-0.8085445604757));
#40786=CARTESIAN_POINT('Ctrl Pts',(-10.03741120843,4.875021498606,1.765516636523));
#40787=CARTESIAN_POINT('Ctrl Pts',(-9.956161208426,2.991751843891,3.552672808756));
#40788=CARTESIAN_POINT('Ctrl Pts',(-9.874911208426,0.4034826162665,3.756374013533));
#40789=CARTESIAN_POINT('Ctrl Pts',(-9.793661208426,-1.736173683172,2.285828984956));
#40790=CARTESIAN_POINT('Ctrl Pts',(-9.712411208426,-2.473554962079,-0.2035285038406));
#40791=CARTESIAN_POINT('Ctrl Pts',(-9.631161208426,-1.480004419211,-2.602171624442));
#40792=CARTESIAN_POINT('Ctrl Pts',(-9.549911208426,0.8016444086106,-3.841006095744));
#40793=CARTESIAN_POINT('Ctrl Pts',(-9.468661208426,3.3544423399,-3.367872149436));
#40794=CARTESIAN_POINT('Ctrl Pts',(-9.387411208426,5.040586231791,-1.393654028254));
#40795=CARTESIAN_POINT('Ctrl Pts',(-9.306161208426,5.108549945275,1.201740552274));
#40796=CARTESIAN_POINT('Ctrl Pts',(-9.224911208426,3.528034739086,3.261458897656));
#40797=CARTESIAN_POINT('Ctrl Pts',(-9.143661208426,1.003514254708,3.867708124722));
#40798=CARTESIAN_POINT('Ctrl Pts',(-9.062411208426,-1.339906564498,2.74938154341));
#40799=CARTESIAN_POINT('Ctrl Pts',(-9.008244541759,-2.08489850173,1.188641964648));
#40800=CARTESIAN_POINT('Ctrl Pts',(-8.981161208426,-2.170278823326,0.3763024677635));
#40801=CARTESIAN_POINT('',(-9.08094010928004,-1.70769139852697,1.7999999682789));
#40802=CARTESIAN_POINT('Ctrl Pts',(-11.5809617506456,4.5260831847495,1.79907626034106));
#40803=CARTESIAN_POINT('Ctrl Pts',(-11.5684450873295,4.3378600575804,2.1262786819466));
#40804=CARTESIAN_POINT('Ctrl Pts',(-11.5538980982549,4.06794174588371,2.48158171780862));
#40805=CARTESIAN_POINT('Ctrl Pts',(-11.5214314833192,3.30533424391916,3.09434306772659));
#40806=CARTESIAN_POINT('Ctrl Pts',(-11.5058149680683,2.87955875891145,3.31694181014995));
#40807=CARTESIAN_POINT('Ctrl Pts',(-11.4743697636094,1.97084917822777,3.58784773144761));
#40808=CARTESIAN_POINT('Ctrl Pts',(-11.458927499448,1.49858395212458,3.62974369515122));
#40809=CARTESIAN_POINT('Ctrl Pts',(-11.4278797681144,0.567783349223922,
3.52751529061047));
#40810=CARTESIAN_POINT('Ctrl Pts',(-11.4125981009723,0.118590523682951,
3.39023797385841));
#40811=CARTESIAN_POINT('Ctrl Pts',(-11.3789404175473,-0.776750715579688,
2.91391088646765));
#40812=CARTESIAN_POINT('Ctrl Pts',(-11.363281015408,-1.12631120018392,2.58165267968671));
#40813=CARTESIAN_POINT('Ctrl Pts',(-11.3354748649634,-1.65756052459529,
1.93228316468842));
#40814=CARTESIAN_POINT('Ctrl Pts',(-11.3205629146619,-1.87884143765697,
1.53172977266817));
#40815=CARTESIAN_POINT('Ctrl Pts',(-11.2898146617579,-2.16265954300596,
0.650116766645046));
#40816=CARTESIAN_POINT('Ctrl Pts',(-11.2740125696461,-2.21484896790171,
0.166880112239114));
#40817=CARTESIAN_POINT('Ctrl Pts',(-11.2452857971753,-2.14178934307187,
-0.696743368548383));
#40818=CARTESIAN_POINT('Ctrl Pts',(-11.2299872318515,-2.04216345247547,
-1.15659791290261));
#40819=CARTESIAN_POINT('Ctrl Pts',(-11.1965187948146,-1.58161797675723,
-2.05390441834313));
#40820=CARTESIAN_POINT('Ctrl Pts',(-11.1809028018103,-1.28346141477642,
-2.43059522198911));
#40821=CARTESIAN_POINT('Ctrl Pts',(-11.1494553479051,-0.563858309517445,
-3.04814548837911));
#40822=CARTESIAN_POINT('Ctrl Pts',(-11.1340098599798,-0.149535385823463,
-3.27882544829088));
#40823=CARTESIAN_POINT('Ctrl Pts',(-11.1029565216824,0.742348833731377,
-3.56464372425645));
#40824=CARTESIAN_POINT('Ctrl Pts',(-11.0876732494035,1.20855364600226,-3.62224850779717));
#40825=CARTESIAN_POINT('Ctrl Pts',(-11.0540224073665,2.22006102775741,-3.55194694257004));
#40826=CARTESIAN_POINT('Ctrl Pts',(-11.0383675007242,2.67453375101345,-3.39102207324724));
#40827=CARTESIAN_POINT('Ctrl Pts',(-11.0105554436935,3.42438260732585,-3.01428152575009));
#40828=CARTESIAN_POINT('Ctrl Pts',(-10.995646825868,3.78954524063164,-2.73864661536387));
#40829=CARTESIAN_POINT('Ctrl Pts',(-10.9649039633072,4.40784438986543,-2.04929227481183));
#40830=CARTESIAN_POINT('Ctrl Pts',(-10.949101116759,4.65238613785367,-1.62921992321605));
#40831=CARTESIAN_POINT('Ctrl Pts',(-10.920381728934,4.93742752730497,-0.810959839651295));
#40832=CARTESIAN_POINT('Ctrl Pts',(-10.9050839876911,5.0338584634379,-0.350448986549228));
#40833=CARTESIAN_POINT('Ctrl Pts',(-10.8716136041178,4.97891930544053,0.656699056108514));
#40834=CARTESIAN_POINT('Ctrl Pts',(-10.8559955478887,4.86008836875808,1.12224707164084));
#40835=CARTESIAN_POINT('Ctrl Pts',(-10.8245490450561,4.45453566345954,1.97938216415778));
#40836=CARTESIAN_POINT('Ctrl Pts',(-10.8091065245231,4.17024380133705,2.35881196450516));
#40837=CARTESIAN_POINT('Ctrl Pts',(-10.7780497954225,3.47214510051836,2.98330370028508));
#40838=CARTESIAN_POINT('Ctrl Pts',(-10.7627635570628,3.06977273055838,3.22589817344446));
#40839=CARTESIAN_POINT('Ctrl Pts',(-10.7291162063469,2.11747273302227,3.57376459988511));
#40840=CARTESIAN_POINT('Ctrl Pts',(-10.7134646975643,1.63698623022721,3.61203190002298));
#40841=CARTESIAN_POINT('Ctrl Pts',(-10.6856469276413,0.798531261064757,
3.57346703035343));
#40842=CARTESIAN_POINT('Ctrl Pts',(-10.6707424649389,0.352879643376062,
3.47053387849982));
#40843=CARTESIAN_POINT('Ctrl Pts',(-10.6400060097322,-0.492512987916646,
3.09309930974023));
#40844=CARTESIAN_POINT('Ctrl Pts',(-10.6242022843195,-0.887025969969569,
2.8091196588916));
#40845=CARTESIAN_POINT('Ctrl Pts',(-10.5954908481819,-1.48059838918454,
2.17820084892424));
#40846=CARTESIAN_POINT('Ctrl Pts',(-10.5801941864632,-1.75636379133539,
1.7970258246446));
#40847=CARTESIAN_POINT('Ctrl Pts',(-10.546722144091,-2.11671818989919,0.854902102534742));
#40848=CARTESIAN_POINT('Ctrl Pts',(-10.5311017518598,-2.19793715412459,
0.381267556022045));
#40849=CARTESIAN_POINT('Ctrl Pts',(-10.4996563495939,-2.17689468407349,
-0.566708949154503));
#40850=CARTESIAN_POINT('Ctrl Pts',(-10.484217199875,-2.07199190034994,-1.02896894673998));
#40851=CARTESIAN_POINT('Ctrl Pts',(-10.4531565975826,-1.6889857158799,-1.88386424768358));
#40852=CARTESIAN_POINT('Ctrl Pts',(-10.4378669742447,-1.42033608863859,
-2.26946266636307));
#40853=CARTESIAN_POINT('Ctrl Pts',(-10.4042232279263,-0.692530601496339,
-2.97513752621574));
#40854=CARTESIAN_POINT('Ctrl Pts',(-10.388575550876,-0.269500817280129,
-3.20590346729835));
#40855=CARTESIAN_POINT('Ctrl Pts',(-10.3607516492302,0.512062543121538,
-3.51243382004678));
#40856=CARTESIAN_POINT('Ctrl Pts',(-10.3458519718052,0.960835502840228,
-3.6));
#40857=CARTESIAN_POINT('Ctrl Pts',(-10.3160282435544,1.85916449715974,-3.6));
#40858=CARTESIAN_POINT('Ctrl Pts',(-10.3011285661188,2.30793745687843,-3.51243382004679));
#40859=CARTESIAN_POINT('Ctrl Pts',(-10.2733046644732,3.0895008172801,-3.20590346729836));
#40860=CARTESIAN_POINT('Ctrl Pts',(-10.2576569874231,3.51253060149631,-2.97513752621576));
#40861=CARTESIAN_POINT('Ctrl Pts',(-10.2240132411048,4.24033608863857,-2.2694626663631));
#40862=CARTESIAN_POINT('Ctrl Pts',(-10.2087236177669,4.50898571587988,-1.88386424768361));
#40863=CARTESIAN_POINT('Ctrl Pts',(-10.1776630154745,4.89199190034992,-1.02896894674003));
#40864=CARTESIAN_POINT('Ctrl Pts',(-10.1622238657555,4.99689468407348,-0.566708949154548));
#40865=CARTESIAN_POINT('Ctrl Pts',(-10.1307784634897,5.0179371541246,0.38126755602198));
#40866=CARTESIAN_POINT('Ctrl Pts',(-10.1151580712585,4.9367181898992,0.854902102534665));
#40867=CARTESIAN_POINT('Ctrl Pts',(-10.0816860288865,4.57636379133542,1.79702582464447));
#40868=CARTESIAN_POINT('Ctrl Pts',(-10.066389367168,4.30059838918458,2.17820084892409));
#40869=CARTESIAN_POINT('Ctrl Pts',(-10.0376779310305,3.70702596996962,2.80911965889149));
#40870=CARTESIAN_POINT('Ctrl Pts',(-10.021874205618,3.31251298791666,3.09309930974017));
#40871=CARTESIAN_POINT('Ctrl Pts',(-9.99113775041132,2.46712035662394,3.47053387849983));
#40872=CARTESIAN_POINT('Ctrl Pts',(-9.97623328770884,2.02146873893528,3.57346703035345));
#40873=CARTESIAN_POINT('Ctrl Pts',(-9.94841551778588,1.18301376977285,3.61203190002298));
#40874=CARTESIAN_POINT('Ctrl Pts',(-9.93276400900317,0.702527266977886,
3.57376459988507));
#40875=CARTESIAN_POINT('Ctrl Pts',(-9.8991166582872,-0.249772730558297,
3.22589817344437));
#40876=CARTESIAN_POINT('Ctrl Pts',(-9.88383041992763,-0.652145100518404,
2.9833037002849));
#40877=CARTESIAN_POINT('Ctrl Pts',(-9.85277369082696,-1.35024380133725,
2.35881196450481));
#40878=CARTESIAN_POINT('Ctrl Pts',(-9.8373311702941,-1.63453566345976,1.97938216415737));
#40879=CARTESIAN_POINT('Ctrl Pts',(-9.80588466746157,-2.04008836875821,
1.12224707164038));
#40880=CARTESIAN_POINT('Ctrl Pts',(-9.79026661123261,-2.15891930544059,
0.656699056108114));
#40881=CARTESIAN_POINT('Ctrl Pts',(-9.75679622765946,-2.21385846343786,
-0.350448986549525));
#40882=CARTESIAN_POINT('Ctrl Pts',(-9.74149848641643,-2.1174275273049,-0.810959839651566));
#40883=CARTESIAN_POINT('Ctrl Pts',(-9.71277909859132,-1.83238613785356,
-1.6292199232163));
#40884=CARTESIAN_POINT('Ctrl Pts',(-9.69697625204285,-1.58784438986529,
-2.0492922748121));
#40885=CARTESIAN_POINT('Ctrl Pts',(-9.66623338948216,-0.969545240631444,
-2.73864661536413));
#40886=CARTESIAN_POINT('Ctrl Pts',(-9.65132477165689,-0.604382607325644,
-3.01428152575034));
#40887=CARTESIAN_POINT('Ctrl Pts',(-9.62351271462641,0.145466248986811,
-3.39102207324742));
#40888=CARTESIAN_POINT('Ctrl Pts',(-9.60785780798448,0.599938972242795,
-3.55194694257012));
#40889=CARTESIAN_POINT('Ctrl Pts',(-9.57420696594746,1.61144635399806,-3.62224850779716));
#40890=CARTESIAN_POINT('Ctrl Pts',(-9.55892369366837,2.07765116626913,-3.56464372425638));
#40891=CARTESIAN_POINT('Ctrl Pts',(-9.52787035537066,2.96953538582417,-3.27882544829067));
#40892=CARTESIAN_POINT('Ctrl Pts',(-9.51242486744516,3.38385830951819,-3.04814548837884));
#40893=CARTESIAN_POINT('Ctrl Pts',(-9.48097741353986,4.10346141477696,-2.43059522198876));
#40894=CARTESIAN_POINT('Ctrl Pts',(-9.46536142053563,4.40161797675756,-2.05390441834288));
#40895=CARTESIAN_POINT('Ctrl Pts',(-9.43189298349869,4.86216345247558,-1.15659791290247));
#40896=CARTESIAN_POINT('Ctrl Pts',(-9.41659441817477,4.96178934307193,-0.696743368548196));
#40897=CARTESIAN_POINT('Ctrl Pts',(-9.38786764570381,5.03484896790173,0.166880112239431));
#40898=CARTESIAN_POINT('Ctrl Pts',(-9.37206555359201,4.98265954300592,0.650116766645498));
#40899=CARTESIAN_POINT('Ctrl Pts',(-9.34131730068819,4.69884143765681,1.53172977266874));
#40900=CARTESIAN_POINT('Ctrl Pts',(-9.32640535038695,4.47756052459509,1.93228316468901));
#40901=CARTESIAN_POINT('Ctrl Pts',(-9.29859919994251,3.94631120018363,2.58165267968722));
#40902=CARTESIAN_POINT('Ctrl Pts',(-9.28293979780336,3.59675071557947,2.91391088646799));
#40903=CARTESIAN_POINT('Ctrl Pts',(-9.2492821143784,2.70140947631694,3.39023797385853));
#40904=CARTESIAN_POINT('Ctrl Pts',(-9.23400044723609,2.25221665077595,3.52751529061053));
#40905=CARTESIAN_POINT('Ctrl Pts',(-9.20295271590245,1.32141604787522,3.62974369515122));
#40906=CARTESIAN_POINT('Ctrl Pts',(-9.18751045174112,0.849150821771942,
3.58784773144756));
#40907=CARTESIAN_POINT('Ctrl Pts',(-9.15606524728236,-0.0595587589118044,
3.31694181014979));
#40908=CARTESIAN_POINT('Ctrl Pts',(-9.14044873203119,-0.485334243919505,
3.09434306772639));
#40909=CARTESIAN_POINT('Ctrl Pts',(-9.10798160501358,-1.24795377417342,
2.48157205297963));
#40910=CARTESIAN_POINT('Ctrl Pts',(-9.09343435231503,-1.51787189169958,
2.12625850253129));
#40911=CARTESIAN_POINT('Ctrl Pts',(-9.08091840173459,-1.70608413170262,
1.79907461418022));
#40912=CARTESIAN_POINT('',(-9.36905988923136,-1.70769139850482,1.79999996826055));
#40913=CARTESIAN_POINT('',(-9.369059892324,-1.707691453624,1.8));
#40914=CARTESIAN_POINT('Ctrl Pts',(-11.8690815026286,4.52608269350975,1.79907711429981));
#40915=CARTESIAN_POINT('Ctrl Pts',(-11.856564880409,4.3378600965681,2.12627841043079));
#40916=CARTESIAN_POINT('Ctrl Pts',(-11.8420179011084,4.06794217344854,2.48158137425679));
#40917=CARTESIAN_POINT('Ctrl Pts',(-11.8095512679702,3.30533424391916,3.09434306772659));
#40918=CARTESIAN_POINT('Ctrl Pts',(-11.7939347527189,2.87955875891145,3.31694181014995));
#40919=CARTESIAN_POINT('Ctrl Pts',(-11.7624895482601,1.97084917822778,3.58784773144761));
#40920=CARTESIAN_POINT('Ctrl Pts',(-11.7470472840988,1.49858395212459,3.62974369515122));
#40921=CARTESIAN_POINT('Ctrl Pts',(-11.7159995527651,0.567783349223929,
3.52751529061047));
#40922=CARTESIAN_POINT('Ctrl Pts',(-11.7007178856228,0.118590523682957,
3.39023797385841));
#40923=CARTESIAN_POINT('Ctrl Pts',(-11.6670602021978,-0.776750715579682,
2.91391088646765));
#40924=CARTESIAN_POINT('Ctrl Pts',(-11.6514008000586,-1.12631120018392,
2.58165267968671));
#40925=CARTESIAN_POINT('Ctrl Pts',(-11.6235946496142,-1.65756052459529,
1.93228316468843));
#40926=CARTESIAN_POINT('Ctrl Pts',(-11.608682699313,-1.87884143765697,1.53172977266818));
#40927=CARTESIAN_POINT('Ctrl Pts',(-11.5779344464092,-2.16265954300595,
0.65011676664506));
#40928=CARTESIAN_POINT('Ctrl Pts',(-11.5621323542974,-2.21484896790171,
0.166880112239127));
#40929=CARTESIAN_POINT('Ctrl Pts',(-11.5334055818265,-2.14178934307187,
-0.696743368548371));
#40930=CARTESIAN_POINT('Ctrl Pts',(-11.5181070165025,-2.04216345247547,
-1.1565979129026));
#40931=CARTESIAN_POINT('Ctrl Pts',(-11.4846385794655,-1.58161797675724,
-2.05390441834312));
#40932=CARTESIAN_POINT('Ctrl Pts',(-11.4690225864612,-1.28346141477642,
-2.43059522198911));
#40933=CARTESIAN_POINT('Ctrl Pts',(-11.4375751325559,-0.563858309517446,
-3.04814548837911));
#40934=CARTESIAN_POINT('Ctrl Pts',(-11.4221296446305,-0.149535385823461,
-3.27882544829088));
#40935=CARTESIAN_POINT('Ctrl Pts',(-11.3910763063328,0.742348833731382,
-3.56464372425646));
#40936=CARTESIAN_POINT('Ctrl Pts',(-11.3757930340538,1.20855364600227,-3.62224850779717));
#40937=CARTESIAN_POINT('Ctrl Pts',(-11.3421421920168,2.22006102775741,-3.55194694257004));
#40938=CARTESIAN_POINT('Ctrl Pts',(-11.3264872853748,2.67453375101345,-3.39102207324724));
#40939=CARTESIAN_POINT('Ctrl Pts',(-11.2986752283443,3.42438260732584,-3.0142815257501));
#40940=CARTESIAN_POINT('Ctrl Pts',(-11.2837666105191,3.78954524063164,-2.73864661536387));
#40941=CARTESIAN_POINT('Ctrl Pts',(-11.2530237479584,4.40784438986543,-2.04929227481183));
#40942=CARTESIAN_POINT('Ctrl Pts',(-11.2372209014099,4.65238613785367,-1.62921992321605));
#40943=CARTESIAN_POINT('Ctrl Pts',(-11.2085015135848,4.93742752730497,-0.810959839651302));
#40944=CARTESIAN_POINT('Ctrl Pts',(-11.1932037723418,5.0338584634379,-0.350448986549234));
#40945=CARTESIAN_POINT('Ctrl Pts',(-11.1597333887686,4.97891930544053,0.65669905610851));
#40946=CARTESIAN_POINT('Ctrl Pts',(-11.1441153325397,4.86008836875808,1.12224707164084));
#40947=CARTESIAN_POINT('Ctrl Pts',(-11.1126688297072,4.45453566345955,1.97938216415777));
#40948=CARTESIAN_POINT('Ctrl Pts',(-11.0972263091744,4.17024380133706,2.35881196450515));
#40949=CARTESIAN_POINT('Ctrl Pts',(-11.0661695800737,3.47214510051836,2.98330370028508));
#40950=CARTESIAN_POINT('Ctrl Pts',(-11.0508833417141,3.06977273055838,3.22589817344446));
#40951=CARTESIAN_POINT('Ctrl Pts',(-11.0172359909979,2.11747273302226,3.57376459988511));
#40952=CARTESIAN_POINT('Ctrl Pts',(-11.0015844822151,1.6369862302272,3.61203190002299));
#40953=CARTESIAN_POINT('Ctrl Pts',(-10.973766712292,0.798531261064747,3.57346703035343));
#40954=CARTESIAN_POINT('Ctrl Pts',(-10.9588622495894,0.352879643376049,
3.47053387849982));
#40955=CARTESIAN_POINT('Ctrl Pts',(-10.9281257943826,-0.492512987916658,
3.09309930974022));
#40956=CARTESIAN_POINT('Ctrl Pts',(-10.9123220689698,-0.88702596996958,
2.80911965889159));
#40957=CARTESIAN_POINT('Ctrl Pts',(-10.8836106328322,-1.48059838918455,
2.17820084892423));
#40958=CARTESIAN_POINT('Ctrl Pts',(-10.8683139711136,-1.7563637913354,1.79702582464458));
#40959=CARTESIAN_POINT('Ctrl Pts',(-10.8348419287415,-2.11671818989919,
0.854902102534729));
#40960=CARTESIAN_POINT('Ctrl Pts',(-10.8192215365103,-2.1979371541246,0.381267556022032));
#40961=CARTESIAN_POINT('Ctrl Pts',(-10.7877761342445,-2.17689468407348,
-0.566708949154515));
#40962=CARTESIAN_POINT('Ctrl Pts',(-10.7723369845255,-2.07199190034993,
-1.02896894674));
#40963=CARTESIAN_POINT('Ctrl Pts',(-10.7412763822331,-1.68898571587989,
-1.88386424768359));
#40964=CARTESIAN_POINT('Ctrl Pts',(-10.7259867588952,-1.42033608863858,
-2.26946266636308));
#40965=CARTESIAN_POINT('Ctrl Pts',(-10.6923430125769,-0.692530601496336,
-2.97513752621574));
#40966=CARTESIAN_POINT('Ctrl Pts',(-10.6766953355268,-0.269500817280127,
-3.20590346729835));
#40967=CARTESIAN_POINT('Ctrl Pts',(-10.6488714338812,0.512062543121538,
-3.51243382004678));
#40968=CARTESIAN_POINT('Ctrl Pts',(-10.6339717564456,0.960835502840229,
-3.6));
#40969=CARTESIAN_POINT('Ctrl Pts',(-10.6041480281948,1.85916449715974,-3.6));
#40970=CARTESIAN_POINT('Ctrl Pts',(-10.5892483507698,2.30793745687843,-3.51243382004679));
#40971=CARTESIAN_POINT('Ctrl Pts',(-10.561424449124,3.0895008172801,-3.20590346729836));
#40972=CARTESIAN_POINT('Ctrl Pts',(-10.5457767720737,3.51253060149632,-2.97513752621576));
#40973=CARTESIAN_POINT('Ctrl Pts',(-10.5121330257553,4.24033608863857,-2.26946266636309));
#40974=CARTESIAN_POINT('Ctrl Pts',(-10.4968434024174,4.50898571587988,-1.8838642476836));
#40975=CARTESIAN_POINT('Ctrl Pts',(-10.465782800125,4.89199190034993,-1.02896894674001));
#40976=CARTESIAN_POINT('Ctrl Pts',(-10.4503436504061,4.99689468407348,-0.566708949154526));
#40977=CARTESIAN_POINT('Ctrl Pts',(-10.4188982481402,5.01793715412459,0.381267556022008));
#40978=CARTESIAN_POINT('Ctrl Pts',(-10.403277855909,4.93671818989919,0.854902102534692));
#40979=CARTESIAN_POINT('Ctrl Pts',(-10.3698058135368,4.57636379133541,1.7970258246445));
#40980=CARTESIAN_POINT('Ctrl Pts',(-10.3545091518181,4.30059838918456,2.17820084892412));
#40981=CARTESIAN_POINT('Ctrl Pts',(-10.3257977156805,3.70702596996959,2.80911965889151));
#40982=CARTESIAN_POINT('Ctrl Pts',(-10.3099939902678,3.31251298791663,3.09309930974019));
#40983=CARTESIAN_POINT('Ctrl Pts',(-10.2792575350611,2.4671203566239,3.47053387849984));
#40984=CARTESIAN_POINT('Ctrl Pts',(-10.2643530723587,2.02146873893524,3.57346703035346));
#40985=CARTESIAN_POINT('Ctrl Pts',(-10.2365353024357,1.18301376977281,3.61203190002298));
#40986=CARTESIAN_POINT('Ctrl Pts',(-10.2208837936531,0.702527266977845,
3.57376459988506));
#40987=CARTESIAN_POINT('Ctrl Pts',(-10.1872364429371,-0.249772730558337,
3.22589817344435));
#40988=CARTESIAN_POINT('Ctrl Pts',(-10.1719502045775,-0.652145100518445,
2.98330370028487));
#40989=CARTESIAN_POINT('Ctrl Pts',(-10.1408934754768,-1.35024380133728,
2.35881196450477));
#40990=CARTESIAN_POINT('Ctrl Pts',(-10.125450954944,-1.63453566345979,1.97938216415733));
#40991=CARTESIAN_POINT('Ctrl Pts',(-10.0940044521113,-2.04008836875823,
1.12224707164033));
#40992=CARTESIAN_POINT('Ctrl Pts',(-10.0783863958821,-2.1589193054406,0.656699056108066));
#40993=CARTESIAN_POINT('Ctrl Pts',(-10.0449160123088,-2.21385846343786,
-0.350448986549575));
#40994=CARTESIAN_POINT('Ctrl Pts',(-10.0296182710657,-2.11742752730489,
-0.810959839651615));
#40995=CARTESIAN_POINT('Ctrl Pts',(-10.0008988832406,-1.83238613785353,
-1.62921992321635));
#40996=CARTESIAN_POINT('Ctrl Pts',(-9.9850960366923,-1.58784438986525,-2.04929227481215));
#40997=CARTESIAN_POINT('Ctrl Pts',(-9.95435317413131,-0.969545240631397,
-2.73864661536417));
#40998=CARTESIAN_POINT('Ctrl Pts',(-9.93944455630554,-0.604382607325591,
-3.01428152575038));
#40999=CARTESIAN_POINT('Ctrl Pts',(-9.91163249927465,0.14546624898688,-3.39102207324745));
#41000=CARTESIAN_POINT('Ctrl Pts',(-9.89597759263216,0.599938972242873,
-3.55194694257014));
#41001=CARTESIAN_POINT('Ctrl Pts',(-9.86232675059507,1.61144635399815,-3.62224850779715));
#41002=CARTESIAN_POINT('Ctrl Pts',(-9.84704347831627,2.07765116626922,-3.56464372425636));
#41003=CARTESIAN_POINT('Ctrl Pts',(-9.81599014001884,2.96953538582425,-3.27882544829063));
#41004=CARTESIAN_POINT('Ctrl Pts',(-9.80054465209373,3.38385830951826,-3.04814548837879));
#41005=CARTESIAN_POINT('Ctrl Pts',(-9.76909719818853,4.10346141477701,-2.4305952219887));
#41006=CARTESIAN_POINT('Ctrl Pts',(-9.75348120518421,4.40161797675761,-2.05390441834282));
#41007=CARTESIAN_POINT('Ctrl Pts',(-9.72001276814728,4.86216345247561,-1.1565979129024));
#41008=CARTESIAN_POINT('Ctrl Pts',(-9.70471420282341,4.96178934307195,-0.696743368548125));
#41009=CARTESIAN_POINT('Ctrl Pts',(-9.67598743035251,5.03484896790172,0.1668801122395));
#41010=CARTESIAN_POINT('Ctrl Pts',(-9.66018533824078,4.98265954300591,0.650116766645566));
#41011=CARTESIAN_POINT('Ctrl Pts',(-9.6294370853368,4.69884143765678,1.5317297726688));
#41012=CARTESIAN_POINT('Ctrl Pts',(-9.6145251350353,4.47756052459505,1.93228316468907));
#41013=CARTESIAN_POINT('Ctrl Pts',(-9.58671898459069,3.94631120018358,2.58165267968727));
#41014=CARTESIAN_POINT('Ctrl Pts',(-9.5710595824514,3.59675071557941,2.91391088646803));
#41015=CARTESIAN_POINT('Ctrl Pts',(-9.53740189902645,2.70140947631686,3.39023797385856));
#41016=CARTESIAN_POINT('Ctrl Pts',(-9.52212023188427,2.25221665077588,3.52751529061055));
#41017=CARTESIAN_POINT('Ctrl Pts',(-9.49107250055062,1.32141604787514,3.62974369515122));
#41018=CARTESIAN_POINT('Ctrl Pts',(-9.47563023638925,0.849150821771872,
3.58784773144755));
#41019=CARTESIAN_POINT('Ctrl Pts',(-9.44418503193039,-0.0595587589118644,
3.31694181014976));
#41020=CARTESIAN_POINT('Ctrl Pts',(-9.42856851667912,-0.485334243919561,
3.09434306772636));
#41021=CARTESIAN_POINT('Ctrl Pts',(-9.39610138755524,-1.24795382365235,
2.48157201322289));
#41022=CARTESIAN_POINT('Ctrl Pts',(-9.38155413329044,-1.51787195955029,
2.12625841386456));
#41023=CARTESIAN_POINT('Ctrl Pts',(-9.36903818168777,-1.70608420231175,
1.79907449143491));
#41024=CARTESIAN_POINT('Ctrl Pts',(-12.17488944963,5.430961212849,0.4226200533094));
#41025=CARTESIAN_POINT('Ctrl Pts',(-12.14780611629,5.335071764451,1.334947212679));
#41026=CARTESIAN_POINT('Ctrl Pts',(-12.09363944963,4.49838171004,3.087792066179));
#41027=CARTESIAN_POINT('Ctrl Pts',(-12.01238944963,1.86651847134,4.343769052512));
#41028=CARTESIAN_POINT('Ctrl Pts',(-11.93113944963,-0.9687352755443,3.662899000864));
#41029=CARTESIAN_POINT('Ctrl Pts',(-11.84988944963,-2.743789860399,1.349658053758));
#41030=CARTESIAN_POINT('Ctrl Pts',(-11.76863944963,-2.667460761666,-1.565193402042));
#41031=CARTESIAN_POINT('Ctrl Pts',(-11.68738944963,-0.7737760730864,-3.782410239809));
#41032=CARTESIAN_POINT('Ctrl Pts',(-11.60613944963,2.093235680042,-4.313780376177));
#41033=CARTESIAN_POINT('Ctrl Pts',(-11.52488944963,4.655723656744,-2.922462659301));
#41034=CARTESIAN_POINT('Ctrl Pts',(-11.44363944963,5.771566414534,-0.2285800240809));
#41035=CARTESIAN_POINT('Ctrl Pts',(-11.36238944963,4.943423784343,2.56718265288));
#41036=CARTESIAN_POINT('Ctrl Pts',(-11.28113944963,2.540405635919,4.218731264996));
#41037=CARTESIAN_POINT('Ctrl Pts',(-11.19988944963,-0.3664434354111,3.989957282902));
#41038=CARTESIAN_POINT('Ctrl Pts',(-11.11863944963,-2.481517318933,1.982827111076));
#41039=CARTESIAN_POINT('Ctrl Pts',(-11.03738944963,-2.862110501329,-0.9080651192168));
#41040=CARTESIAN_POINT('Ctrl Pts',(-10.95613944963,-1.338589527067,-3.394225391463));
#41041=CARTESIAN_POINT('Ctrl Pts',(-10.87488944963,1.41,-4.367551991253));
#41042=CARTESIAN_POINT('Ctrl Pts',(-10.79363944963,4.158589527067,-3.394225391463));
#41043=CARTESIAN_POINT('Ctrl Pts',(-10.71238944963,5.682110501329,-0.9080651192168));
#41044=CARTESIAN_POINT('Ctrl Pts',(-10.63113944963,5.301517318933,1.982827111076));
#41045=CARTESIAN_POINT('Ctrl Pts',(-10.54988944963,3.186443435411,3.989957282902));
#41046=CARTESIAN_POINT('Ctrl Pts',(-10.46863944963,0.2795943640806,4.218731264996));
#41047=CARTESIAN_POINT('Ctrl Pts',(-10.38738944963,-2.123423784343,2.56718265288));
#41048=CARTESIAN_POINT('Ctrl Pts',(-10.30613944963,-2.951566414534,-0.2285800240809));
#41049=CARTESIAN_POINT('Ctrl Pts',(-10.22488944963,-1.835723656744,-2.922462659301));
#41050=CARTESIAN_POINT('Ctrl Pts',(-10.14363944963,0.7267643199575,-4.313780376177));
#41051=CARTESIAN_POINT('Ctrl Pts',(-10.06238944963,3.593776073086,-3.782410239809));
#41052=CARTESIAN_POINT('Ctrl Pts',(-9.981139449625,5.487460761666,-1.565193402042));
#41053=CARTESIAN_POINT('Ctrl Pts',(-9.899889449625,5.563789860399,1.349658053758));
#41054=CARTESIAN_POINT('Ctrl Pts',(-9.818639449625,3.788735275544,3.662899000864));
#41055=CARTESIAN_POINT('Ctrl Pts',(-9.737389449625,0.9534815286599,4.343769052512));
#41056=CARTESIAN_POINT('Ctrl Pts',(-9.656139449625,-1.67838171004,3.087792066179));
#41057=CARTESIAN_POINT('Ctrl Pts',(-9.601972782958,-2.515071764451,1.334947212679));
#41058=CARTESIAN_POINT('Ctrl Pts',(-9.574889449625,-2.610961212849,0.4226200533094));
#41059=CARTESIAN_POINT('Ctrl Pts',(-12.08131644732,5.269775872549,0.4056787913812));
#41060=CARTESIAN_POINT('Ctrl Pts',(-12.05423311398,5.177730274553,1.281434157126));
#41061=CARTESIAN_POINT('Ctrl Pts',(-12.00006644732,4.37458000429,2.964013997052));
#41062=CARTESIAN_POINT('Ctrl Pts',(-11.91881644732,1.848218348245,4.169643549716));
#41063=CARTESIAN_POINT('Ctrl Pts',(-11.83756644732,-0.8733806489824,3.51606703938));
#41064=CARTESIAN_POINT('Ctrl Pts',(-11.75631644732,-2.577279914956,1.295555295446));
#41065=CARTESIAN_POINT('Ctrl Pts',(-11.67506644732,-2.504010565149,-1.502450635378));
#41066=CARTESIAN_POINT('Ctrl Pts',(-11.59381644732,-0.686236633921,-3.630787518428));
#41067=CARTESIAN_POINT('Ctrl Pts',(-11.51256644732,2.06584730951,-4.140857007583));
#41068=CARTESIAN_POINT('Ctrl Pts',(-11.43131644732,4.5256146991,-2.805312029559));
#41069=CARTESIAN_POINT('Ctrl Pts',(-11.35006644732,5.596727481863,-0.2194171033222));
#41070=CARTESIAN_POINT('Ctrl Pts',(-11.26881644732,4.801782001457,2.464273873707));
#41071=CARTESIAN_POINT('Ctrl Pts',(-11.18756644732,2.495091889415,4.049618060818));
#41072=CARTESIAN_POINT('Ctrl Pts',(-11.10631644732,-0.2952324426901,3.830014774536));
#41073=CARTESIAN_POINT('Ctrl Pts',(-11.02506644732,-2.325520901626,1.903342966431));
#41074=CARTESIAN_POINT('Ctrl Pts',(-10.94381644732,-2.690857522625,-0.8716641748885));
#41075=CARTESIAN_POINT('Ctrl Pts',(-10.86256644732,-1.2284088228,-3.258163553058));
#41076=CARTESIAN_POINT('Ctrl Pts',(-10.78131644732,1.41,-4.192473119132));
#41077=CARTESIAN_POINT('Ctrl Pts',(-10.70006644732,4.0484088228,-3.258163553058));
#41078=CARTESIAN_POINT('Ctrl Pts',(-10.61881644732,5.510857522625,-0.8716641748885));
#41079=CARTESIAN_POINT('Ctrl Pts',(-10.53756644732,5.145520901626,1.903342966431));
#41080=CARTESIAN_POINT('Ctrl Pts',(-10.45631644732,3.11523244269,3.830014774536));
#41081=CARTESIAN_POINT('Ctrl Pts',(-10.37506644732,0.3249081105847,4.049618060818));
#41082=CARTESIAN_POINT('Ctrl Pts',(-10.29381644732,-1.981782001457,2.464273873707));
#41083=CARTESIAN_POINT('Ctrl Pts',(-10.21256644732,-2.776727481863,-0.2194171033222));
#41084=CARTESIAN_POINT('Ctrl Pts',(-10.13131644732,-1.7056146991,-2.805312029559));
#41085=CARTESIAN_POINT('Ctrl Pts',(-10.05006644732,0.7541526904896,-4.140857007583));
#41086=CARTESIAN_POINT('Ctrl Pts',(-9.968816447316,3.506236633921,-3.630787518428));
#41087=CARTESIAN_POINT('Ctrl Pts',(-9.887566447316,5.324010565149,-1.502450635378));
#41088=CARTESIAN_POINT('Ctrl Pts',(-9.806316447316,5.397279914956,1.295555295446));
#41089=CARTESIAN_POINT('Ctrl Pts',(-9.725066447316,3.693380648982,3.51606703938));
#41090=CARTESIAN_POINT('Ctrl Pts',(-9.643816447316,0.9717816517551,4.169643549716));
#41091=CARTESIAN_POINT('Ctrl Pts',(-9.562566447316,-1.55458000429,2.964013997052));
#41092=CARTESIAN_POINT('Ctrl Pts',(-9.50839978065,-2.357730274553,1.281434157126));
#41093=CARTESIAN_POINT('Ctrl Pts',(-9.481316447316,-2.449775872549,0.4056787913812));
#41094=CARTESIAN_POINT('Ctrl Pts',(-11.98774344501,5.10859053225,0.388737529453));
#41095=CARTESIAN_POINT('Ctrl Pts',(-11.96066011167,5.020388784654,1.227921101574));
#41096=CARTESIAN_POINT('Ctrl Pts',(-11.90649344501,4.250778298539,2.840235927925));
#41097=CARTESIAN_POINT('Ctrl Pts',(-11.82524344501,1.82991822515,3.99551804692));
#41098=CARTESIAN_POINT('Ctrl Pts',(-11.74399344501,-0.7780260224205,3.369235077895));
#41099=CARTESIAN_POINT('Ctrl Pts',(-11.66274344501,-2.410769969513,1.241452537133));
#41100=CARTESIAN_POINT('Ctrl Pts',(-11.58149344501,-2.340560368632,-1.439707868714));
#41101=CARTESIAN_POINT('Ctrl Pts',(-11.50024344501,-0.5986971947557,-3.479164797048));
#41102=CARTESIAN_POINT('Ctrl Pts',(-11.41899344501,2.038458938978,-3.967933638989));
#41103=CARTESIAN_POINT('Ctrl Pts',(-11.33774344501,4.395505741456,-2.688161399818));
#41104=CARTESIAN_POINT('Ctrl Pts',(-11.25649344501,5.421888549192,-0.2102541825635));
#41105=CARTESIAN_POINT('Ctrl Pts',(-11.17524344501,4.660140218572,2.361365094534));
#41106=CARTESIAN_POINT('Ctrl Pts',(-11.09399344501,2.449778142911,3.88050485664));
#41107=CARTESIAN_POINT('Ctrl Pts',(-11.01274344501,-0.2240214499691,3.670072266171));
#41108=CARTESIAN_POINT('Ctrl Pts',(-10.93149344501,-2.16952448432,1.823858821786));
#41109=CARTESIAN_POINT('Ctrl Pts',(-10.85024344501,-2.519604543921,-0.8352632305602));
#41110=CARTESIAN_POINT('Ctrl Pts',(-10.76899344501,-1.118228118532,-3.122101714653));
#41111=CARTESIAN_POINT('Ctrl Pts',(-10.68774344501,1.41,-4.017394247012));
#41112=CARTESIAN_POINT('Ctrl Pts',(-10.60649344501,3.938228118532,-3.122101714653));
#41113=CARTESIAN_POINT('Ctrl Pts',(-10.52524344501,5.339604543921,-0.8352632305602));
#41114=CARTESIAN_POINT('Ctrl Pts',(-10.44399344501,4.98952448432,1.823858821786));
#41115=CARTESIAN_POINT('Ctrl Pts',(-10.36274344501,3.044021449969,3.670072266171));
#41116=CARTESIAN_POINT('Ctrl Pts',(-10.28149344501,0.3702218570889,3.88050485664));
#41117=CARTESIAN_POINT('Ctrl Pts',(-10.20024344501,-1.840140218572,2.361365094534));
#41118=CARTESIAN_POINT('Ctrl Pts',(-10.11899344501,-2.601888549192,-0.2102541825635));
#41119=CARTESIAN_POINT('Ctrl Pts',(-10.03774344501,-1.575505741456,-2.688161399818));
#41120=CARTESIAN_POINT('Ctrl Pts',(-9.956493445008,0.7815410610216,-3.967933638989));
#41121=CARTESIAN_POINT('Ctrl Pts',(-9.875243445008,3.418697194756,-3.479164797048));
#41122=CARTESIAN_POINT('Ctrl Pts',(-9.793993445008,5.160560368632,-1.439707868714));
#41123=CARTESIAN_POINT('Ctrl Pts',(-9.712743445008,5.230769969513,1.241452537133));
#41124=CARTESIAN_POINT('Ctrl Pts',(-9.631493445008,3.59802602242,3.369235077895));
#41125=CARTESIAN_POINT('Ctrl Pts',(-9.550243445008,0.9900817748502,3.99551804692));
#41126=CARTESIAN_POINT('Ctrl Pts',(-9.468993445008,-1.430778298539,2.840235927925));
#41127=CARTESIAN_POINT('Ctrl Pts',(-9.414826778341,-2.200388784654,1.227921101574));
#41128=CARTESIAN_POINT('Ctrl Pts',(-9.387743445008,-2.28859053225,0.388737529453));
#41129=CARTESIAN_POINT('Ctrl Pts',(-11.8941704427,4.94740519195,0.3717962675248));
#41130=CARTESIAN_POINT('Ctrl Pts',(-11.86708710937,4.863047294756,1.174408046021));
#41131=CARTESIAN_POINT('Ctrl Pts',(-11.8129204427,4.126976592789,2.716457858798));
#41132=CARTESIAN_POINT('Ctrl Pts',(-11.7316704427,1.811618102055,3.821392544123));
#41133=CARTESIAN_POINT('Ctrl Pts',(-11.6504204427,-0.6826713958586,3.22240311641));
#41134=CARTESIAN_POINT('Ctrl Pts',(-11.5691704427,-2.244260024069,1.187349778821));
#41135=CARTESIAN_POINT('Ctrl Pts',(-11.4879204427,-2.177110172115,-1.37696510205));
#41136=CARTESIAN_POINT('Ctrl Pts',(-11.4066704427,-0.5111577555903,-3.327542075668));
#41137=CARTESIAN_POINT('Ctrl Pts',(-11.3254204427,2.011070568446,-3.795010270395));
#41138=CARTESIAN_POINT('Ctrl Pts',(-11.2441704427,4.265396783812,-2.571010770076));
#41139=CARTESIAN_POINT('Ctrl Pts',(-11.1629204427,5.247049616522,-0.2010912618048));
#41140=CARTESIAN_POINT('Ctrl Pts',(-11.0816704427,4.518498435686,2.258456315361));
#41141=CARTESIAN_POINT('Ctrl Pts',(-11.0004204427,2.404464396407,3.711391652462));
#41142=CARTESIAN_POINT('Ctrl Pts',(-10.9191704427,-0.1528104572481,3.510129757805));
#41143=CARTESIAN_POINT('Ctrl Pts',(-10.8379204427,-2.013528067013,1.744374677141));
#41144=CARTESIAN_POINT('Ctrl Pts',(-10.7566704427,-2.348351565217,-0.7988622862319));
#41145=CARTESIAN_POINT('Ctrl Pts',(-10.6754204427,-1.008047414265,-2.986039876248));
#41146=CARTESIAN_POINT('Ctrl Pts',(-10.5941704427,1.41,-3.842315374891));
#41147=CARTESIAN_POINT('Ctrl Pts',(-10.5129204427,3.828047414265,-2.986039876248));
#41148=CARTESIAN_POINT('Ctrl Pts',(-10.4316704427,5.168351565217,-0.7988622862319));
#41149=CARTESIAN_POINT('Ctrl Pts',(-10.3504204427,4.833528067013,1.744374677141));
#41150=CARTESIAN_POINT('Ctrl Pts',(-10.2691704427,2.972810457248,3.510129757805));
#41151=CARTESIAN_POINT('Ctrl Pts',(-10.1879204427,0.4155356035931,3.711391652462));
#41152=CARTESIAN_POINT('Ctrl Pts',(-10.1066704427,-1.698498435686,2.258456315361));
#41153=CARTESIAN_POINT('Ctrl Pts',(-10.0254204427,-2.427049616522,-0.2010912618048));
#41154=CARTESIAN_POINT('Ctrl Pts',(-9.944170442699,-1.445396783812,-2.571010770076));
#41155=CARTESIAN_POINT('Ctrl Pts',(-9.862920442699,0.8089294315536,-3.795010270395));
#41156=CARTESIAN_POINT('Ctrl Pts',(-9.781670442699,3.33115775559,-3.327542075668));
#41157=CARTESIAN_POINT('Ctrl Pts',(-9.700420442699,4.997110172115,-1.37696510205));
#41158=CARTESIAN_POINT('Ctrl Pts',(-9.619170442699,5.064260024069,1.187349778821));
#41159=CARTESIAN_POINT('Ctrl Pts',(-9.537920442699,3.502671395859,3.22240311641));
#41160=CARTESIAN_POINT('Ctrl Pts',(-9.456670442699,1.008381897945,3.821392544123));
#41161=CARTESIAN_POINT('Ctrl Pts',(-9.375420442699,-1.306976592789,2.716457858798));
#41162=CARTESIAN_POINT('Ctrl Pts',(-9.321253776032,-2.043047294756,1.174408046021));
#41163=CARTESIAN_POINT('Ctrl Pts',(-9.294170442699,-2.12740519195,0.3717962675247));
#41164=CARTESIAN_POINT('',(-9.59950292206818,-2.05335595141186,1.99956949001459));
#41165=CARTESIAN_POINT('',(-9.6,-2.054101615138,2.));
#41166=CARTESIAN_POINT('Ctrl Pts',(-9.60038389030658,-2.0529396754269,1.99929827157929));
#41167=CARTESIAN_POINT('Ctrl Pts',(-9.60356530287706,-2.00039204375156,
2.09076525956697));
#41168=CARTESIAN_POINT('Ctrl Pts',(-9.60671484827216,-1.94423773209052,
2.18016104618138));
#41169=CARTESIAN_POINT('Ctrl Pts',(-9.61408724163892,-1.80249740006208,
2.38692131089865));
#41170=CARTESIAN_POINT('Ctrl Pts',(-9.61822215610905,-1.71422667129878,
2.50151091015392));
#41171=CARTESIAN_POINT('Ctrl Pts',(-9.62752557198061,-1.50197970552175,
2.74767411679855));
#41172=CARTESIAN_POINT('Ctrl Pts',(-9.63270765290204,-1.3754430723976,2.87546943152105));
#41173=CARTESIAN_POINT('Ctrl Pts',(-9.64887550363486,-0.968293782115969,
3.23412919115236));
#41174=CARTESIAN_POINT('Ctrl Pts',(-9.66016975238785,-0.663659725799785,
3.43661940584889));
#41175=CARTESIAN_POINT('Ctrl Pts',(-9.67632979613604,-0.189542768342011,
3.66788018375336));
#41176=CARTESIAN_POINT('Ctrl Pts',(-9.68135338289722,-0.036546137152591,
3.73128585713501));
#41177=CARTESIAN_POINT('Ctrl Pts',(-9.69224736938775,0.309509670573514,
3.85011655992189));
#41178=CARTESIAN_POINT('Ctrl Pts',(-9.69797243888469,0.503018926468948,
3.90055566772882));
#41179=CARTESIAN_POINT('Ctrl Pts',(-9.70781276540716,0.84255087277572,3.96177018746316));
#41180=CARTESIAN_POINT('Ctrl Pts',(-9.71194276219778,0.985825172191182,
3.97951488629265));
#41181=CARTESIAN_POINT('Ctrl Pts',(-9.72745568668193,1.5114670143326,4.01533129444717));
#41182=CARTESIAN_POINT('Ctrl Pts',(-9.73934444916767,1.89643369774521,3.98611924326558));
#41183=CARTESIAN_POINT('Ctrl Pts',(-9.75634099757543,2.43748806067625,3.86761301664057));
#41184=CARTESIAN_POINT('Ctrl Pts',(-9.76158382277774,2.60314950883664,3.82015904654046));
#41185=CARTESIAN_POINT('Ctrl Pts',(-9.77264780072068,2.95189040385358,3.69541703711582));
#41186=CARTESIAN_POINT('Ctrl Pts',(-9.77834886504983,3.13279319787768,3.61499425675465));
#41187=CARTESIAN_POINT('Ctrl Pts',(-9.78809948113757,3.43332706222437,3.4530480553865));
#41188=CARTESIAN_POINT('Ctrl Pts',(-9.79217582267793,3.55518422433439,3.37855139482717));
#41189=CARTESIAN_POINT('Ctrl Pts',(-9.80867298776108,4.01774454336137,3.05977039466347));
#41190=CARTESIAN_POINT('Ctrl Pts',(-9.82175163310386,4.32467416430134,2.76746153256514));
#41191=CARTESIAN_POINT('Ctrl Pts',(-9.83955881259253,4.67970399945409,2.30675385449881));
#41192=CARTESIAN_POINT('Ctrl Pts',(-9.84451574946329,4.77155439973838,2.17143332655518));
#41193=CARTESIAN_POINT('Ctrl Pts',(-9.85484351938631,4.94853306828867,1.87275013717391));
#41194=CARTESIAN_POINT('Ctrl Pts',(-9.86011041467817,5.03082291373801,1.70886404923415));
#41195=CARTESIAN_POINT('Ctrl Pts',(-9.86943108170336,5.15647050662968,1.40756122410476));
#41196=CARTESIAN_POINT('Ctrl Pts',(-9.87349827715893,5.2040919766527,1.27325096319659));
#41197=CARTESIAN_POINT('Ctrl Pts',(-9.88997934009062,5.36250385534211,0.734865045393361));
#41198=CARTESIAN_POINT('Ctrl Pts',(-9.90305133392686,5.41686001613788,0.31476452742291));
#41199=CARTESIAN_POINT('Ctrl Pts',(-9.92084546501746,5.40263864746328,-0.266266922728023));
#41200=CARTESIAN_POINT('Ctrl Pts',(-9.92579666794673,5.38882790792707,-0.429042738008711));
#41201=CARTESIAN_POINT('Ctrl Pts',(-9.93610600141257,5.33841054894495,-0.771919576338839));
#41202=CARTESIAN_POINT('Ctrl Pts',(-9.94136091884868,5.29930430288804,-0.950648946963678));
#41203=CARTESIAN_POINT('Ctrl Pts',(-9.95067177282764,5.20746617111596,-1.26354440945371));
#41204=CARTESIAN_POINT('Ctrl Pts',(-9.9547410020691,5.159936242499,-1.39796426332582));
#41205=CARTESIAN_POINT('Ctrl Pts',(-9.97122325667245,4.94423427933181,-1.91611054506857));
#41206=CARTESIAN_POINT('Ctrl Pts',(-9.98429397417252,4.72213490688853,-2.27678351108641));
#41207=CARTESIAN_POINT('Ctrl Pts',(-10.0020887433787,4.34544430186493,-2.71941947935478));
#41208=CARTESIAN_POINT('Ctrl Pts',(-10.0070414655184,4.2322450932266,-2.83726924033038));
#41209=CARTESIAN_POINT('Ctrl Pts',(-10.0173533129096,3.97723159744509,-3.07206834503773));
#41210=CARTESIAN_POINT('Ctrl Pts',(-10.0226092318958,3.83433887046246,-3.18637976934664));
#41211=CARTESIAN_POINT('Ctrl Pts',(-10.031921004753,3.5660324141649,-3.37176777016096));
#41212=CARTESIAN_POINT('Ctrl Pts',(-10.0359901742059,3.44450475238576,-3.44631916963979));
#41213=CARTESIAN_POINT('Ctrl Pts',(-10.0524713276702,2.95083066874372,-3.71323316974167));
#41214=CARTESIAN_POINT('Ctrl Pts',(-10.0655408566307,2.55128780158735,-3.85375264974307));
#41215=CARTESIAN_POINT('Ctrl Pts',(-10.0833348409095,1.9800155071088,-3.9607014925102));
#41216=CARTESIAN_POINT('Ctrl Pts',(-10.0882878803586,1.8178689752247,-3.98105582710122));
#41217=CARTESIAN_POINT('Ctrl Pts',(-10.0986028994856,1.47181841038385,-4.00306053216985));
#41218=CARTESIAN_POINT('Ctrl Pts',(-10.1038614457517,1.28873662241507,-4.00197013253393));
#41219=CARTESIAN_POINT('Ctrl Pts',(-10.1131761742988,0.963450536031142,
-3.97717099590949));
#41220=CARTESIAN_POINT('Ctrl Pts',(-10.1172456861664,0.822079760251391,
-3.95862047716695));
#41221=CARTESIAN_POINT('Ctrl Pts',(-10.1337210833123,0.270654828968657,
-3.85538213337134));
#41222=CARTESIAN_POINT('Ctrl Pts',(-10.1467835422855,-0.12807379225162,
-3.71323318192157));
#41223=CARTESIAN_POINT('Ctrl Pts',(-10.1645727398934,-0.639225617322842,
-3.43696945479779));
#41224=CARTESIAN_POINT('Ctrl Pts',(-10.1695274186164,-0.778097028999871,
-3.35073195043681));
#41225=CARTESIAN_POINT('Ctrl Pts',(-10.1798510443381,-1.06112010795561,
-3.14991508542845));
#41226=CARTESIAN_POINT('Ctrl Pts',(-10.1851160499579,-1.20289109057113,
-3.03370354506004));
#41227=CARTESIAN_POINT('Ctrl Pts',(-10.1944386818381,-1.44025798266449,
-2.80950825991934));
#41228=CARTESIAN_POINT('Ctrl Pts',(-10.1985096791852,-1.53846870358844,
-2.70607957564346));
#41229=CARTESIAN_POINT('Ctrl Pts',(-10.2149660765781,-1.901540294255,-2.27929208182364));
#41230=CARTESIAN_POINT('Ctrl Pts',(-10.2280047461702,-2.12161193747308,
-1.91856587848559));
#41231=CARTESIAN_POINT('Ctrl Pts',(-10.2457782540083,-2.34500085639878,
-1.38278262607149));
#41232=CARTESIAN_POINT('Ctrl Pts',(-10.2507388319314,-2.39876523335634,
-1.22821628666278));
#41233=CARTESIAN_POINT('Ctrl Pts',(-10.2610940638057,-2.49270795668494,
-0.893073927079879));
#41234=CARTESIAN_POINT('Ctrl Pts',(-10.2663828896523,-2.52991411400295,
-0.712710153376773));
#41235=CARTESIAN_POINT('Ctrl Pts',(-10.2757342916575,-2.57330753149533,
-0.388081751887753));
#41236=CARTESIAN_POINT('Ctrl Pts',(-10.2798103901135,-2.58449302881199,
-0.245736061020243));
#41237=CARTESIAN_POINT('Ctrl Pts',(-10.2961990259462,-2.59773794386555,
0.31202360398641));
#41238=CARTESIAN_POINT('Ctrl Pts',(-10.3091532014495,-2.5423095309823,0.728235535351825));
#41239=CARTESIAN_POINT('Ctrl Pts',(-10.3268709512183,-2.3800745075292,1.28358089222998));
#41240=CARTESIAN_POINT('Ctrl Pts',(-10.331852549475,-2.32455286622402,1.43821007369828));
#41241=CARTESIAN_POINT('Ctrl Pts',(-10.3423194746549,-2.18552130886872,
1.76126220786652));
#41242=CARTESIAN_POINT('Ctrl Pts',(-10.3476922445167,-2.09953324990513,
1.92748599744783));
#41243=CARTESIAN_POINT('Ctrl Pts',(-10.3571458922523,-1.92672997818416,
2.20991504740668));
#41244=CARTESIAN_POINT('Ctrl Pts',(-10.3612408013389,-1.84533486327226,
2.32792924036541));
#41245=CARTESIAN_POINT('Ctrl Pts',(-10.3773779107013,-1.50932128266654,
2.76207457284958));
#41246=CARTESIAN_POINT('Ctrl Pts',(-10.3900198521859,-1.21201226449631,
3.04441768316098));
#41247=CARTESIAN_POINT('Ctrl Pts',(-10.4075335128801,-0.743988086270147,
3.37240036674797));
#41248=CARTESIAN_POINT('Ctrl Pts',(-10.4125957843033,-0.601796957317238,
3.4595532256687));
#41249=CARTESIAN_POINT('Ctrl Pts',(-10.4234767888686,-0.279127871830285,
3.63054871401733));
#41250=CARTESIAN_POINT('Ctrl Pts',(-10.429157275838,-0.0976044409438953,
3.70992203602593));
#41251=CARTESIAN_POINT('Ctrl Pts',(-10.4389963500317,0.227674526330999,
3.82363980065691));
#41252=CARTESIAN_POINT('Ctrl Pts',(-10.4431705301241,0.367777254335285,
3.86402210570016));
#41253=CARTESIAN_POINT('Ctrl Pts',(-10.4582004139136,0.864978434099937,
3.97776706276133));
#41254=CARTESIAN_POINT('Ctrl Pts',(-10.4694924955657,1.23080414723719,4.01002125222356));
#41255=CARTESIAN_POINT('Ctrl Pts',(-10.4871409462028,1.80472053537462,3.98404612758533));
#41256=CARTESIAN_POINT('Ctrl Pts',(-10.493577465914,2.01464812178365,3.95814054182262));
#41257=CARTESIAN_POINT('Ctrl Pts',(-10.5045000912726,2.37481293781915,3.88433901412407));
#41258=CARTESIAN_POINT('Ctrl Pts',(-10.5090183740214,2.52595482119583,3.84390308541401));
#41259=CARTESIAN_POINT('Ctrl Pts',(-10.5166111392828,2.77801443806076,3.75997974605779));
#41260=CARTESIAN_POINT('Ctrl Pts',(-10.5197090386381,2.87987189669372,3.72129811497914));
#41261=CARTESIAN_POINT('Ctrl Pts',(-10.5277070283744,3.13450631164313,3.61227739170519));
#41262=CARTESIAN_POINT('Ctrl Pts',(-10.5326867226591,3.28450323417034,3.5362650427459));
#41263=CARTESIAN_POINT('Ctrl Pts',(-10.5440435692485,3.6088581575327,3.34557807293149));
#41264=CARTESIAN_POINT('Ctrl Pts',(-10.5504678209985,3.7804766845146,3.22585319720809));
#41265=CARTESIAN_POINT('Ctrl Pts',(-10.5655939875803,4.16088617150598,2.91459262974356));
#41266=CARTESIAN_POINT('Ctrl Pts',(-10.5742932160297,4.36131384990957,2.71250670110083));
#41267=CARTESIAN_POINT('Ctrl Pts',(-10.5870541477555,4.63087356683859,2.37551237534754));
#41268=CARTESIAN_POINT('Ctrl Pts',(-10.5913105589387,4.71670929439931,2.25483510527093));
#41269=CARTESIAN_POINT('Ctrl Pts',(-10.6020163495018,4.91630961176043,1.93759246460366));
#41270=CARTESIAN_POINT('Ctrl Pts',(-10.6084882172266,5.01965141413363,1.73663506835275));
#41271=CARTESIAN_POINT('Ctrl Pts',(-10.6205587464262,5.17287461575667,1.3634604433922));
#41272=CARTESIAN_POINT('Ctrl Pts',(-10.6259588258771,5.22918660095898,1.19541593695418));
#41273=CARTESIAN_POINT('Ctrl Pts',(-10.6423653971073,5.36562042592812,0.678895814094211));
#41274=CARTESIAN_POINT('Ctrl Pts',(-10.6534679352852,5.41143141899804,0.321003183428782));
#41275=CARTESIAN_POINT('Ctrl Pts',(-10.6684083871825,5.40786865333887,-0.184422482507212));
#41276=CARTESIAN_POINT('Ctrl Pts',(-10.6726466517092,5.39854196104777,-0.331641454778599));
#41277=CARTESIAN_POINT('Ctrl Pts',(-10.6832935495075,5.35402793405433,-0.701737652690854));
#41278=CARTESIAN_POINT('Ctrl Pts',(-10.689724630813,5.30815987282224,-0.921509015215272));
#41279=CARTESIAN_POINT('Ctrl Pts',(-10.7017378455914,5.19311101656967,-1.30622602262263));
#41280=CARTESIAN_POINT('Ctrl Pts',(-10.7071253608828,5.13135976370246,-1.47193389142936));
#41281=CARTESIAN_POINT('Ctrl Pts',(-10.7235583995194,4.91233815883653,-1.96019232383478));
#41282=CARTESIAN_POINT('Ctrl Pts',(-10.7347025093434,4.72210818287561,-2.26833649793867));
#41283=CARTESIAN_POINT('Ctrl Pts',(-10.749676954179,4.40044025166506,-2.65973903608302));
#41284=CARTESIAN_POINT('Ctrl Pts',(-10.7539120496034,4.30059582846155,-2.76819109251104));
#41285=CARTESIAN_POINT('Ctrl Pts',(-10.7645484338315,4.03332647440469,-3.02751190420293));
#41286=CARTESIAN_POINT('Ctrl Pts',(-10.7709721639332,3.85957691637718,-3.16927194024045));
#41287=CARTESIAN_POINT('Ctrl Pts',(-10.7829750644081,3.52835270750287,-3.39569146699147));
#41288=CARTESIAN_POINT('Ctrl Pts',(-10.7883603277257,3.37614985856842,-3.48559111068736));
#41289=CARTESIAN_POINT('Ctrl Pts',(-10.8047979820205,2.89856072894582,-3.72734106315919));
#41290=CARTESIAN_POINT('Ctrl Pts',(-10.8159494144163,2.55659015861143,-3.84719422135782));
#41291=CARTESIAN_POINT('Ctrl Pts',(-10.8309298036846,2.06008374208132,-3.94896588298085));
#41292=CARTESIAN_POINT('Ctrl Pts',(-10.8351643065083,1.91425722535568,-3.97040873696884));
#41293=CARTESIAN_POINT('Ctrl Pts',(-10.845799102281,1.54340786781898,-4.00373022752363));
#41294=CARTESIAN_POINT('Ctrl Pts',(-10.8522218321573,1.31920204806696,-4.00455379063362));
#41295=CARTESIAN_POINT('Ctrl Pts',(-10.86422325653,0.919348748111904,-3.97207705536693));
#41296=CARTESIAN_POINT('Ctrl Pts',(-10.8696081359326,0.744500468340475,
-3.94616230546156));
#41297=CARTESIAN_POINT('Ctrl Pts',(-10.8860469497402,0.221165463968839,
-3.83348293218832));
#41298=CARTESIAN_POINT('Ctrl Pts',(-10.8972000195863,-0.120070896657474,
-3.71140022738352));
#41299=CARTESIAN_POINT('Ctrl Pts',(-10.9121818333282,-0.570015541435581,
-3.47799933620615));
#41300=CARTESIAN_POINT('Ctrl Pts',(-10.9164162819486,-0.696835886350252,
-3.40289049026002));
#41301=CARTESIAN_POINT('Ctrl Pts',(-10.9270500962871,-1.00597629144814,
-3.1954181329681));
#41302=CARTESIAN_POINT('Ctrl Pts',(-10.933471910365,-1.18070770031624,-3.05498200480715));
#41303=CARTESIAN_POINT('Ctrl Pts',(-10.9454724639931,-1.47099500267918,
-2.77813020528333));
#41304=CARTESIAN_POINT('Ctrl Pts',(-10.9508575091326,-1.59057346493261,
-2.64795208549007));
#41305=CARTESIAN_POINT('Ctrl Pts',(-10.9672957226068,-1.92635978655342,
-2.23105522557671));
#41306=CARTESIAN_POINT('Ctrl Pts',(-10.9784479704523,-2.11471224113583,
-1.92145639935711));
#41307=CARTESIAN_POINT('Ctrl Pts',(-10.9934292463538,-2.31750461921738,
-1.45693204652551));
#41308=CARTESIAN_POINT('Ctrl Pts',(-10.9976638817805,-2.36880024259132,
-1.31874592294464));
#41309=CARTESIAN_POINT('Ctrl Pts',(-11.0082978931886,-2.47849044690317,
-0.962954122100787));
#41310=CARTESIAN_POINT('Ctrl Pts',(-11.0147196930115,-2.52590757199542,
-0.743850529451884));
#41311=CARTESIAN_POINT('Ctrl Pts',(-11.0267188429428,-2.57727552756237,
-0.34605818607726));
#41312=CARTESIAN_POINT('Ctrl Pts',(-11.0321023801037,-2.58828479071026,
-0.169686925643484));
#41313=CARTESIAN_POINT('Ctrl Pts',(-11.0485403456435,-2.58690626763649,
0.365610443292089));
#41314=CARTESIAN_POINT('Ctrl Pts',(-11.0596940741681,-2.53845513269296,
0.724789970060807));
#41315=CARTESIAN_POINT('Ctrl Pts',(-11.0746745975932,-2.40373806791304,
1.21339296651227));
#41316=CARTESIAN_POINT('Ctrl Pts',(-11.0789074289317,-2.35666607982398,
1.35300673589102));
#41317=CARTESIAN_POINT('Ctrl Pts',(-11.0895490982095,-2.21792479375506,
1.69880872528293));
#41318=CARTESIAN_POINT('Ctrl Pts',(-11.0959803388385,-2.11672128528476,
1.89922480552137));
#41319=CARTESIAN_POINT('Ctrl Pts',(-11.1079949941462,-1.90596565912335,
2.24109766425555));
#41320=CARTESIAN_POINT('Ctrl Pts',(-11.1133839304883,-1.80338731043011,
2.38521224645819));
#41321=CARTESIAN_POINT('Ctrl Pts',(-11.1298339556531,-1.46505782436029,
2.80055387367309));
#41322=CARTESIAN_POINT('Ctrl Pts',(-11.1409940587441,-1.20110074462961,
3.04925145424864));
#41323=CARTESIAN_POINT('Ctrl Pts',(-11.1559893263683,-0.788365636720366,
3.3442816688788));
#41324=CARTESIAN_POINT('Ctrl Pts',(-11.1602297731123,-0.663644245149938,
3.42323090938001));
#41325=CARTESIAN_POINT('Ctrl Pts',(-11.1708232940868,-0.339642445151675,
3.6035615679563));
#41326=CARTESIAN_POINT('Ctrl Pts',(-11.1771992020061,-0.136755697950704,
3.69480174137272));
#41327=CARTESIAN_POINT('Ctrl Pts',(-11.1891423376604,0.23977664199463,3.82737754525561));
#41328=CARTESIAN_POINT('Ctrl Pts',(-11.1945206374603,0.40978980570469,3.87489124106396));
#41329=CARTESIAN_POINT('Ctrl Pts',(-11.2109056449069,0.931879281381264,
3.98489475412638));
#41330=CARTESIAN_POINT('Ctrl Pts',(-11.2220100452921,1.29164583404792,4.01254222052902));
#41331=CARTESIAN_POINT('Ctrl Pts',(-11.2369319057045,1.79563625227147,3.9834622357161));
#41332=CARTESIAN_POINT('Ctrl Pts',(-11.2411533761928,1.94160496329731,3.96680896786886));
#41333=CARTESIAN_POINT('Ctrl Pts',(-11.2514157657781,2.29607364367905,3.90602338247599));
#41334=CARTESIAN_POINT('Ctrl Pts',(-11.2574649232284,2.50143665498611,3.85336742407973));
#41335=CARTESIAN_POINT('Ctrl Pts',(-11.2687667488048,2.86029422951289,3.72988603275378));
#41336=CARTESIAN_POINT('Ctrl Pts',(-11.2738366549422,3.01458057559514,3.66573307315122));
#41337=CARTESIAN_POINT('Ctrl Pts',(-11.290025581993,3.48904557328449,3.43329883790693));
#41338=CARTESIAN_POINT('Ctrl Pts',(-11.3012973732444,3.79283470686785,3.2307315058391));
#41339=CARTESIAN_POINT('Ctrl Pts',(-11.3173736352187,4.19739582695453,2.87344615271929));
#41340=CARTESIAN_POINT('Ctrl Pts',(-11.3224917296601,4.32232029305708,2.74716689547289));
#41341=CARTESIAN_POINT('Ctrl Pts',(-11.33179988888,4.53477391826449,2.50096807962284));
#41342=CARTESIAN_POINT('Ctrl Pts',(-11.3360024161493,4.62443130074115,2.38445811548733));
#41343=CARTESIAN_POINT('Ctrl Pts',(-11.3433948737295,4.76619281627191,2.17704619649897));
#41344=CARTESIAN_POINT('Ctrl Pts',(-11.3464900793102,4.82130673923218,2.08917298194309));
#41345=CARTESIAN_POINT('Ctrl Pts',(-11.3496160435307,4.87293858259124,1.99930017380816));
#41346=CARTESIAN_POINT('Ctrl Pts',(-11.6558295573,4.94740519195,0.3717962675248));
#41347=CARTESIAN_POINT('Ctrl Pts',(-11.62874622397,4.863047294756,1.174408046021));
#41348=CARTESIAN_POINT('Ctrl Pts',(-11.5745795573,4.126976592789,2.716457858798));
#41349=CARTESIAN_POINT('Ctrl Pts',(-11.4933295573,1.811618102055,3.821392544123));
#41350=CARTESIAN_POINT('Ctrl Pts',(-11.4120795573,-0.6826713958586,3.22240311641));
#41351=CARTESIAN_POINT('Ctrl Pts',(-11.3308295573,-2.244260024069,1.187349778821));
#41352=CARTESIAN_POINT('Ctrl Pts',(-11.2495795573,-2.177110172115,-1.37696510205));
#41353=CARTESIAN_POINT('Ctrl Pts',(-11.1683295573,-0.5111577555903,-3.327542075668));
#41354=CARTESIAN_POINT('Ctrl Pts',(-11.0870795573,2.011070568446,-3.795010270395));
#41355=CARTESIAN_POINT('Ctrl Pts',(-11.0058295573,4.265396783812,-2.571010770076));
#41356=CARTESIAN_POINT('Ctrl Pts',(-10.9245795573,5.247049616522,-0.2010912618048));
#41357=CARTESIAN_POINT('Ctrl Pts',(-10.8433295573,4.518498435686,2.258456315361));
#41358=CARTESIAN_POINT('Ctrl Pts',(-10.7620795573,2.404464396407,3.711391652462));
#41359=CARTESIAN_POINT('Ctrl Pts',(-10.6808295573,-0.1528104572481,3.510129757805));
#41360=CARTESIAN_POINT('Ctrl Pts',(-10.5995795573,-2.013528067013,1.744374677141));
#41361=CARTESIAN_POINT('Ctrl Pts',(-10.5183295573,-2.348351565217,-0.798862286232));
#41362=CARTESIAN_POINT('Ctrl Pts',(-10.4370795573,-1.008047414265,-2.986039876248));
#41363=CARTESIAN_POINT('Ctrl Pts',(-10.3558295573,1.41,-3.842315374891));
#41364=CARTESIAN_POINT('Ctrl Pts',(-10.2745795573,3.828047414265,-2.986039876248));
#41365=CARTESIAN_POINT('Ctrl Pts',(-10.1933295573,5.168351565217,-0.7988622862319));
#41366=CARTESIAN_POINT('Ctrl Pts',(-10.1120795573,4.833528067013,1.744374677141));
#41367=CARTESIAN_POINT('Ctrl Pts',(-10.0308295573,2.972810457248,3.510129757805));
#41368=CARTESIAN_POINT('Ctrl Pts',(-9.949579557301,0.4155356035931,3.711391652462));
#41369=CARTESIAN_POINT('Ctrl Pts',(-9.868329557301,-1.698498435686,2.258456315361));
#41370=CARTESIAN_POINT('Ctrl Pts',(-9.787079557301,-2.427049616522,-0.2010912618048));
#41371=CARTESIAN_POINT('Ctrl Pts',(-9.705829557301,-1.445396783812,-2.571010770076));
#41372=CARTESIAN_POINT('Ctrl Pts',(-9.624579557301,0.8089294315536,-3.795010270395));
#41373=CARTESIAN_POINT('Ctrl Pts',(-9.543329557301,3.33115775559,-3.327542075668));
#41374=CARTESIAN_POINT('Ctrl Pts',(-9.462079557301,4.997110172115,-1.37696510205));
#41375=CARTESIAN_POINT('Ctrl Pts',(-9.380829557301,5.064260024069,1.187349778821));
#41376=CARTESIAN_POINT('Ctrl Pts',(-9.299579557301,3.502671395859,3.22240311641));
#41377=CARTESIAN_POINT('Ctrl Pts',(-9.218329557301,1.008381897945,3.821392544123));
#41378=CARTESIAN_POINT('Ctrl Pts',(-9.137079557301,-1.306976592789,2.716457858798));
#41379=CARTESIAN_POINT('Ctrl Pts',(-9.082912890634,-2.043047294756,1.174408046021));
#41380=CARTESIAN_POINT('Ctrl Pts',(-9.055829557301,-2.12740519195,0.3717962675247));
#41381=CARTESIAN_POINT('Ctrl Pts',(-11.56225655499,5.10859053225,0.388737529453));
#41382=CARTESIAN_POINT('Ctrl Pts',(-11.53517322166,5.020388784654,1.227921101574));
#41383=CARTESIAN_POINT('Ctrl Pts',(-11.48100655499,4.250778298539,2.840235927925));
#41384=CARTESIAN_POINT('Ctrl Pts',(-11.39975655499,1.82991822515,3.99551804692));
#41385=CARTESIAN_POINT('Ctrl Pts',(-11.31850655499,-0.7780260224205,3.369235077895));
#41386=CARTESIAN_POINT('Ctrl Pts',(-11.23725655499,-2.410769969513,1.241452537133));
#41387=CARTESIAN_POINT('Ctrl Pts',(-11.15600655499,-2.340560368632,-1.439707868714));
#41388=CARTESIAN_POINT('Ctrl Pts',(-11.07475655499,-0.5986971947557,-3.479164797048));
#41389=CARTESIAN_POINT('Ctrl Pts',(-10.99350655499,2.038458938978,-3.967933638989));
#41390=CARTESIAN_POINT('Ctrl Pts',(-10.91225655499,4.395505741456,-2.688161399818));
#41391=CARTESIAN_POINT('Ctrl Pts',(-10.83100655499,5.421888549192,-0.2102541825635));
#41392=CARTESIAN_POINT('Ctrl Pts',(-10.74975655499,4.660140218572,2.361365094534));
#41393=CARTESIAN_POINT('Ctrl Pts',(-10.66850655499,2.449778142911,3.88050485664));
#41394=CARTESIAN_POINT('Ctrl Pts',(-10.58725655499,-0.2240214499691,3.670072266171));
#41395=CARTESIAN_POINT('Ctrl Pts',(-10.50600655499,-2.16952448432,1.823858821786));
#41396=CARTESIAN_POINT('Ctrl Pts',(-10.42475655499,-2.519604543921,-0.8352632305602));
#41397=CARTESIAN_POINT('Ctrl Pts',(-10.34350655499,-1.118228118532,-3.122101714653));
#41398=CARTESIAN_POINT('Ctrl Pts',(-10.26225655499,1.41,-4.017394247012));
#41399=CARTESIAN_POINT('Ctrl Pts',(-10.18100655499,3.938228118532,-3.122101714653));
#41400=CARTESIAN_POINT('Ctrl Pts',(-10.09975655499,5.339604543921,-0.8352632305602));
#41401=CARTESIAN_POINT('Ctrl Pts',(-10.01850655499,4.98952448432,1.823858821786));
#41402=CARTESIAN_POINT('Ctrl Pts',(-9.937256554992,3.044021449969,3.670072266171));
#41403=CARTESIAN_POINT('Ctrl Pts',(-9.856006554992,0.3702218570889,3.88050485664));
#41404=CARTESIAN_POINT('Ctrl Pts',(-9.774756554992,-1.840140218572,2.361365094534));
#41405=CARTESIAN_POINT('Ctrl Pts',(-9.693506554992,-2.601888549192,-0.2102541825635));
#41406=CARTESIAN_POINT('Ctrl Pts',(-9.612256554992,-1.575505741456,-2.688161399818));
#41407=CARTESIAN_POINT('Ctrl Pts',(-9.531006554992,0.7815410610216,-3.967933638989));
#41408=CARTESIAN_POINT('Ctrl Pts',(-9.449756554992,3.418697194756,-3.479164797048));
#41409=CARTESIAN_POINT('Ctrl Pts',(-9.368506554992,5.160560368632,-1.439707868714));
#41410=CARTESIAN_POINT('Ctrl Pts',(-9.287256554992,5.230769969513,1.241452537133));
#41411=CARTESIAN_POINT('Ctrl Pts',(-9.206006554992,3.59802602242,3.369235077895));
#41412=CARTESIAN_POINT('Ctrl Pts',(-9.124756554992,0.9900817748502,3.99551804692));
#41413=CARTESIAN_POINT('Ctrl Pts',(-9.043506554992,-1.430778298539,2.840235927925));
#41414=CARTESIAN_POINT('Ctrl Pts',(-8.989339888326,-2.200388784654,1.227921101574));
#41415=CARTESIAN_POINT('Ctrl Pts',(-8.962256554992,-2.28859053225,0.388737529453));
#41416=CARTESIAN_POINT('Ctrl Pts',(-11.46868355268,5.269775872549,0.4056787913812));
#41417=CARTESIAN_POINT('Ctrl Pts',(-11.44160021935,5.177730274553,1.281434157126));
#41418=CARTESIAN_POINT('Ctrl Pts',(-11.38743355268,4.37458000429,2.964013997052));
#41419=CARTESIAN_POINT('Ctrl Pts',(-11.30618355268,1.848218348245,4.169643549716));
#41420=CARTESIAN_POINT('Ctrl Pts',(-11.22493355268,-0.8733806489824,3.51606703938));
#41421=CARTESIAN_POINT('Ctrl Pts',(-11.14368355268,-2.577279914956,1.295555295446));
#41422=CARTESIAN_POINT('Ctrl Pts',(-11.06243355268,-2.504010565149,-1.502450635378));
#41423=CARTESIAN_POINT('Ctrl Pts',(-10.98118355268,-0.686236633921,-3.630787518428));
#41424=CARTESIAN_POINT('Ctrl Pts',(-10.89993355268,2.06584730951,-4.140857007583));
#41425=CARTESIAN_POINT('Ctrl Pts',(-10.81868355268,4.5256146991,-2.805312029559));
#41426=CARTESIAN_POINT('Ctrl Pts',(-10.73743355268,5.596727481863,-0.2194171033222));
#41427=CARTESIAN_POINT('Ctrl Pts',(-10.65618355268,4.801782001457,2.464273873707));
#41428=CARTESIAN_POINT('Ctrl Pts',(-10.57493355268,2.495091889415,4.049618060818));
#41429=CARTESIAN_POINT('Ctrl Pts',(-10.49368355268,-0.2952324426901,3.830014774536));
#41430=CARTESIAN_POINT('Ctrl Pts',(-10.41243355268,-2.325520901626,1.903342966431));
#41431=CARTESIAN_POINT('Ctrl Pts',(-10.33118355268,-2.690857522625,-0.8716641748885));
#41432=CARTESIAN_POINT('Ctrl Pts',(-10.24993355268,-1.2284088228,-3.258163553058));
#41433=CARTESIAN_POINT('Ctrl Pts',(-10.16868355268,1.41,-4.192473119132));
#41434=CARTESIAN_POINT('Ctrl Pts',(-10.08743355268,4.0484088228,-3.258163553058));
#41435=CARTESIAN_POINT('Ctrl Pts',(-10.00618355268,5.510857522625,-0.8716641748885));
#41436=CARTESIAN_POINT('Ctrl Pts',(-9.924933552684,5.145520901626,1.903342966431));
#41437=CARTESIAN_POINT('Ctrl Pts',(-9.843683552684,3.11523244269,3.830014774536));
#41438=CARTESIAN_POINT('Ctrl Pts',(-9.762433552684,0.3249081105847,4.049618060818));
#41439=CARTESIAN_POINT('Ctrl Pts',(-9.681183552684,-1.981782001457,2.464273873707));
#41440=CARTESIAN_POINT('Ctrl Pts',(-9.599933552684,-2.776727481863,-0.2194171033222));
#41441=CARTESIAN_POINT('Ctrl Pts',(-9.518683552684,-1.7056146991,-2.805312029559));
#41442=CARTESIAN_POINT('Ctrl Pts',(-9.437433552684,0.7541526904896,-4.140857007583));
#41443=CARTESIAN_POINT('Ctrl Pts',(-9.356183552684,3.506236633921,-3.630787518428));
#41444=CARTESIAN_POINT('Ctrl Pts',(-9.274933552684,5.324010565149,-1.502450635378));
#41445=CARTESIAN_POINT('Ctrl Pts',(-9.193683552684,5.397279914956,1.295555295446));
#41446=CARTESIAN_POINT('Ctrl Pts',(-9.112433552684,3.693380648982,3.51606703938));
#41447=CARTESIAN_POINT('Ctrl Pts',(-9.031183552684,0.9717816517551,4.169643549716));
#41448=CARTESIAN_POINT('Ctrl Pts',(-8.949933552684,-1.55458000429,2.964013997052));
#41449=CARTESIAN_POINT('Ctrl Pts',(-8.895766886017,-2.357730274553,1.281434157126));
#41450=CARTESIAN_POINT('Ctrl Pts',(-8.868683552684,-2.449775872549,0.4056787913812));
#41451=CARTESIAN_POINT('Ctrl Pts',(-11.37511055037,5.430961212849,0.4226200533094));
#41452=CARTESIAN_POINT('Ctrl Pts',(-11.34802721704,5.335071764451,1.334947212679));
#41453=CARTESIAN_POINT('Ctrl Pts',(-11.29386055037,4.49838171004,3.087792066179));
#41454=CARTESIAN_POINT('Ctrl Pts',(-11.21261055037,1.86651847134,4.343769052512));
#41455=CARTESIAN_POINT('Ctrl Pts',(-11.13136055037,-0.9687352755443,3.662899000864));
#41456=CARTESIAN_POINT('Ctrl Pts',(-11.05011055037,-2.743789860399,1.349658053758));
#41457=CARTESIAN_POINT('Ctrl Pts',(-10.96886055037,-2.667460761666,-1.565193402042));
#41458=CARTESIAN_POINT('Ctrl Pts',(-10.88761055037,-0.7737760730864,-3.782410239809));
#41459=CARTESIAN_POINT('Ctrl Pts',(-10.80636055037,2.093235680042,-4.313780376177));
#41460=CARTESIAN_POINT('Ctrl Pts',(-10.72511055037,4.655723656744,-2.922462659301));
#41461=CARTESIAN_POINT('Ctrl Pts',(-10.64386055037,5.771566414534,-0.2285800240809));
#41462=CARTESIAN_POINT('Ctrl Pts',(-10.56261055037,4.943423784343,2.56718265288));
#41463=CARTESIAN_POINT('Ctrl Pts',(-10.48136055037,2.540405635919,4.218731264996));
#41464=CARTESIAN_POINT('Ctrl Pts',(-10.40011055037,-0.3664434354111,3.989957282902));
#41465=CARTESIAN_POINT('Ctrl Pts',(-10.31886055037,-2.481517318933,1.982827111076));
#41466=CARTESIAN_POINT('Ctrl Pts',(-10.23761055037,-2.862110501329,-0.9080651192168));
#41467=CARTESIAN_POINT('Ctrl Pts',(-10.15636055037,-1.338589527067,-3.394225391463));
#41468=CARTESIAN_POINT('Ctrl Pts',(-10.07511055037,1.41,-4.367551991253));
#41469=CARTESIAN_POINT('Ctrl Pts',(-9.993860550375,4.158589527067,-3.394225391463));
#41470=CARTESIAN_POINT('Ctrl Pts',(-9.912610550375,5.682110501329,-0.9080651192168));
#41471=CARTESIAN_POINT('Ctrl Pts',(-9.831360550375,5.301517318933,1.982827111076));
#41472=CARTESIAN_POINT('Ctrl Pts',(-9.750110550375,3.186443435411,3.989957282902));
#41473=CARTESIAN_POINT('Ctrl Pts',(-9.668860550375,0.2795943640806,4.218731264996));
#41474=CARTESIAN_POINT('Ctrl Pts',(-9.587610550375,-2.123423784343,2.56718265288));
#41475=CARTESIAN_POINT('Ctrl Pts',(-9.506360550375,-2.951566414534,-0.2285800240809));
#41476=CARTESIAN_POINT('Ctrl Pts',(-9.425110550375,-1.835723656744,-2.922462659301));
#41477=CARTESIAN_POINT('Ctrl Pts',(-9.343860550375,0.7267643199575,-4.313780376177));
#41478=CARTESIAN_POINT('Ctrl Pts',(-9.262610550375,3.593776073086,-3.782410239809));
#41479=CARTESIAN_POINT('Ctrl Pts',(-9.181360550375,5.487460761666,-1.565193402042));
#41480=CARTESIAN_POINT('Ctrl Pts',(-9.100110550375,5.563789860399,1.349658053758));
#41481=CARTESIAN_POINT('Ctrl Pts',(-9.018860550375,3.788735275544,3.662899000864));
#41482=CARTESIAN_POINT('Ctrl Pts',(-8.937610550375,0.9534815286599,4.343769052512));
#41483=CARTESIAN_POINT('Ctrl Pts',(-8.856360550375,-1.67838171004,3.087792066179));
#41484=CARTESIAN_POINT('Ctrl Pts',(-8.802193883708,-2.515071764451,1.334947212679));
#41485=CARTESIAN_POINT('Ctrl Pts',(-8.775110550375,-2.610961212849,0.4226200533094));
#41486=CARTESIAN_POINT('',(-8.85049707793188,-2.05335595069089,1.99956949126325));
#41487=CARTESIAN_POINT('Ctrl Pts',(-9.60040561164376,-2.05290755290942,
1.99927856802735));
#41488=CARTESIAN_POINT('Ctrl Pts',(-9.592648539488,-2.1776137658591,1.78299963277453));
#41489=CARTESIAN_POINT('Ctrl Pts',(-9.58470884554327,-2.28217153326222,
1.55504283182618));
#41490=CARTESIAN_POINT('Ctrl Pts',(-9.57348439445244,-2.40287751946333,
1.21030822786898));
#41491=CARTESIAN_POINT('Ctrl Pts',(-9.56998824900667,-2.43637685170845,
1.09948652005087));
#41492=CARTESIAN_POINT('Ctrl Pts',(-9.56104116063325,-2.51151184159235,
0.804747256195322));
#41493=CARTESIAN_POINT('Ctrl Pts',(-9.55572697913885,-2.54503434182388,
0.6189391301607));
#41494=CARTESIAN_POINT('Ctrl Pts',(-9.54639135395835,-2.58076150842344,
0.289758296971684));
#41495=CARTESIAN_POINT('Ctrl Pts',(-9.5423673684783,-2.58858131215265,0.147003740181955));
#41496=CARTESIAN_POINT('Ctrl Pts',(-9.53507432994476,-2.58884776661925,
-0.105680704039776));
#41497=CARTESIAN_POINT('Ctrl Pts',(-9.53184207956503,-2.58441720541216,
-0.215490452908572));
#41498=CARTESIAN_POINT('Ctrl Pts',(-9.52280012432087,-2.55989678693276,
-0.513982059176623));
#41499=CARTESIAN_POINT('Ctrl Pts',(-9.51686679260937,-2.53091011969018,
-0.701672132362012));
#41500=CARTESIAN_POINT('Ctrl Pts',(-9.50588507958739,-2.45341801109884,
-1.04246274749219));
#41501=CARTESIAN_POINT('Ctrl Pts',(-9.50084214484328,-2.40862312286159,
-1.19645621581327));
#41502=CARTESIAN_POINT('Ctrl Pts',(-9.49233887140167,-2.3158703794896,-1.45621742318579));
#41503=CARTESIAN_POINT('Ctrl Pts',(-9.48882592440186,-2.27219666730552,
-1.56360618312295));
#41504=CARTESIAN_POINT('Ctrl Pts',(-9.48029499114608,-2.15159532242807,
-1.82637699560855));
#41505=CARTESIAN_POINT('Ctrl Pts',(-9.47538062504686,-2.069064105986,-1.97900341303359));
#41506=CARTESIAN_POINT('Ctrl Pts',(-9.46615567140573,-1.89546155828856,
-2.25561353392233));
#41507=CARTESIAN_POINT('Ctrl Pts',(-9.46183917000714,-1.80644120827349,
-2.38087096327682));
#41508=CARTESIAN_POINT('Ctrl Pts',(-9.45415180995853,-1.63964141944734,
-2.58902989023001));
#41509=CARTESIAN_POINT('Ctrl Pts',(-9.45082545411876,-1.56505867046786,
-2.67437719622726));
#41510=CARTESIAN_POINT('Ctrl Pts',(-9.44193507944392,-1.3616794778249,-2.88785816818869));
#41511=CARTESIAN_POINT('Ctrl Pts',(-9.4362720629285,-1.22761667937358,-3.01060219187097));
#41512=CARTESIAN_POINT('Ctrl Pts',(-9.42537925227153,-0.956317980604446,
-3.22729703651813));
#41513=CARTESIAN_POINT('Ctrl Pts',(-9.42015377674645,-0.820292770316238,
-3.32283525765303));
#41514=CARTESIAN_POINT('Ctrl Pts',(-9.41140145470753,-0.578262866398371,
-3.47131975099939));
#41515=CARTESIAN_POINT('Ctrl Pts',(-9.40781778162555,-0.474838742752067,
-3.52864839224943));
#41516=CARTESIAN_POINT('Ctrl Pts',(-9.39902837168875,-0.208041882939476,
-3.66125372848236));
#41517=CARTESIAN_POINT('Ctrl Pts',(-9.39393789067322,-0.0417324379309015,
-3.73027639780195));
#41518=CARTESIAN_POINT('Ctrl Pts',(-9.38462373683353,0.270802409734637,
-3.83600739585551));
#41519=CARTESIAN_POINT('Ctrl Pts',(-9.3803935544249,0.415853012911651,-3.87615241357383));
#41520=CARTESIAN_POINT('Ctrl Pts',(-9.37282172899103,0.672504693060417,
-3.93180158109821));
#41521=CARTESIAN_POINT('Ctrl Pts',(-9.36952225777246,0.783217461030843,
-3.95094716539007));
#41522=CARTESIAN_POINT('Ctrl Pts',(-9.36057767995255,1.07730095533725,-3.98898846612685));
#41523=CARTESIAN_POINT('Ctrl Pts',(-9.35482582565714,1.26143084800293,-3.99993400067362));
#41524=CARTESIAN_POINT('Ctrl Pts',(-9.34390302474602,1.60941374719111,-3.996804169109));
#41525=CARTESIAN_POINT('Ctrl Pts',(-9.33873705567264,1.77333514304933,-3.985318970206));
#41526=CARTESIAN_POINT('Ctrl Pts',(-9.33006499181736,2.05225354082227,-3.94849144148094));
#41527=CARTESIAN_POINT('Ctrl Pts',(-9.32650344265707,2.16798340920093,-3.92801068498396));
#41528=CARTESIAN_POINT('Ctrl Pts',(-9.31770187978694,2.45914821402567,-3.8629718548007));
#41529=CARTESIAN_POINT('Ctrl Pts',(-9.31258089141444,2.63287631226559,-3.81149482924049));
#41530=CARTESIAN_POINT('Ctrl Pts',(-9.30325830244933,2.94244192303581,-3.69650349598188));
#41531=CARTESIAN_POINT('Ctrl Pts',(-9.29905027707537,3.07961834901688,-3.63662675072915));
#41532=CARTESIAN_POINT('Ctrl Pts',(-9.29150488237336,3.31315682168349,-3.51865862815614));
#41533=CARTESIAN_POINT('Ctrl Pts',(-9.28820897884544,3.41107967410374,-3.4638869342709));
#41534=CARTESIAN_POINT('Ctrl Pts',(-9.27854372821509,3.6837784145769,-3.29574888792376));
#41535=CARTESIAN_POINT('Ctrl Pts',(-9.27201150657151,3.85227437190568,-3.17269744237438));
#41536=CARTESIAN_POINT('Ctrl Pts',(-9.26076563378601,4.12433811974851,-2.93979520510097));
#41537=CARTESIAN_POINT('Ctrl Pts',(-9.25605159748808,4.23295854266567,-2.83576544018229));
#41538=CARTESIAN_POINT('Ctrl Pts',(-9.2479582242247,4.4126197712042,-2.64320887657756));
#41539=CARTESIAN_POINT('Ctrl Pts',(-9.24453637118187,4.48636945008601,-2.55712563604215));
#41540=CARTESIAN_POINT('Ctrl Pts',(-9.23527915118763,4.68063272081885,-2.30955700187998));
#41541=CARTESIAN_POINT('Ctrl Pts',(-9.22961408698511,4.79281112244183,-2.14179114553789));
#41542=CARTESIAN_POINT('Ctrl Pts',(-9.21884251351113,4.98047464746399,-1.80954647457836));
#41543=CARTESIAN_POINT('Ctrl Pts',(-9.21373710578579,5.05855440007191,-1.64655360337947));
#41544=CARTESIAN_POINT('Ctrl Pts',(-9.20505023257498,5.16751183864385,-1.37267062905776));
#41545=CARTESIAN_POINT('Ctrl Pts',(-9.20158993180501,5.20513996551312,-1.26465070786087));
#41546=CARTESIAN_POINT('Ctrl Pts',(-9.19343918098472,5.28149413823754,-1.01106616003464));
#41547=CARTESIAN_POINT('Ctrl Pts',(-9.18870681802321,5.31678442944973,-0.864384964301256));
#41548=CARTESIAN_POINT('Ctrl Pts',(-9.17739515814574,5.38131982281984,-0.509975379617664));
#41549=CARTESIAN_POINT('Ctrl Pts',(-9.17081921067416,5.40279186905983,-0.300777659727165));
#41550=CARTESIAN_POINT('Ctrl Pts',(-9.16110302171323,5.41033007588258,0.0221346401150478));
#41551=CARTESIAN_POINT('Ctrl Pts',(-9.15779006413838,5.40810872064692,0.13533898255474));
#41552=CARTESIAN_POINT('Ctrl Pts',(-9.1501099337789,5.39152354672244,0.401818718343227));
#41553=CARTESIAN_POINT('Ctrl Pts',(-9.14578574227475,5.37308243798484,0.554813369105755));
#41554=CARTESIAN_POINT('Ctrl Pts',(-9.1365314088165,5.31523418561994,0.877269127846519));
#41555=CARTESIAN_POINT('Ctrl Pts',(-9.13159401369815,5.27342523279836,1.04628752255256));
#41556=CARTESIAN_POINT('Ctrl Pts',(-9.12291148671605,5.1843800684607,1.32601600955524));
#41557=CARTESIAN_POINT('Ctrl Pts',(-9.11926957743045,5.14287952611652,1.43844054224961));
#41558=CARTESIAN_POINT('Ctrl Pts',(-9.11039177534989,5.03139259821727,1.70335638586575));
#41559=CARTESIAN_POINT('Ctrl Pts',(-9.10510023615257,4.95660383324509,1.85391807599278));
#41560=CARTESIAN_POINT('Ctrl Pts',(-9.09423927196797,4.78354047908282,2.15381290277887));
#41561=CARTESIAN_POINT('Ctrl Pts',(-9.08867386848596,4.68404755562057,2.30249311099628));
#41562=CARTESIAN_POINT('Ctrl Pts',(-9.07990374444557,4.50603297095058,2.53329501675828));
#41563=CARTESIAN_POINT('Ctrl Pts',(-9.07660075824385,4.43335574420623,2.61961582623421));
#41564=CARTESIAN_POINT('Ctrl Pts',(-9.06896979110242,4.25409634850611,2.81507344530256));
#41565=CARTESIAN_POINT('Ctrl Pts',(-9.06468373933528,4.14461929465385,2.92151190694135));
#41566=CARTESIAN_POINT('Ctrl Pts',(-9.05539340321852,3.89608227609904,3.13700171113091));
#41567=CARTESIAN_POINT('Ctrl Pts',(-9.05038120579234,3.75508985350886,3.24380605163546));
#41568=CARTESIAN_POINT('Ctrl Pts',(-9.04159512009966,3.50686187688791,3.40699539292465));
#41569=CARTESIAN_POINT('Ctrl Pts',(-9.03792977313163,3.4031621408114,3.4685727911801));
#41570=CARTESIAN_POINT('Ctrl Pts',(-9.02896739234424,3.14725711947419,3.60535098970956));
#41571=CARTESIAN_POINT('Ctrl Pts',(-9.0236134674557,2.99245342224551,3.67586783017103));
#41572=CARTESIAN_POINT('Ctrl Pts',(-9.01278533577553,2.66972272653378,3.79894303584769));
#41573=CARTESIAN_POINT('Ctrl Pts',(-9.00731356779278,2.50148472998555,3.85080686984647));
#41574=CARTESIAN_POINT('Ctrl Pts',(-8.99860131029036,2.21963774923441,3.91764290759745));
#41575=CARTESIAN_POINT('Ctrl Pts',(-8.99527062217913,2.10782053336575,3.93910479370828));
#41576=CARTESIAN_POINT('Ctrl Pts',(-8.98752159965826,1.84129132913886,3.97852936330207));
#41577=CARTESIAN_POINT('Ctrl Pts',(-8.98314744245908,1.68598465452508,3.99229038034456));
#41578=CARTESIAN_POINT('Ctrl Pts',(-8.97394664224195,1.36059820382706,4.00209870554907));
#41579=CARTESIAN_POINT('Ctrl Pts',(-8.9691140595699,1.19047788812806,3.99641147226209));
#41580=CARTESIAN_POINT('Ctrl Pts',(-8.96059716426728,0.903927748838954,
3.96834102692915));
#41581=CARTESIAN_POINT('Ctrl Pts',(-8.95700957819773,0.787066552216668,
3.95158223146842));
#41582=CARTESIAN_POINT('Ctrl Pts',(-8.94831693167847,0.510559749166548,
3.89940737616986));
#41583=CARTESIAN_POINT('Ctrl Pts',(-8.94315879217041,0.351720107753647,
3.85925077816371));
#41584=CARTESIAN_POINT('Ctrl Pts',(-8.93223114940881,0.0201993913987,3.75364135889862));
#41585=CARTESIAN_POINT('Ctrl Pts',(-8.92646800622479,-0.151703930561329,
3.68559482016283));
#41586=CARTESIAN_POINT('Ctrl Pts',(-8.91759357809553,-0.41751404746469,
3.55838411955562));
#41587=CARTESIAN_POINT('Ctrl Pts',(-8.91436575366286,-0.514758393542523,
3.50675051154773));
#41588=CARTESIAN_POINT('Ctrl Pts',(-8.90704049634875,-0.734254785941745,
3.37829084050234));
#41589=CARTESIAN_POINT('Ctrl Pts',(-8.9029793843837,-0.854810071293984,
3.29866643381797));
#41590=CARTESIAN_POINT('Ctrl Pts',(-8.89365713134142,-1.12044496397458,
3.10185526197797));
#41591=CARTESIAN_POINT('Ctrl Pts',(-8.88838974677078,-1.2624183779927,2.98049157119333));
#41592=CARTESIAN_POINT('Ctrl Pts',(-8.8794044082883,-1.47951408331325,2.7667175653459));
#41593=CARTESIAN_POINT('Ctrl Pts',(-8.87581931075566,-1.56003831183313,
2.6799717451396));
#41594=CARTESIAN_POINT('Ctrl Pts',(-8.86475153953041,-1.79264008377585,
2.40606890783807));
#41595=CARTESIAN_POINT('Ctrl Pts',(-8.85708769733734,-1.93217852399906,
2.20811551137394));
#41596=CARTESIAN_POINT('Ctrl Pts',(-8.84959438835624,-2.05287980560813,
1.99932662776271));
#41597=CARTESIAN_POINT('',(-9.080940107676,-1.707691453624,1.8));
#41598=CARTESIAN_POINT('Ctrl Pts',(-9.155829557301,-0.6806876086837,2.877584625945));
#41599=CARTESIAN_POINT('Ctrl Pts',(-9.128746223968,-1.333590849641,2.403222654717));
#41600=CARTESIAN_POINT('Ctrl Pts',(-9.074579557301,-2.301009810423,0.9947418214436));
#41601=CARTESIAN_POINT('Ctrl Pts',(-8.993329557301,-2.10023207207,-1.562884793063));
#41602=CARTESIAN_POINT('Ctrl Pts',(-8.912079557301,-0.3343472621158,-3.423508148791));
#41603=CARTESIAN_POINT('Ctrl Pts',(-8.830829557301,2.208854940398,-3.758356902288));
#41604=CARTESIAN_POINT('Ctrl Pts',(-8.749579557301,4.396041844558,-2.418045984201));
#41605=CARTESIAN_POINT('Ctrl Pts',(-8.668329557301,5.252314847485,-3.831845932778E-7));
#41606=CARTESIAN_POINT('Ctrl Pts',(-8.587079557301,4.396040017561,2.418047516939));
#41607=CARTESIAN_POINT('Ctrl Pts',(-8.505829557301,2.208862248383,3.758351537704));
#41608=CARTESIAN_POINT('Ctrl Pts',(-8.424579557301,-0.3343746670588,3.423528074391));
#41609=CARTESIAN_POINT('Ctrl Pts',(-8.343329557301,-2.100129760283,1.562810455248));
#41610=CARTESIAN_POINT('Ctrl Pts',(-8.262079557301,-2.301391652629,-0.9944643957835));
#41611=CARTESIAN_POINT('Ctrl Pts',(-8.180829557301,-0.8484563122144,-3.108498436179));
#41612=CARTESIAN_POINT('Ctrl Pts',(-8.099579557301,1.611091249384,-3.837049615173));
#41613=CARTESIAN_POINT('Ctrl Pts',(-8.018329557301,3.981010816611,-2.855396788715));
#41614=CARTESIAN_POINT('Ctrl Pts',(-7.937079557301,5.205010096676,-0.6010705501845));
#41615=CARTESIAN_POINT('Ctrl Pts',(-7.855829557301,4.737542724007,1.921157687446));
#41616=CARTESIAN_POINT('Ctrl Pts',(-7.774579557301,2.786962682412,3.587110426432));
#41617=CARTESIAN_POINT('Ctrl Pts',(-7.693329557301,0.2226592513938,3.654259074947));
#41618=CARTESIAN_POINT('Ctrl Pts',(-7.612079557301,-1.812436817629,2.092674938032));
#41619=CARTESIAN_POINT('Ctrl Pts',(-7.530829557301,-2.411266769463,-0.4016313216255));
#41620=CARTESIAN_POINT('Ctrl Pts',(-7.449579557301,-1.306927256222,-2.716927256679));
#41621=CARTESIAN_POINT('Ctrl Pts',(-7.368329557301,1.008368675403,-3.821266770609));
#41622=CARTESIAN_POINT('Ctrl Pts',(-7.287079557301,3.502674949463,-3.222436812587));
#41623=CARTESIAN_POINT('Ctrl Pts',(-7.205829557301,5.064259032195,-1.187340767628));
#41624=CARTESIAN_POINT('Ctrl Pts',(-7.124579557301,4.997110586008,1.376962753456));
#41625=CARTESIAN_POINT('Ctrl Pts',(-7.043329557301,3.331157091895,3.327542458853));
#41626=CARTESIAN_POINT('Ctrl Pts',(-6.962079557301,0.8089316724422,3.795011086251));
#41627=CARTESIAN_POINT('Ctrl Pts',(-6.880829557301,-1.445405083671,2.571007123468));
#41628=CARTESIAN_POINT('Ctrl Pts',(-6.799579557301,-2.427018657974,0.2011050323817));
#41629=CARTESIAN_POINT('Ctrl Pts',(-6.718329557301,-1.698613970016,-2.258507751061));
#41630=CARTESIAN_POINT('Ctrl Pts',(-6.637079557301,0.4159667823653,-3.711199680242));
#41631=CARTESIAN_POINT('Ctrl Pts',(-6.582912890634,2.119456445115,-3.577630700739));
#41632=CARTESIAN_POINT('Ctrl Pts',(-6.555829557301,2.856717583266,-3.24938089347));
#41633=CARTESIAN_POINT('Ctrl Pts',(-9.062256554992,-0.7759518420355,3.008704594398));
#41634=CARTESIAN_POINT('Ctrl Pts',(-9.035173221659,-1.458605260133,2.512727854262));
#41635=CARTESIAN_POINT('Ctrl Pts',(-8.981006554992,-2.470105615594,1.040068209092));
#41636=CARTESIAN_POINT('Ctrl Pts',(-8.899756554992,-2.260179242486,-1.634099172968));
#41637=CARTESIAN_POINT('Ctrl Pts',(-8.818506554992,-0.4138301575682,-3.579503658505));
#41638=CARTESIAN_POINT('Ctrl Pts',(-8.737256554992,2.245255550006,-3.929610124181));
#41639=CARTESIAN_POINT('Ctrl Pts',(-8.656006554992,4.532103772651,-2.528226623306));
#41640=CARTESIAN_POINT('Ctrl Pts',(-8.574756554992,5.427393695574,-4.006447741335E-7));
#41641=CARTESIAN_POINT('Ctrl Pts',(-8.493506554992,4.532101862406,2.528228225885));
#41642=CARTESIAN_POINT('Ctrl Pts',(-8.412256554992,2.245263190987,3.929604515154));
#41643=CARTESIAN_POINT('Ctrl Pts',(-8.331006554992,-0.4138588112444,3.579524492034));
#41644=CARTESIAN_POINT('Ctrl Pts',(-8.249756554992,-2.260072268762,1.634021447877));
#41645=CARTESIAN_POINT('Ctrl Pts',(-8.168506554992,-2.470504856815,-1.039778142259));
#41646=CARTESIAN_POINT('Ctrl Pts',(-8.087256554992,-0.9513650912439,-3.250140219087));
#41647=CARTESIAN_POINT('Ctrl Pts',(-8.006006554992,1.620254169577,-4.011888547782));
#41648=CARTESIAN_POINT('Ctrl Pts',(-7.924756554992,4.098161448473,-2.985505746582));
#41649=CARTESIAN_POINT('Ctrl Pts',(-7.843506554992,5.377933457354,-0.6284589198844));
#41650=CARTESIAN_POINT('Ctrl Pts',(-7.762256554992,4.88916547493,2.008697123506));
#41651=CARTESIAN_POINT('Ctrl Pts',(-7.681006554992,2.849705338822,3.750560634537));
#41652=CARTESIAN_POINT('Ctrl Pts',(-7.599756554992,0.1685569045517,3.820768977142));
#41653=CARTESIAN_POINT('Ctrl Pts',(-7.518506554992,-1.959270314743,2.188029725996));
#41654=CARTESIAN_POINT('Ctrl Pts',(-7.437256554992,-2.585386541213,-0.4199320470833));
#41655=CARTESIAN_POINT('Ctrl Pts',(-7.356006554992,-1.430726713904,-2.840726714381));
#41656=CARTESIAN_POINT('Ctrl Pts',(-7.274756554992,0.9900679498094,-3.995386542412));
#41657=CARTESIAN_POINT('Ctrl Pts',(-7.193506554992,3.598029737948,-3.369270309471));
#41658=CARTESIAN_POINT('Ctrl Pts',(-7.112256554992,5.230768932443,-1.241443115336));
#41659=CARTESIAN_POINT('Ctrl Pts',(-7.031006554992,5.160560801384,1.439705413104));
#41660=CARTESIAN_POINT('Ctrl Pts',(-6.949756554992,3.418696500819,3.479165197693));
#41661=CARTESIAN_POINT('Ctrl Pts',(-6.868506554992,0.7815434040185,3.96793449202));
#41662=CARTESIAN_POINT('Ctrl Pts',(-6.787256554992,-1.575514419506,2.688157587048));
#41663=CARTESIAN_POINT('Ctrl Pts',(-6.706006554992,-2.601856179989,0.2102685806102));
#41664=CARTESIAN_POINT('Ctrl Pts',(-6.624756554992,-1.840261017337,-2.361418873952));
#41665=CARTESIAN_POINT('Ctrl Pts',(-6.543506554992,0.3706726829451,-3.880304137017));
#41666=CARTESIAN_POINT('Ctrl Pts',(-6.489339888326,2.151783524521,-3.740648955836));
#41667=CARTESIAN_POINT('Ctrl Pts',(-6.462256554992,2.922638690214,-3.397442123851));
#41668=CARTESIAN_POINT('Ctrl Pts',(-8.968683552684,-0.8712160753873,3.139824562851));
#41669=CARTESIAN_POINT('Ctrl Pts',(-8.94160021935,-1.583619670625,2.622233053807));
#41670=CARTESIAN_POINT('Ctrl Pts',(-8.887433552684,-2.639201420765,1.08539459674));
#41671=CARTESIAN_POINT('Ctrl Pts',(-8.806183552684,-2.420126412902,-1.705313552873));
#41672=CARTESIAN_POINT('Ctrl Pts',(-8.724933552684,-0.4933130530206,-3.735499168218));
#41673=CARTESIAN_POINT('Ctrl Pts',(-8.643683552684,2.281656159615,-4.100863346074));
#41674=CARTESIAN_POINT('Ctrl Pts',(-8.562433552684,4.668165700744,-2.638407262411));
#41675=CARTESIAN_POINT('Ctrl Pts',(-8.481183552684,5.602472543663,-4.181049654858E-7));
#41676=CARTESIAN_POINT('Ctrl Pts',(-8.399933552684,4.66816370725,2.638408934831));
#41677=CARTESIAN_POINT('Ctrl Pts',(-8.318683552684,2.28166413359,4.100857492604));
#41678=CARTESIAN_POINT('Ctrl Pts',(-8.237433552684,-0.4933429554299,3.735520909677));
#41679=CARTESIAN_POINT('Ctrl Pts',(-8.156183552684,-2.420014777241,1.705232440507));
#41680=CARTESIAN_POINT('Ctrl Pts',(-8.074933552684,-2.639618061001,-1.085091888735));
#41681=CARTESIAN_POINT('Ctrl Pts',(-7.993683552684,-1.054273870273,-3.391782001995));
#41682=CARTESIAN_POINT('Ctrl Pts',(-7.912433552684,1.62941708977,-4.186727480392));
#41683=CARTESIAN_POINT('Ctrl Pts',(-7.831183552684,4.215312080335,-3.11561470445));
#41684=CARTESIAN_POINT('Ctrl Pts',(-7.749933552684,5.550856818033,-0.6558472895843));
#41685=CARTESIAN_POINT('Ctrl Pts',(-7.668683552684,5.040788225852,2.096236559566));
#41686=CARTESIAN_POINT('Ctrl Pts',(-7.587433552684,2.912447995233,3.914010842643));
#41687=CARTESIAN_POINT('Ctrl Pts',(-7.506183552684,0.1144545577098,3.987278879338));
#41688=CARTESIAN_POINT('Ctrl Pts',(-7.424933552684,-2.106103811857,2.283384513961));
#41689=CARTESIAN_POINT('Ctrl Pts',(-7.343683552684,-2.759506312963,-0.4382327725412));
#41690=CARTESIAN_POINT('Ctrl Pts',(-7.262433552684,-1.554526171585,-2.964526172083));
#41691=CARTESIAN_POINT('Ctrl Pts',(-7.181183552684,0.9717672242161,-4.169506314214));
#41692=CARTESIAN_POINT('Ctrl Pts',(-7.099933552684,3.693384526433,-3.516103806355));
#41693=CARTESIAN_POINT('Ctrl Pts',(-7.018683552684,5.39727883269,-1.295545463045));
#41694=CARTESIAN_POINT('Ctrl Pts',(-6.937433552684,5.324011016761,1.502448072752));
#41695=CARTESIAN_POINT('Ctrl Pts',(-6.856183552684,3.506235909742,3.630787936533));
#41696=CARTESIAN_POINT('Ctrl Pts',(-6.774933552684,0.7541551355947,4.140857897789));
#41697=CARTESIAN_POINT('Ctrl Pts',(-6.693683552684,-1.705623755341,2.805308050628));
#41698=CARTESIAN_POINT('Ctrl Pts',(-6.612433552684,-2.776693702003,0.2194321288388));
#41699=CARTESIAN_POINT('Ctrl Pts',(-6.531183552684,-1.981908064657,-2.464329996843));
#41700=CARTESIAN_POINT('Ctrl Pts',(-6.449933552684,0.325378583525,-4.049408593792));
#41701=CARTESIAN_POINT('Ctrl Pts',(-6.395766886017,2.184110603928,-3.903667210934));
#41702=CARTESIAN_POINT('Ctrl Pts',(-6.368683552684,2.988559797162,-3.545503354232));
#41703=CARTESIAN_POINT('Ctrl Pts',(-8.875110550375,-0.9664803087391,3.270944531304));
#41704=CARTESIAN_POINT('Ctrl Pts',(-8.848027217042,-1.708634081117,2.731738253352));
#41705=CARTESIAN_POINT('Ctrl Pts',(-8.793860550375,-2.808297225935,1.130720984389));
#41706=CARTESIAN_POINT('Ctrl Pts',(-8.712610550375,-2.580073583318,-1.776527932779));
#41707=CARTESIAN_POINT('Ctrl Pts',(-8.631360550375,-0.5727959484731,-3.891494677932));
#41708=CARTESIAN_POINT('Ctrl Pts',(-8.550110550375,2.318056769223,-4.272116567967));
#41709=CARTESIAN_POINT('Ctrl Pts',(-8.468860550375,4.804227628837,-2.748587901516));
#41710=CARTESIAN_POINT('Ctrl Pts',(-8.387610550375,5.777551391752,-4.35565146617E-7));
#41711=CARTESIAN_POINT('Ctrl Pts',(-8.306360550375,4.804225552094,2.748589643777));
#41712=CARTESIAN_POINT('Ctrl Pts',(-8.225110550375,2.318065076194,4.272110470055));
#41713=CARTESIAN_POINT('Ctrl Pts',(-8.143860550375,-0.5728270996155,3.89151732732));
#41714=CARTESIAN_POINT('Ctrl Pts',(-8.062610550375,-2.57995728572,1.776443433137));
#41715=CARTESIAN_POINT('Ctrl Pts',(-7.981360550375,-2.808731265186,-1.130405635211));
#41716=CARTESIAN_POINT('Ctrl Pts',(-7.900110550375,-1.157182649303,-3.533423784903));
#41717=CARTESIAN_POINT('Ctrl Pts',(-7.818860550375,1.638580009963,-4.361566413001));
#41718=CARTESIAN_POINT('Ctrl Pts',(-7.737610550375,4.332462712197,-3.245723662317));
#41719=CARTESIAN_POINT('Ctrl Pts',(-7.656360550375,5.723780178711,-0.6832356592843));
#41720=CARTESIAN_POINT('Ctrl Pts',(-7.575110550375,5.192410976774,2.183775995627));
#41721=CARTESIAN_POINT('Ctrl Pts',(-7.493860550375,2.975190651644,4.077461050748));
#41722=CARTESIAN_POINT('Ctrl Pts',(-7.412610550375,0.06035221086774,4.153788781534));
#41723=CARTESIAN_POINT('Ctrl Pts',(-7.331360550375,-2.252937308971,2.378739301925));
#41724=CARTESIAN_POINT('Ctrl Pts',(-7.250110550375,-2.933626084714,-0.4565334979991));
#41725=CARTESIAN_POINT('Ctrl Pts',(-7.168860550375,-1.678325629267,-3.088325629786));
#41726=CARTESIAN_POINT('Ctrl Pts',(-7.087610550375,0.9534664986228,-4.343626086017));
#41727=CARTESIAN_POINT('Ctrl Pts',(-7.006360550375,3.788739314919,-3.662937303239));
#41728=CARTESIAN_POINT('Ctrl Pts',(-6.925110550375,5.563788732938,-1.349647810754));
#41729=CARTESIAN_POINT('Ctrl Pts',(-6.843860550375,5.487461232137,1.5651907324));
#41730=CARTESIAN_POINT('Ctrl Pts',(-6.762610550375,3.593775318665,3.782410675374));
#41731=CARTESIAN_POINT('Ctrl Pts',(-6.681360550375,0.726766867171,4.313781303558));
#41732=CARTESIAN_POINT('Ctrl Pts',(-6.600110550375,-1.835733091177,2.922458514209));
#41733=CARTESIAN_POINT('Ctrl Pts',(-6.518860550375,-2.951531224017,0.2285956770674));
#41734=CARTESIAN_POINT('Ctrl Pts',(-6.437610550375,-2.123555111978,-2.567241119733));
#41735=CARTESIAN_POINT('Ctrl Pts',(-6.356360550375,0.2800844841049,-4.218513050568));
#41736=CARTESIAN_POINT('Ctrl Pts',(-6.302193883708,2.216437683334,-4.066685466031));
#41737=CARTESIAN_POINT('Ctrl Pts',(-6.275110550375,3.05448090411,-3.693564584614));
#41738=CARTESIAN_POINT('',(-7.09950292206828,1.41000000072087,-3.99913898127794));
#41739=CARTESIAN_POINT('Ctrl Pts',(-8.84961610999201,-2.05291292567607,
1.99934460346442));
#41740=CARTESIAN_POINT('Ctrl Pts',(-8.84643469718357,-2.10585184919526,
1.90810351889361));
#41741=CARTESIAN_POINT('Ctrl Pts',(-8.84328515155475,-2.15519371918908,
1.8147745582008));
#41742=CARTESIAN_POINT('Ctrl Pts',(-8.83591275217547,-2.2633832825094,1.58864351247807));
#41743=CARTESIAN_POINT('Ctrl Pts',(-8.8317778322986,-2.31848548620886,1.45490383377774));
#41744=CARTESIAN_POINT('Ctrl Pts',(-8.82247441886724,-2.4255455182645,1.14801103160697));
#41745=CARTESIAN_POINT('Ctrl Pts',(-8.81729234582501,-2.4729511085549,0.974529705226004));
#41746=CARTESIAN_POINT('Ctrl Pts',(-8.80112450537185,-2.57998489333633,
0.442598530957726));
#41747=CARTESIAN_POINT('Ctrl Pts',(-8.78983025833947,-2.60302956037622,
0.077532645670375));
#41748=CARTESIAN_POINT('Ctrl Pts',(-8.77367021457257,-2.56624884193027,
-0.44869507039522));
#41749=CARTESIAN_POINT('Ctrl Pts',(-8.7686466263556,-2.54466145780971,-0.612896922482584));
#41750=CARTESIAN_POINT('Ctrl Pts',(-8.75775263229734,-2.47454393779728,
-0.972005640751989));
#41751=CARTESIAN_POINT('Ctrl Pts',(-8.7520275571852,-2.4214708033906,-1.16480931942071));
#41752=CARTESIAN_POINT('Ctrl Pts',(-8.7421872235292,-2.30471804700921,-1.48946009464062));
#41753=CARTESIAN_POINT('Ctrl Pts',(-8.73805722520744,-2.24844822486328,
-1.62241166452016));
#41754=CARTESIAN_POINT('Ctrl Pts',(-8.72254433148797,-2.01664563597645,
-2.09553806880504));
#41755=CARTESIAN_POINT('Ctrl Pts',(-8.71065560548505,-1.79886466058706,
-2.4143220834137));
#41756=CARTESIAN_POINT('Ctrl Pts',(-8.69365907904848,-1.42570887431899,
-2.82363549841843));
#41757=CARTESIAN_POINT('Ctrl Pts',(-8.68841624212281,-1.30178161453281,
-2.94337585970706));
#41758=CARTESIAN_POINT('Ctrl Pts',(-8.67735221388011,-1.01938028138805,
-3.18302451148001));
#41759=CARTESIAN_POINT('Ctrl Pts',(-8.67165111376055,-0.859279685456863,
-3.2994802782033));
#41760=CARTESIAN_POINT('Ctrl Pts',(-8.66190045517826,-0.568761868358127,
-3.47877777326836));
#41761=CARTESIAN_POINT('Ctrl Pts',(-8.65782410662076,-0.443317057013741,
-3.54706086873473));
#41762=CARTESIAN_POINT('Ctrl Pts',(-8.64132703477721,0.0640327092394041,
-3.7882575867043));
#41763=CARTESIAN_POINT('Ctrl Pts',(-8.62824850589926,0.470640809013835,
-3.90791123447323));
#41764=CARTESIAN_POINT('Ctrl Pts',(-8.61044140350239,1.04713748034553,-3.98502302993153));
#41765=CARTESIAN_POINT('Ctrl Pts',(-8.60548443803191,1.2102545500858,-3.9969078795374));
#41766=CARTESIAN_POINT('Ctrl Pts',(-8.59515651420951,1.55741612539018,-4.00083483168217));
#41767=CARTESIAN_POINT('Ctrl Pts',(-8.5898895028002,1.74049468293642,-3.99015660630172));
#41768=CARTESIAN_POINT('Ctrl Pts',(-8.58056869571077,2.06425917812041,-3.94831799296271));
#41769=CARTESIAN_POINT('Ctrl Pts',(-8.57650147557731,2.20438669944499,-3.92240383461698));
#41770=CARTESIAN_POINT('Ctrl Pts',(-8.56002073851416,2.74983692291422,-3.79040103014612));
#41771=CARTESIAN_POINT('Ctrl Pts',(-8.54694915183239,3.14082122272124,-3.62743044270923));
#41772=CARTESIAN_POINT('Ctrl Pts',(-8.52915529031549,3.63689263990031,-3.32460692390838));
#41773=CARTESIAN_POINT('Ctrl Pts',(-8.52420398753128,3.77095831295386,-3.23125759146068));
#41774=CARTESIAN_POINT('Ctrl Pts',(-8.51389411669355,4.04270443314504,-3.01614686497048));
#41775=CARTESIAN_POINT('Ctrl Pts',(-8.50863879372461,4.17794605317645,-2.89290537102979));
#41776=CARTESIAN_POINT('Ctrl Pts',(-8.49932745081146,4.40301277325326,-2.65690966990474));
#41777=CARTESIAN_POINT('Ctrl Pts',(-8.49525813554999,4.49565973671551,-2.54853493962672));
#41778=CARTESIAN_POINT('Ctrl Pts',(-8.47877701820019,4.83650831458462,-2.10268780431962));
#41779=CARTESIAN_POINT('Ctrl Pts',(-8.46570772144381,5.03779224688927,-1.73004875918671));
#41780=CARTESIAN_POINT('Ctrl Pts',(-8.44791389274035,5.23278312210009,-1.18254251514403));
#41781=CARTESIAN_POINT('Ctrl Pts',(-8.44296082188042,5.27825054675726,-1.02557489464891));
#41782=CARTESIAN_POINT('Ctrl Pts',(-8.43264709904295,5.35410471824543,-0.687268766736908));
#41783=CARTESIAN_POINT('Ctrl Pts',(-8.42738976494414,5.38166207631401,-0.506314523396236));
#41784=CARTESIAN_POINT('Ctrl Pts',(-8.41807628569901,5.40805734092156,-0.181200078776905));
#41785=CARTESIAN_POINT('Ctrl Pts',(-8.41400681584487,5.4118535287336,-0.038669047923537));
#41786=CARTESIAN_POINT('Ctrl Pts',(-8.39752963410245,5.39615862362053,0.52218033981318));
#41787=CARTESIAN_POINT('Ctrl Pts',(-8.38446506662701,5.31812128108418,0.938302420612284));
#41788=CARTESIAN_POINT('Ctrl Pts',(-8.36667436630585,5.12518920830089,1.48642197477676));
#41789=CARTESIAN_POINT('Ctrl Pts',(-8.36172010839471,5.06173943130446,1.63706105192243));
#41790=CARTESIAN_POINT('Ctrl Pts',(-8.35139853909729,4.90769379927833,1.9479521346632));
#41791=CARTESIAN_POINT('Ctrl Pts',(-8.34613505129627,4.81511847895967,2.10611122227327));
#41792=CARTESIAN_POINT('Ctrl Pts',(-8.33681436091682,4.63086025725661,2.37557631433623));
#41793=CARTESIAN_POINT('Ctrl Pts',(-8.33274379702978,4.54407997861189,2.48874957051106));
#41794=CARTESIAN_POINT('Ctrl Pts',(-8.31628231271703,4.17924031072928,2.91426545442384));
#41795=CARTESIAN_POINT('Ctrl Pts',(-8.30323722853692,3.85721688860602,3.1881762018038));
#41796=CARTESIAN_POINT('Ctrl Pts',(-8.28545952434312,3.36281797574608,3.49265111290003));
#41797=CARTESIAN_POINT('Ctrl Pts',(-8.28050056801215,3.21860185244998,3.56989604452081));
#41798=CARTESIAN_POINT('Ctrl Pts',(-8.27015399752479,2.90252714976439,3.71496809787658));
#41799=CARTESIAN_POINT('Ctrl Pts',(-8.2648716942581,2.73042207311042,3.77985135598681));
#41800=CARTESIAN_POINT('Ctrl Pts',(-8.25552815725815,2.4168523873549,3.87344601601425));
#41801=CARTESIAN_POINT('Ctrl Pts',(-8.25145344246759,2.27805406488937,3.90676794863051));
#41802=CARTESIAN_POINT('Ctrl Pts',(-8.23504627533598,1.72859796267692,4.00729376382368));
#41803=CARTESIAN_POINT('Ctrl Pts',(-8.22206902177147,1.30810857964516,4.01761971390415));
#41804=CARTESIAN_POINT('Ctrl Pts',(-8.20433605616193,0.73372767392041,3.94396573773987));
#41805=CARTESIAN_POINT('Ctrl Pts',(-8.19936022590262,0.572500695069959,
3.91329702216157));
#41806=CARTESIAN_POINT('Ctrl Pts',(-8.18892380739151,0.232662762010082,
3.82666841761553));
#41807=CARTESIAN_POINT('Ctrl Pts',(-8.1835739289633,0.055804878837681,3.76800568319578));
#41808=CARTESIAN_POINT('Ctrl Pts',(-8.17414828388991,-0.24931686021425,
3.64199374421524));
#41809=CARTESIAN_POINT('Ctrl Pts',(-8.17005862117415,-0.378491633600513,
3.58018568526668));
#41810=CARTESIAN_POINT('Ctrl Pts',(-8.15385090523078,-0.862176067366126,
3.31524999388456));
#41811=CARTESIAN_POINT('Ctrl Pts',(-8.14112155289688,-1.1896129757399,3.06391314723039));
#41812=CARTESIAN_POINT('Ctrl Pts',(-8.12355106804285,-1.58751208926258,
2.65094746033788));
#41813=CARTESIAN_POINT('Ctrl Pts',(-8.11851185870086,-1.69521545317531,
2.52454464835922));
#41814=CARTESIAN_POINT('Ctrl Pts',(-8.10774692043597,-1.91202275223654,
2.23539747847899));
#41815=CARTESIAN_POINT('Ctrl Pts',(-8.10215212382597,-2.01718949125223,
2.07111639983117));
#41816=CARTESIAN_POINT('Ctrl Pts',(-8.09242214684246,-2.17897934001922,
1.77120100599946));
#41817=CARTESIAN_POINT('Ctrl Pts',(-8.08827176158543,-2.24068067267691,
1.63990604557891));
#41818=CARTESIAN_POINT('Ctrl Pts',(-8.07277346807375,-2.43777648938402,
1.15189321164572));
#41819=CARTESIAN_POINT('Ctrl Pts',(-8.06092748807461,-2.52942794093955,
0.778194848400361));
#41820=CARTESIAN_POINT('Ctrl Pts',(-8.0439329940201,-2.58532310514898,0.227278919275189));
#41821=CARTESIAN_POINT('Ctrl Pts',(-8.0386545985082,-2.59180184588262,0.0539466788231075));
#41822=CARTESIAN_POINT('Ctrl Pts',(-8.02676493514619,-2.58083524313243,
-0.343816479428662));
#41823=CARTESIAN_POINT('Ctrl Pts',(-8.02035871879499,-2.55569647006428,
-0.566535524687872));
#41824=CARTESIAN_POINT('Ctrl Pts',(-8.0095271388049,-2.48102652403134,-0.938235635197529));
#41825=CARTESIAN_POINT('Ctrl Pts',(-8.00508399092669,-2.44177743325494,
-1.08737917292164));
#41826=CARTESIAN_POINT('Ctrl Pts',(-7.99246936242149,-2.30960412619161,
-1.49174308730004));
#41827=CARTESIAN_POINT('Ctrl Pts',(-7.98414661604672,-2.19915574141526,
-1.74055185695866));
#41828=CARTESIAN_POINT('Ctrl Pts',(-7.96641282816883,-1.91427179669719,
-2.24147382111215));
#41829=CARTESIAN_POINT('Ctrl Pts',(-7.95699926375979,-1.73327257169777,
-2.4902085265274));
#41830=CARTESIAN_POINT('Ctrl Pts',(-7.94367664760113,-1.42749794893696,
-2.8222559768075));
#41831=CARTESIAN_POINT('Ctrl Pts',(-7.93950682957255,-1.32326419294921,
-2.92355007450332));
#41832=CARTESIAN_POINT('Ctrl Pts',(-7.92909444821615,-1.04808197102979,
-3.16273656141954));
#41833=CARTESIAN_POINT('Ctrl Pts',(-7.92282961016138,-0.871721932073699,
-3.29180018360956));
#41834=CARTESIAN_POINT('Ctrl Pts',(-7.91104846735441,-0.535623827938592,
-3.49747550084486));
#41835=CARTESIAN_POINT('Ctrl Pts',(-7.9057109061316,-0.380428706964164,
-3.57897918373674));
#41836=CARTESIAN_POINT('Ctrl Pts',(-7.88857829163988,0.129325875921738,
-3.80611417105785));
#41837=CARTESIAN_POINT('Ctrl Pts',(-7.87666038551479,0.501701075827734,
-3.91275031985627));
#41838=CARTESIAN_POINT('Ctrl Pts',(-7.86126248587222,1.02093550287008,-3.98298630746433));
#41839=CARTESIAN_POINT('Ctrl Pts',(-7.85725423808037,1.16073590492058,-3.99430115306265));
#41840=CARTESIAN_POINT('Ctrl Pts',(-7.84749742147575,1.50232643507186,-4.00360908631064));
#41841=CARTESIAN_POINT('Ctrl Pts',(-7.84172746727987,1.70292087807701,-3.99362152230159));
#41842=CARTESIAN_POINT('Ctrl Pts',(-7.83062259574907,2.07207861054924,-3.94695937181635));
#41843=CARTESIAN_POINT('Ctrl Pts',(-7.82542178055052,2.24008519917537,-3.91467830952474));
#41844=CARTESIAN_POINT('Ctrl Pts',(-7.80796444285909,2.79114901220283,-3.7723593348863));
#41845=CARTESIAN_POINT('Ctrl Pts',(-7.7955482729733,3.16267514216532,-3.61589653192316));
#41846=CARTESIAN_POINT('Ctrl Pts',(-7.77974656484461,3.62187610157493,-3.33511324646981));
#41847=CARTESIAN_POINT('Ctrl Pts',(-7.77576926878808,3.73666685794663,-3.25621775732238));
#41848=CARTESIAN_POINT('Ctrl Pts',(-7.76616137317479,4.00347215087133,-3.05116023396499));
#41849=CARTESIAN_POINT('Ctrl Pts',(-7.76050972811701,4.14990634499246,-2.91994128613319));
#41850=CARTESIAN_POINT('Ctrl Pts',(-7.74956344298934,4.40422140540033,-2.65542404049085));
#41851=CARTESIAN_POINT('Ctrl Pts',(-7.74439281601866,4.5140925868034,-2.52550074770107));
#41852=CARTESIAN_POINT('Ctrl Pts',(-7.72686007370345,4.85524575071136,-2.06671020327493));
#41853=CARTESIAN_POINT('Ctrl Pts',(-7.71432915419634,5.04748430892309,-1.70824460230927));
#41854=CARTESIAN_POINT('Ctrl Pts',(-7.69843468145297,5.22844258390508,-1.19784564861864));
#41855=CARTESIAN_POINT('Ctrl Pts',(-7.69446426354047,5.26787075238927,-1.06447768018486));
#41856=CARTESIAN_POINT('Ctrl Pts',(-7.68489100187416,5.34574648758367,-0.738358811855705));
#41857=CARTESIAN_POINT('Ctrl Pts',(-7.67926720125676,5.37680047670683,-0.545206265220628));
#41858=CARTESIAN_POINT('Ctrl Pts',(-7.66835808107404,5.40798735545737,-0.180806195381952));
#41859=CARTESIAN_POINT('Ctrl Pts',(-7.6631944340885,5.41167212919348,-0.0109084292610411));
#41860=CARTESIAN_POINT('Ctrl Pts',(-7.64564410891077,5.38831496683481,0.560947118691117));
#41861=CARTESIAN_POINT('Ctrl Pts',(-7.63308645584631,5.3120322444401,0.961350579724166));
#41862=CARTESIAN_POINT('Ctrl Pts',(-7.61717046027468,5.13113362775074,1.47258037647918));
#41863=CARTESIAN_POINT('Ctrl Pts',(-7.61320169525421,5.07784838133224,1.60098553140313));
#41864=CARTESIAN_POINT('Ctrl Pts',(-7.60363636244069,4.93322578023245,1.90317190361519));
#41865=CARTESIAN_POINT('Ctrl Pts',(-7.5980188583853,4.83591371367482,2.07262712512135));
#41866=CARTESIAN_POINT('Ctrl Pts',(-7.58711818588042,4.63100129230278,2.375233244504));
#41867=CARTESIAN_POINT('Ctrl Pts',(-7.58195616510477,4.52698715077923,2.50955735486238));
#41868=CARTESIAN_POINT('Ctrl Pts',(-7.56440132806299,4.1488985576194,2.93942952767956));
#41869=CARTESIAN_POINT('Ctrl Pts',(-7.55183700381181,3.83748071484364,3.20274145831215));
#41870=CARTESIAN_POINT('Ctrl Pts',(-7.53591553578612,3.37499075557905,3.48627865256812));
#41871=CARTESIAN_POINT('Ctrl Pts',(-7.53194708936957,3.25277819857129,3.55252490237572));
#41872=CARTESIAN_POINT('Ctrl Pts',(-7.52238434054904,2.95029152413514,3.69630262689152));
#41873=CARTESIAN_POINT('Ctrl Pts',(-7.51676910519429,2.76810053092606,3.76672276634242));
#41874=CARTESIAN_POINT('Ctrl Pts',(-7.50587110941699,2.41850472499507,3.87291915771657));
#41875=CARTESIAN_POINT('Ctrl Pts',(-7.50070928331498,2.25314440176428,3.91185336740775));
#41876=CARTESIAN_POINT('Ctrl Pts',(-7.48315412510653,1.68877799028105,4.00800581000016));
#41877=CARTESIAN_POINT('Ctrl Pts',(-7.47058925348492,1.28103513176941,4.01666501820596));
#41878=CARTESIAN_POINT('Ctrl Pts',(-7.4546672235838,0.743155605801197,3.94596580112017));
#41879=CARTESIAN_POINT('Ctrl Pts',(-7.45069871652713,0.606485421942205,
3.92053935865417));
#41880=CARTESIAN_POINT('Ctrl Pts',(-7.44113632603371,0.280935375524862,
3.84192110553983));
#41881=CARTESIAN_POINT('Ctrl Pts',(-7.4355215328099,0.0950404895053442,
3.78199857509237));
#41882=CARTESIAN_POINT('Ctrl Pts',(-7.42462540897175,-0.243425406291763,
3.64455115422927));
#41883=CARTESIAN_POINT('Ctrl Pts',(-7.41946507362647,-0.396396210947056,
3.570771188204));
#41884=CARTESIAN_POINT('Ctrl Pts',(-7.40191019799819,-0.895509931253181,
3.29036186734888));
#41885=CARTESIAN_POINT('Ctrl Pts',(-7.38934378813035,-1.21787775746866,
3.04047992587711));
#41886=CARTESIAN_POINT('Ctrl Pts',(-7.37342249874026,-1.5913904607136,2.6470668369273));
#41887=CARTESIAN_POINT('Ctrl Pts',(-7.36945579441319,-1.68156625222372,
2.54135046778569));
#41888=CARTESIAN_POINT('Ctrl Pts',(-7.35988526470485,-1.88529164648697,
2.27515597070471));
#41889=CARTESIAN_POINT('Ctrl Pts',(-7.35426042843444,-1.99223519290982,
2.11129129683516));
#41890=CARTESIAN_POINT('Ctrl Pts',(-7.34334831524404,-2.16897000334207,
1.79096734915893));
#41891=CARTESIAN_POINT('Ctrl Pts',(-7.33818263269869,-2.24145480846847,
1.6371831953705));
#41892=CARTESIAN_POINT('Ctrl Pts',(-7.32061520538891,-2.45285389888773,
1.10470660786811));
#41893=CARTESIAN_POINT('Ctrl Pts',(-7.30804205117675,-2.54602121212175,
0.707359986720556));
#41894=CARTESIAN_POINT('Ctrl Pts',(-7.29210548837713,-2.58848143003375,
0.166017920341317));
#41895=CARTESIAN_POINT('Ctrl Pts',(-7.28813054711029,-2.59195385365601,
0.0268232157132258));
#41896=CARTESIAN_POINT('Ctrl Pts',(-7.2786095950252,-2.58256970679197,-0.306399647676443));
#41897=CARTESIAN_POINT('Ctrl Pts',(-7.27304288623182,-2.5627955459446,-0.49893328789067));
#41898=CARTESIAN_POINT('Ctrl Pts',(-7.26220556584929,-2.49932381543594,
-0.856657746582581));
#41899=CARTESIAN_POINT('Ctrl Pts',(-7.25705175808226,-2.45914226539997,
-1.02143552756869));
#41900=CARTESIAN_POINT('Ctrl Pts',(-7.23954859536847,-2.28960376308852,
-1.56645372978732));
#41901=CARTESIAN_POINT('Ctrl Pts',(-7.22702922529765,-2.1133726816539,-1.9325863528688));
#41902=CARTESIAN_POINT('Ctrl Pts',(-7.21116533333725,-1.80820099873601,
-2.3787079603919));
#41903=CARTESIAN_POINT('Ctrl Pts',(-7.20721311584906,-1.72408161752784,
-2.48868157581462));
#41904=CARTESIAN_POINT('Ctrl Pts',(-7.19752151294438,-1.50366283508033,
-2.7473125400986));
#41905=CARTESIAN_POINT('Ctrl Pts',(-7.19176142535338,-1.36208549037252,
-2.8896389522497));
#41906=CARTESIAN_POINT('Ctrl Pts',(-7.18071866119574,-1.08172397574098,
-3.13164072702576));
#41907=CARTESIAN_POINT('Ctrl Pts',(-7.17557244423305,-0.946705733537348,
-3.2339897351788));
#41908=CARTESIAN_POINT('Ctrl Pts',(-7.1593907426499,-0.507092836481076,
-3.5260056698966));
#41909=CARTESIAN_POINT('Ctrl Pts',(-7.14821761855518,-0.181767730933443,
-3.68511173709286));
#41910=CARTESIAN_POINT('Ctrl Pts',(-7.13225496889577,0.32742237991983,-3.85413806620003));
#41911=CARTESIAN_POINT('Ctrl Pts',(-7.12715648571192,0.49900937139241,-3.89853576118905));
#41912=CARTESIAN_POINT('Ctrl Pts',(-7.11797189453762,0.814410352902328,
-3.95766919426007));
#41913=CARTESIAN_POINT('Ctrl Pts',(-7.11387693386829,0.956304762310888,
-3.97632621261017));
#41914=CARTESIAN_POINT('Ctrl Pts',(-7.10660144309169,1.20284245916133,-3.99507587614319));
#41915=CARTESIAN_POINT('Ctrl Pts',(-7.10350803129759,1.30643915417203,-3.99886470380827));
#41916=CARTESIAN_POINT('Ctrl Pts',(-7.10038389721637,1.41002651567319,-3.9986428669731));
#41917=CARTESIAN_POINT('',(-6.35049707793183,1.40999999927913,-3.999138981278));
#41918=CARTESIAN_POINT('Ctrl Pts',(-7.10040561164375,1.41002774730112,-3.99860519579024));
#41919=CARTESIAN_POINT('Ctrl Pts',(-7.09264853948305,1.65968390616741,-3.99846447658792));
#41920=CARTESIAN_POINT('Ctrl Pts',(-7.08470884553314,1.90937917061482,-3.97503575881809));
#41921=CARTESIAN_POINT('Ctrl Pts',(-7.07348439443978,2.26828108839417,-3.90720290721754));
#41922=CARTESIAN_POINT('Ctrl Pts',(-7.06998824899606,2.38100516871555,-3.88080332604567));
#41923=CARTESIAN_POINT('Ctrl Pts',(-7.06104116063078,2.67382435338878,-3.79850250412021));
#41924=CARTESIAN_POINT('Ctrl Pts',(-7.055726979142,2.85150016068744,-3.73462977797167));
#41925=CARTESIAN_POINT('Ctrl Pts',(-7.04639135396558,3.15444270784623,-3.60097999533984));
#41926=CARTESIAN_POINT('Ctrl Pts',(-7.04236736848393,3.28198168245327,-3.53637486560756));
#41927=CARTESIAN_POINT('Ctrl Pts',(-7.03507432994842,3.50094605759099,-3.41026339980517));
#41928=CARTESIAN_POINT('Ctrl Pts',(-7.03184207956834,3.5938288091045,-3.35152154680779));
#41929=CARTESIAN_POINT('Ctrl Pts',(-7.02280012435035,3.84006991300434,-3.18104043885625));
#41930=CARTESIAN_POINT('Ctrl Pts',(-7.01686679266736,3.98812095015316,-3.06209221266588));
#41931=CARTESIAN_POINT('Ctrl Pts',(-7.00588507965679,4.24450822583334,-2.82458677088115));
#41932=CARTESIAN_POINT('Ctrl Pts',(-7.0008421448956,4.35547303771764,-2.70879652522094));
#41933=CARTESIAN_POINT('Ctrl Pts',(-6.99233887143207,4.53405647103683,-2.49858968903497));
#41934=CARTESIAN_POINT('Ctrl Pts',(-6.98882592442692,4.60522100925099,-2.40707276472707));
#41935=CARTESIAN_POINT('Ctrl Pts',(-6.98029498517621,4.7724866533641,-2.17124336441763));
#41936=CARTESIAN_POINT('Ctrl Pts',(-6.9753806135466,4.8633994956659,-2.02345584474559));
#41937=CARTESIAN_POINT('Ctrl Pts',(-6.96615565763097,5.01614960889643,-1.73480647039514));
#41938=CARTESIAN_POINT('Ctrl Pts',(-6.96183915945002,5.08011548494544,-1.59508397302638));
#41939=CARTESIAN_POINT('Ctrl Pts',(-6.95415180342381,5.17698644045154,-1.34655178541396));
#41940=CARTESIAN_POINT('Ctrl Pts',(-6.95082544829128,5.21360798629057,-1.23928760181713));
#41941=CARTESIAN_POINT('Ctrl Pts',(-6.94193504283024,5.29679860924318,-0.956414591520403));
#41942=CARTESIAN_POINT('Ctrl Pts',(-6.9362719925443,5.33606680270269,-0.778939748243768));
#41943=CARTESIAN_POINT('Ctrl Pts',(-6.92537916887946,5.38808047222023,-0.435640326624288));
#41944=CARTESIAN_POINT('Ctrl Pts',(-6.92015371441268,5.40280624044388,-0.270070567720667));
#41945=CARTESIAN_POINT('Ctrl Pts',(-6.91140141938467,5.41038251322496,0.0137748843846125));
#41946=CARTESIAN_POINT('Ctrl Pts',(-6.90781775281387,5.40831848296732,0.132006925836137));
#41947=CARTESIAN_POINT('Ctrl Pts',(-6.89902934632707,5.38976170196528,0.429328533989616));
#41948=CARTESIAN_POINT('Ctrl Pts',(-6.89393978297168,5.36638901832164,0.60783464006324));
#41949=CARTESIAN_POINT('Ctrl Pts',(-6.88462602447094,5.30169827724794,0.931350734217961));
#41950=CARTESIAN_POINT('Ctrl Pts',(-6.88039531901273,5.26393730394495,1.07706025500683));
#41951=CARTESIAN_POINT('Ctrl Pts',(-6.87282284039256,5.1838004561804,1.3271752500617));
#41952=CARTESIAN_POINT('Ctrl Pts',(-6.86952325485292,5.14502401023233,1.43263276436424));
#41953=CARTESIAN_POINT('Ctrl Pts',(-6.86058474051734,5.03100590108868,1.70615350829162));
#41954=CARTESIAN_POINT('Ctrl Pts',(-6.85483951679451,4.94852610480644,1.87091019134176));
#41955=CARTESIAN_POINT('Ctrl Pts',(-6.84391930736957,4.77191220217314,2.17066711142937));
#41956=CARTESIAN_POINT('Ctrl Pts',(-6.83874926067223,4.67995002126213,2.30699930816388));
#41957=CARTESIAN_POINT('Ctrl Pts',(-6.83007196160328,4.50851272045314,2.53027683615581));
#41958=CARTESIAN_POINT('Ctrl Pts',(-6.82650914570957,4.43289105125086,2.6202947692206));
#41959=CARTESIAN_POINT('Ctrl Pts',(-6.81755327328165,4.22745669818194,2.84378511200389));
#41960=CARTESIAN_POINT('Ctrl Pts',(-6.81229167157356,4.09197825925759,2.9718348929275));
#41961=CARTESIAN_POINT('Ctrl Pts',(-6.80290679013607,3.83505888724771,3.18288313349167));
#41962=CARTESIAN_POINT('Ctrl Pts',(-6.79877791300063,3.71674561959577,3.26967036479431));
#41963=CARTESIAN_POINT('Ctrl Pts',(-6.79133081516892,3.50058149852532,3.41061310926603));
#41964=CARTESIAN_POINT('Ctrl Pts',(-6.78805166651218,3.40468773490404,3.46754722413532));
#41965=CARTESIAN_POINT('Ctrl Pts',(-6.77849957510682,3.12601985984053,3.61744959952603));
#41966=CARTESIAN_POINT('Ctrl Pts',(-6.77207200824075,2.93822694029586,3.70052768487301));
#41967=CARTESIAN_POINT('Ctrl Pts',(-6.7608990332163,2.60283850902814,3.81935006854174));
#41968=CARTESIAN_POINT('Ctrl Pts',(-6.75615422202189,2.45756574588288,3.8618045463782));
#41969=CARTESIAN_POINT('Ctrl Pts',(-6.74802154077296,2.19982294215036,3.92154433453711));
#41970=CARTESIAN_POINT('Ctrl Pts',(-6.74459021637031,2.08813236287482,3.94247816661047));
#41971=CARTESIAN_POINT('Ctrl Pts',(-6.73577048954965,1.79140335578528,3.98493518026796));
#41972=CARTESIAN_POINT('Ctrl Pts',(-6.73051500342436,1.6054027348797,3.9983293358653));
#41973=CARTESIAN_POINT('Ctrl Pts',(-6.71933816238249,1.20939494222431,3.9992549221185));
#41974=CARTESIAN_POINT('Ctrl Pts',(-6.71341488875577,0.999400629268839,
3.98323814803905));
#41975=CARTESIAN_POINT('Ctrl Pts',(-6.70347327430911,0.668190190731935,
3.93131425303137));
#41976=CARTESIAN_POINT('Ctrl Pts',(-6.69964972193144,0.545364264772287,
3.90603566386308));
#41977=CARTESIAN_POINT('Ctrl Pts',(-6.6900283600526,0.244337374723786,3.82925242751296));
#41978=CARTESIAN_POINT('Ctrl Pts',(-6.6841627211255,0.0678103802409079,
3.77095870914652));
#41979=CARTESIAN_POINT('Ctrl Pts',(-6.67337864743503,-0.251317973649497,
3.64055277063818));
#41980=CARTESIAN_POINT('Ctrl Pts',(-6.66844317053658,-0.395227860993703,
3.57153050297422));
#41981=CARTESIAN_POINT('Ctrl Pts',(-6.66007513270807,-0.639313085021569,
3.4358517989492));
#41982=CARTESIAN_POINT('Ctrl Pts',(-6.65658987000914,-0.741319442714824,
3.37291345569331));
#41983=CARTESIAN_POINT('Ctrl Pts',(-6.64802726253102,-0.988472565784273,
3.20464366323693));
#41984=CARTESIAN_POINT('Ctrl Pts',(-6.64301275132767,-1.12989126015751,
3.09374754301853));
#41985=CARTESIAN_POINT('Ctrl Pts',(-6.6339919336344,-1.36626465943441,2.88129956958178));
#41986=CARTESIAN_POINT('Ctrl Pts',(-6.63001547809971,-1.46446248742735,
2.78337082473436));
#41987=CARTESIAN_POINT('Ctrl Pts',(-6.62218341247131,-1.64141488645966,
2.5873616125255));
#41988=CARTESIAN_POINT('Ctrl Pts',(-6.61835047027259,-1.72110213433034,
2.49017371941394));
#41989=CARTESIAN_POINT('Ctrl Pts',(-6.60868881929315,-1.90734550988093,
2.23997675687712));
#41990=CARTESIAN_POINT('Ctrl Pts',(-6.60279163931173,-2.00823906322116,
2.08268657418761));
#41991=CARTESIAN_POINT('Ctrl Pts',(-6.5922404165828,-2.17026678416869,1.78680482365681));
#41992=CARTESIAN_POINT('Ctrl Pts',(-6.58756310012162,-2.2353280492693,1.65031709481824));
#41993=CARTESIAN_POINT('Ctrl Pts',(-6.57957839978225,-2.33582817755596,
1.40435358487513));
#41994=CARTESIAN_POINT('Ctrl Pts',(-6.57623003568454,-2.37452690980641,
1.29646580053329));
#41995=CARTESIAN_POINT('Ctrl Pts',(-6.56836257095053,-2.45580442423401,
1.03498848397479));
#41996=CARTESIAN_POINT('Ctrl Pts',(-6.56389070096702,-2.49397874547159,
0.880032145100022));
#41997=CARTESIAN_POINT('Ctrl Pts',(-6.55472662491674,-2.55264024750825,
0.56118595528033));
#41998=CARTESIAN_POINT('Ctrl Pts',(-6.55003117462333,-2.57245884526863,
0.397184356979848));
#41999=CARTESIAN_POINT('Ctrl Pts',(-6.54158642076005,-2.58898539341239,
0.112147995876195));
#42000=CARTESIAN_POINT('Ctrl Pts',(-6.53791897762239,-2.59045416366361,
-0.00851120688142535));
#42001=CARTESIAN_POINT('Ctrl Pts',(-6.52894812416622,-2.58091616443174,
-0.298783773648617));
#42002=CARTESIAN_POINT('Ctrl Pts',(-6.52358767827291,-2.56453412952355,
-0.46830403049804));
#42003=CARTESIAN_POINT('Ctrl Pts',(-6.51276365501153,-2.50968827107301,
-0.809199611323964));
#42004=CARTESIAN_POINT('Ctrl Pts',(-6.50730232689531,-2.47053421558778,
-0.980507490960601));
#42005=CARTESIAN_POINT('Ctrl Pts',(-6.49859957075455,-2.38757900086817,
-1.25771032018614));
#42006=CARTESIAN_POINT('Ctrl Pts',(-6.49526864637286,-2.35025216690491,
-1.36528598131246));
#42007=CARTESIAN_POINT('Ctrl Pts',(-6.48751837186656,-2.25110865134264,
-1.6158597727343));
#42008=CARTESIAN_POINT('Ctrl Pts',(-6.4831432271011,-2.18535260593672,-1.75727087972514));
#42009=CARTESIAN_POINT('Ctrl Pts',(-6.47394310377158,-2.03115235522827,
-2.04393838762632));
#42010=CARTESIAN_POINT('Ctrl Pts',(-6.46911221099969,-1.94119644121271,
-2.18836830501301));
#42011=CARTESIAN_POINT('Ctrl Pts',(-6.46059714177034,-1.77364756358404,
-2.42244253864324));
#42012=CARTESIAN_POINT('Ctrl Pts',(-6.45700955059748,-1.70070330793377,
-2.51526801224145));
#42013=CARTESIAN_POINT('Ctrl Pts',(-6.44831688368771,-1.51726468619222,
-2.72864293314367));
#42014=CARTESIAN_POINT('Ctrl Pts',(-6.44315872852927,-1.40306784295126,
-2.84612409470512));
#42015=CARTESIAN_POINT('Ctrl Pts',(-6.43223109663733,-1.14584714399316,
-3.08042436512098));
#42016=CARTESIAN_POINT('Ctrl Pts',(-6.42646797975804,-1.00096605520036,
-3.19527318558294));
#42017=CARTESIAN_POINT('Ctrl Pts',(-6.4175935758287,-0.75789395628627,-3.36186569224979));
#42018=CARTESIAN_POINT('Ctrl Pts',(-6.41436575114532,-0.664555757280254,
-3.4202649657445));
#42019=CARTESIAN_POINT('Ctrl Pts',(-6.40704049248205,-0.443558176644393,
-3.54612460119316));
#42020=CARTESIAN_POINT('Ctrl Pts',(-6.40297937944882,-0.314323736959716,
-3.61071635027914));
#42021=CARTESIAN_POINT('Ctrl Pts',(-6.39365712910819,-0.0110628974216484,
-3.74235727491184));
#42022=CARTESIAN_POINT('Ctrl Pts',(-6.38838974829826,0.165027719985866,
-3.80462796653876));
#42023=CARTESIAN_POINT('Ctrl Pts',(-6.37940441536318,0.458709115427309,
-3.88575132598774));
#42024=CARTESIAN_POINT('Ctrl Pts',(-6.37581931929682,0.574095268851708,
-3.91211444104551));
#42025=CARTESIAN_POINT('Ctrl Pts',(-6.36475154640872,0.927603027900314,
-3.97660210601769));
#42026=CARTESIAN_POINT('Ctrl Pts',(-6.35708770070065,1.16880502641396,-3.99846926139206));
#42027=CARTESIAN_POINT('Ctrl Pts',(-6.34959438835625,1.40997225269887,-3.99860519579024));
#42028=CARTESIAN_POINT('',(-6.5809401104541,1.40999999992274,-3.59999993641013));
#42029=CARTESIAN_POINT('',(-6.580940107676,1.41,-3.6));
#42030=CARTESIAN_POINT('Ctrl Pts',(-9.08096181831227,-1.70608631403884,
1.79907083381568));
#42031=CARTESIAN_POINT('Ctrl Pts',(-9.06844586670953,-1.89532978119226,
1.47248228906589));
#42032=CARTESIAN_POINT('Ctrl Pts',(-9.05389861244493,-2.06808131659788,
1.06106952675657));
#42033=CARTESIAN_POINT('Ctrl Pts',(-9.02143148332091,-2.2174468266351,0.0942360700324087));
#42034=CARTESIAN_POINT('Ctrl Pts',(-9.00581496806962,-2.19733524992031,
-0.385795687504495));
#42035=CARTESIAN_POINT('Ctrl Pts',(-8.97436976361075,-1.97759186945788,
-1.30821422968742));
#42036=CARTESIAN_POINT('Ctrl Pts',(-8.95892749944944,-1.7777422252897,-1.73815589466842));
#42037=CARTESIAN_POINT('Ctrl Pts',(-8.92787976811585,-1.22380952851888,
-2.49313866036759));
#42038=CARTESIAN_POINT('Ctrl Pts',(-8.91259810097365,-0.880327472077836,
-2.81351240010763));
#42039=CARTESIAN_POINT('Ctrl Pts',(-8.87894041754877,-0.0201454942556745,
-3.35073711466932));
#42040=CARTESIAN_POINT('Ctrl Pts',(-8.86328101540959,0.44237879573452,-3.48733627110525));
#42041=CARTESIAN_POINT('Ctrl Pts',(-8.8354748649651,1.27037395437224,-3.62272692428968));
#42042=CARTESIAN_POINT('Ctrl Pts',(-8.82056291466372,1.72790382396507,-3.61408512036349));
#42043=CARTESIAN_POINT('Ctrl Pts',(-8.78981466175988,2.63331213616278,-3.41907230663782));
#42044=CARTESIAN_POINT('Ctrl Pts',(-8.77401256964824,3.07790206736605,-3.22265134720344));
#42045=CARTESIAN_POINT('Ctrl Pts',(-8.74528579717737,3.78929212861787,-2.72756811571601));
#42046=CARTESIAN_POINT('Ctrl Pts',(-8.72998723185347,4.13772490077609,-2.41136229140778));
#42047=CARTESIAN_POINT('Ctrl Pts',(-8.69651879481636,4.68454239160939,-1.56386495711761));
#42048=CARTESIAN_POINT('Ctrl Pts',(-8.68090280181185,4.86168791594835,-1.11730839831426));
#42049=CARTESIAN_POINT('Ctrl Pts',(-8.64945534790638,5.0367005821264,-0.185338695322912));
#42050=CARTESIAN_POINT('Ctrl Pts',(-8.63400985998099,5.02931382570696,0.28881546192218));
#42051=CARTESIAN_POINT('Ctrl Pts',(-8.60295652168341,4.83089760378159,1.20411899127373));
#42052=CARTESIAN_POINT('Ctrl Pts',(-8.58767324940446,4.64768240357197,1.63666659383711));
#42053=CARTESIAN_POINT('Ctrl Pts',(-8.55402240736755,4.08104577128213,2.47750689993866));
#42054=CARTESIAN_POINT('Ctrl Pts',(-8.53836750072557,3.71444438472004,2.79062938894395));
#42055=CARTESIAN_POINT('Ctrl Pts',(-8.51055544369505,3.01325307179545,3.25164727376077));
#42056=CARTESIAN_POINT('Ctrl Pts',(-8.49564682586967,2.59196492057787,3.4300699355234));
#42057=CARTESIAN_POINT('Ctrl Pts',(-8.46490396330893,1.68581697483343,3.62085553562213));
#42058=CARTESIAN_POINT('Ctrl Pts',(-8.44910111676051,1.19975277292987,3.62259872586791));
#42059=CARTESIAN_POINT('Ctrl Pts',(-8.42038172893544,0.348598058934349,
3.46032176848038));
#42060=CARTESIAN_POINT('Ctrl Pts',(-8.40508398769246,-0.0984315066368924,
3.31357798233121));
#42061=CARTESIAN_POINT('Ctrl Pts',(-8.37161360411923,-0.943177717951458,
2.76242525451422));
#42062=CARTESIAN_POINT('Ctrl Pts',(-8.35599554789019,-1.28693865774261,
2.42674063682566));
#42063=CARTESIAN_POINT('Ctrl Pts',(-8.32454904505759,-1.82646306968818,
1.64695414520521));
#42064=CARTESIAN_POINT('Ctrl Pts',(-8.30910652452477,-2.01291298468063,
1.21103527034423));
#42065=CARTESIAN_POINT('Ctrl Pts',(-8.27804979542418,-2.20468934191018,
0.294218193195978));
#42066=CARTESIAN_POINT('Ctrl Pts',(-8.26276355706457,-2.21359613350388,
-0.17554373755032));
#42067=CARTESIAN_POINT('Ctrl Pts',(-8.22911620634852,-2.03870729715697,
-1.17419294066118));
#42068=CARTESIAN_POINT('Ctrl Pts',(-8.21346469756575,-1.83160449981305,
-1.60944010832624));
#42069=CARTESIAN_POINT('Ctrl Pts',(-8.18564692764263,-1.37897885840424,
-2.31628097671549));
#42070=CARTESIAN_POINT('Ctrl Pts',(-8.17074246494018,-1.06701032516302,
-2.65076002294469));
#42071=CARTESIAN_POINT('Ctrl Pts',(-8.14000600973343,-0.317446084704328,
-3.19417423343643));
#42072=CARTESIAN_POINT('Ctrl Pts',(-8.12420228432081,0.125743998114902,
-3.39384267259264));
#42073=CARTESIAN_POINT('Ctrl Pts',(-8.09549084818321,0.968921924879492,
-3.59243206163479));
#42074=CARTESIAN_POINT('Ctrl Pts',(-8.08019418646456,1.43691188026914,-3.64066439324238));
#42075=CARTESIAN_POINT('Ctrl Pts',(-8.04672214409242,2.43299215640587,-3.48167859570911));
#42076=CARTESIAN_POINT('Ctrl Pts',(-8.03110175186132,2.88378118790837,-3.31519900874102));
#42077=CARTESIAN_POINT('Ctrl Pts',(-7.99965634959557,3.69423168855652,-2.82298744252999));
#42078=CARTESIAN_POINT('Ctrl Pts',(-7.98421719987669,4.04210919775715,-2.50100896810475));
#42079=CARTESIAN_POINT('Ctrl Pts',(-7.95315659758425,4.59096715371532,-1.74186823207489));
#42080=CARTESIAN_POINT('Ctrl Pts',(-7.93786697424626,4.79058036633025,-1.31641162082662));
#42081=CARTESIAN_POINT('Ctrl Pts',(-7.90422322792772,5.03780997820345,-0.333276150020889));
#42082=CARTESIAN_POINT('Ctrl Pts',(-7.88857555087737,5.02614425340102,0.148461360209211));
#42083=CARTESIAN_POINT('Ctrl Pts',(-7.86075164923162,4.9008256457112,0.978580261358042));
#42084=CARTESIAN_POINT('Ctrl Pts',(-7.84585197180134,4.75227370220379,1.41101213498212));
#42085=CARTESIAN_POINT('Ctrl Pts',(-7.81602824355066,4.30310920504431,2.1889878650182));
#42086=CARTESIAN_POINT('Ctrl Pts',(-7.80112856612061,4.00288818883333,2.53385355868915));
#42087=CARTESIAN_POINT('Ctrl Pts',(-7.77330466447505,3.34664343612141,3.05744210708992));
#42088=CARTESIAN_POINT('Ctrl Pts',(-7.7576569874249,2.93527937670711,3.30841367623759));
#42089=CARTESIAN_POINT('Ctrl Pts',(-7.72401324110639,1.9602442776905,3.58587428719052));
#42090=CARTESIAN_POINT('Ctrl Pts',(-7.7087236177683,1.4919814378338,3.62573247975904));
#42091=CARTESIAN_POINT('Ctrl Pts',(-7.67766301547583,0.560117297405548,
3.52997791484458));
#42092=CARTESIAN_POINT('Ctrl Pts',(-7.6622238657569,0.107337004481931,3.38969639168412));
#42093=CARTESIAN_POINT('Ctrl Pts',(-7.63077846349124,-0.724155966216571,
2.93393145271847));
#42094=CARTESIAN_POINT('Ctrl Pts',(-7.61515807126026,-1.09372603349347,
2.62677649317388));
#42095=CARTESIAN_POINT('Ctrl Pts',(-7.58168602888828,-1.72945191106649,
1.84363856859722));
#42096=CARTESIAN_POINT('Ctrl Pts',(-7.56638936716971,-1.92167646430538,
1.41423121270979));
#42097=CARTESIAN_POINT('Ctrl Pts',(-7.53767793103207,-2.17128197185495,
0.584723013700023));
#42098=CARTESIAN_POINT('Ctrl Pts',(-7.52187420561931,-2.21995907262114,
0.101074923695193));
#42099=CARTESIAN_POINT('Ctrl Pts',(-7.49113775041247,-2.12413068178685,
-0.819773855556126));
#42100=CARTESIAN_POINT('Ctrl Pts',(-7.47623328771001,-1.99044759733927,
-1.25718605363888));
#42101=CARTESIAN_POINT('Ctrl Pts',(-7.44841551778689,-1.60461826958535,
-2.00259179169766));
#42102=CARTESIAN_POINT('Ctrl Pts',(-7.43276400900423,-1.33123456413401,
-2.39957165922484));
#42103=CARTESIAN_POINT('Ctrl Pts',(-7.39911665828806,-0.553823402944175,
-3.05035443589482));
#42104=CARTESIAN_POINT('Ctrl Pts',(-7.38383041992828,-0.142544241390186,
-3.27752189348148));
#42105=CARTESIAN_POINT('Ctrl Pts',(-7.35277369082752,0.747330816658265,
-3.56984723484916));
#42106=CARTESIAN_POINT('Ctrl Pts',(-7.33733117029458,1.21807259377297,-3.62633630936248));
#42107=CARTESIAN_POINT('Ctrl Pts',(-7.30588466746204,2.16314971101677,-3.5489877084657));
#42108=CARTESIAN_POINT('Ctrl Pts',(-7.29026661123315,2.62574158749036,-3.41912431062187));
#42109=CARTESIAN_POINT('Ctrl Pts',(-7.25679622765995,3.52542695680216,-2.96312899578099));
#42110=CARTESIAN_POINT('Ctrl Pts',(-7.2414984864169,3.87602558624035,-2.64936192882806));
#42111=CARTESIAN_POINT('Ctrl Pts',(-7.21277909859177,4.44213891078422,-1.99337880265077));
#42112=CARTESIAN_POINT('Ctrl Pts',(-7.19697625204333,4.68366136469929,-1.57156326080924));
#42113=CARTESIAN_POINT('Ctrl Pts',(-7.16623338948259,4.97151016120934,-0.691423320158281));
#42114=CARTESIAN_POINT('Ctrl Pts',(-7.15132477165723,5.0276356791207,-0.237365748009261));
#42115=CARTESIAN_POINT('Ctrl Pts',(-7.12351271462668,4.97897813573245,0.6003926843047));
#42116=CARTESIAN_POINT('Ctrl Pts',(-7.10785780798465,4.89110679903859,1.07444004263271));
#42117=CARTESIAN_POINT('Ctrl Pts',(-7.07420696594771,4.44623604957347,1.98558191396118));
#42118=CARTESIAN_POINT('Ctrl Pts',(-7.05892369366876,4.16324643751228,2.36052473298372));
#42119=CARTESIAN_POINT('Ctrl Pts',(-7.02787035537127,3.46977843988283,2.99000998636959));
#42120=CARTESIAN_POINT('Ctrl Pts',(-7.01242486744595,3.06284227260822,3.23348418370285));
#42121=CARTESIAN_POINT('Ctrl Pts',(-6.98097741354077,2.16822650117107,3.54790362030417));
#42122=CARTESIAN_POINT('Ctrl Pts',(-6.96536142053655,1.69292441485119,3.61776937546153));
#42123=CARTESIAN_POINT('Ctrl Pts',(-6.93189298349964,0.685561448299596,
3.56796020431103));
#42124=CARTESIAN_POINT('Ctrl Pts',(-6.91659441817572,0.237502785545008,
3.42431148426496));
#42125=CARTESIAN_POINT('Ctrl Pts',(-6.88786764570467,-0.546946900536641,
3.05577123496467));
#42126=CARTESIAN_POINT('Ctrl Pts',(-6.87206555359276,-0.93934740684421,
2.76895553999292));
#42127=CARTESIAN_POINT('Ctrl Pts',(-6.84131730068868,-1.56093761369266,
2.0823553476949));
#42128=CARTESIAN_POINT('Ctrl Pts',(-6.82640535038721,-1.79718657022345,
1.69044375960059));
#42129=CARTESIAN_POINT('Ctrl Pts',(-6.79859919994262,-2.09393240444934,
0.905683591417754));
#42130=CARTESIAN_POINT('Ctrl Pts',(-6.7829397978034,-2.20689620983523,0.436826228201021));
#42131=CARTESIAN_POINT('Ctrl Pts',(-6.74928211437852,-2.17173694839478,
-0.576725573751296));
#42132=CARTESIAN_POINT('Ctrl Pts',(-6.73400044723635,-2.06602617929488,
-1.0343766302434));
#42133=CARTESIAN_POINT('Ctrl Pts',(-6.70295271590285,-1.6891582731651,-1.89158780048352));
#42134=CARTESIAN_POINT('Ctrl Pts',(-6.68751045174163,-1.41674269123005,
-2.27963350176108));
#42135=CARTESIAN_POINT('Ctrl Pts',(-6.65606524728288,-0.727776491008708,
-2.93114612264656));
#42136=CARTESIAN_POINT('Ctrl Pts',(-6.64044873203163,-0.32211258271571,
-3.18857913776016));
#42137=CARTESIAN_POINT('Ctrl Pts',(-6.60798160501411,0.589872447884793,
-3.54264151700872));
#42138=CARTESIAN_POINT('Ctrl Pts',(-6.59343435231527,1.03254206764506,-3.59874068850377));
#42139=CARTESIAN_POINT('Ctrl Pts',(-6.58091840173488,1.40999774666754,-3.59814532547397));
#42140=CARTESIAN_POINT('Ctrl Pts',(-9.674889449625,-0.9664803087391,3.270944531304));
#42141=CARTESIAN_POINT('Ctrl Pts',(-9.647806116292,-1.708634081117,2.731738253352));
#42142=CARTESIAN_POINT('Ctrl Pts',(-9.593639449625,-2.808297225935,1.130720984389));
#42143=CARTESIAN_POINT('Ctrl Pts',(-9.512389449625,-2.580073583318,-1.776527932779));
#42144=CARTESIAN_POINT('Ctrl Pts',(-9.431139449625,-0.5727959484731,-3.891494677932));
#42145=CARTESIAN_POINT('Ctrl Pts',(-9.349889449625,2.318056769223,-4.272116567967));
#42146=CARTESIAN_POINT('Ctrl Pts',(-9.268639449625,4.804227628837,-2.748587901516));
#42147=CARTESIAN_POINT('Ctrl Pts',(-9.187389449625,5.777551391752,-4.35565146506E-7));
#42148=CARTESIAN_POINT('Ctrl Pts',(-9.106139449625,4.804225552094,2.748589643777));
#42149=CARTESIAN_POINT('Ctrl Pts',(-9.024889449625,2.318065076194,4.272110470055));
#42150=CARTESIAN_POINT('Ctrl Pts',(-8.943639449625,-0.5728270996155,3.89151732732));
#42151=CARTESIAN_POINT('Ctrl Pts',(-8.862389449625,-2.57995728572,1.776443433137));
#42152=CARTESIAN_POINT('Ctrl Pts',(-8.781139449625,-2.808731265186,-1.130405635211));
#42153=CARTESIAN_POINT('Ctrl Pts',(-8.699889449625,-1.157182649303,-3.533423784903));
#42154=CARTESIAN_POINT('Ctrl Pts',(-8.618639449625,1.638580009963,-4.361566413001));
#42155=CARTESIAN_POINT('Ctrl Pts',(-8.537389449625,4.332462712197,-3.245723662317));
#42156=CARTESIAN_POINT('Ctrl Pts',(-8.456139449625,5.723780178711,-0.6832356592843));
#42157=CARTESIAN_POINT('Ctrl Pts',(-8.374889449625,5.192410976774,2.183775995627));
#42158=CARTESIAN_POINT('Ctrl Pts',(-8.293639449625,2.975190651644,4.077461050748));
#42159=CARTESIAN_POINT('Ctrl Pts',(-8.212389449625,0.06035221086774,4.153788781534));
#42160=CARTESIAN_POINT('Ctrl Pts',(-8.131139449625,-2.252937308971,2.378739301925));
#42161=CARTESIAN_POINT('Ctrl Pts',(-8.049889449625,-2.933626084714,-0.4565334979991));
#42162=CARTESIAN_POINT('Ctrl Pts',(-7.968639449625,-1.678325629267,-3.088325629786));
#42163=CARTESIAN_POINT('Ctrl Pts',(-7.887389449625,0.9534664986228,-4.343626086017));
#42164=CARTESIAN_POINT('Ctrl Pts',(-7.806139449625,3.788739314919,-3.662937303239));
#42165=CARTESIAN_POINT('Ctrl Pts',(-7.724889449625,5.563788732938,-1.349647810754));
#42166=CARTESIAN_POINT('Ctrl Pts',(-7.643639449625,5.487461232137,1.5651907324));
#42167=CARTESIAN_POINT('Ctrl Pts',(-7.562389449625,3.593775318665,3.782410675374));
#42168=CARTESIAN_POINT('Ctrl Pts',(-7.481139449625,0.726766867171,4.313781303558));
#42169=CARTESIAN_POINT('Ctrl Pts',(-7.399889449625,-1.835733091177,2.922458514209));
#42170=CARTESIAN_POINT('Ctrl Pts',(-7.318639449625,-2.951531224017,0.2285956770673));
#42171=CARTESIAN_POINT('Ctrl Pts',(-7.237389449625,-2.123555111978,-2.567241119733));
#42172=CARTESIAN_POINT('Ctrl Pts',(-7.156139449625,0.2800844841049,-4.218513050568));
#42173=CARTESIAN_POINT('Ctrl Pts',(-7.101972782958,2.216437683334,-4.066685466031));
#42174=CARTESIAN_POINT('Ctrl Pts',(-7.074889449625,3.05448090411,-3.693564584614));
#42175=CARTESIAN_POINT('Ctrl Pts',(-9.581316447316,-0.8712160753873,3.139824562851));
#42176=CARTESIAN_POINT('Ctrl Pts',(-9.554233113983,-1.583619670625,2.622233053807));
#42177=CARTESIAN_POINT('Ctrl Pts',(-9.500066447316,-2.639201420765,1.08539459674));
#42178=CARTESIAN_POINT('Ctrl Pts',(-9.418816447316,-2.420126412902,-1.705313552873));
#42179=CARTESIAN_POINT('Ctrl Pts',(-9.337566447316,-0.4933130530206,-3.735499168218));
#42180=CARTESIAN_POINT('Ctrl Pts',(-9.256316447316,2.281656159615,-4.100863346074));
#42181=CARTESIAN_POINT('Ctrl Pts',(-9.175066447316,4.668165700744,-2.638407262411));
#42182=CARTESIAN_POINT('Ctrl Pts',(-9.093816447316,5.602472543663,-4.181049656672E-7));
#42183=CARTESIAN_POINT('Ctrl Pts',(-9.012566447316,4.66816370725,2.638408934831));
#42184=CARTESIAN_POINT('Ctrl Pts',(-8.931316447316,2.28166413359,4.100857492604));
#42185=CARTESIAN_POINT('Ctrl Pts',(-8.850066447316,-0.4933429554299,3.735520909677));
#42186=CARTESIAN_POINT('Ctrl Pts',(-8.768816447316,-2.420014777241,1.705232440507));
#42187=CARTESIAN_POINT('Ctrl Pts',(-8.687566447316,-2.639618061001,-1.085091888735));
#42188=CARTESIAN_POINT('Ctrl Pts',(-8.606316447316,-1.054273870273,-3.391782001995));
#42189=CARTESIAN_POINT('Ctrl Pts',(-8.525066447316,1.62941708977,-4.186727480392));
#42190=CARTESIAN_POINT('Ctrl Pts',(-8.443816447316,4.215312080335,-3.11561470445));
#42191=CARTESIAN_POINT('Ctrl Pts',(-8.362566447316,5.550856818033,-0.6558472895843));
#42192=CARTESIAN_POINT('Ctrl Pts',(-8.281316447316,5.040788225852,2.096236559566));
#42193=CARTESIAN_POINT('Ctrl Pts',(-8.200066447316,2.912447995233,3.914010842643));
#42194=CARTESIAN_POINT('Ctrl Pts',(-8.118816447316,0.1144545577098,3.987278879338));
#42195=CARTESIAN_POINT('Ctrl Pts',(-8.037566447316,-2.106103811857,2.283384513961));
#42196=CARTESIAN_POINT('Ctrl Pts',(-7.956316447316,-2.759506312963,-0.4382327725412));
#42197=CARTESIAN_POINT('Ctrl Pts',(-7.875066447316,-1.554526171585,-2.964526172083));
#42198=CARTESIAN_POINT('Ctrl Pts',(-7.793816447316,0.9717672242161,-4.169506314214));
#42199=CARTESIAN_POINT('Ctrl Pts',(-7.712566447316,3.693384526433,-3.516103806355));
#42200=CARTESIAN_POINT('Ctrl Pts',(-7.631316447316,5.39727883269,-1.295545463045));
#42201=CARTESIAN_POINT('Ctrl Pts',(-7.550066447316,5.324011016761,1.502448072752));
#42202=CARTESIAN_POINT('Ctrl Pts',(-7.468816447316,3.506235909742,3.630787936533));
#42203=CARTESIAN_POINT('Ctrl Pts',(-7.387566447316,0.7541551355947,4.140857897789));
#42204=CARTESIAN_POINT('Ctrl Pts',(-7.306316447316,-1.705623755341,2.805308050628));
#42205=CARTESIAN_POINT('Ctrl Pts',(-7.225066447316,-2.776693702003,0.2194321288388));
#42206=CARTESIAN_POINT('Ctrl Pts',(-7.143816447316,-1.981908064657,-2.464329996843));
#42207=CARTESIAN_POINT('Ctrl Pts',(-7.062566447316,0.325378583525,-4.049408593792));
#42208=CARTESIAN_POINT('Ctrl Pts',(-7.00839978065,2.184110603928,-3.903667210934));
#42209=CARTESIAN_POINT('Ctrl Pts',(-6.981316447316,2.988559797162,-3.545503354232));
#42210=CARTESIAN_POINT('Ctrl Pts',(-9.487743445008,-0.7759518420355,3.008704594398));
#42211=CARTESIAN_POINT('Ctrl Pts',(-9.460660111674,-1.458605260133,2.512727854262));
#42212=CARTESIAN_POINT('Ctrl Pts',(-9.406493445008,-2.470105615594,1.040068209092));
#42213=CARTESIAN_POINT('Ctrl Pts',(-9.325243445008,-2.260179242486,-1.634099172968));
#42214=CARTESIAN_POINT('Ctrl Pts',(-9.243993445008,-0.4138301575682,-3.579503658505));
#42215=CARTESIAN_POINT('Ctrl Pts',(-9.162743445008,2.245255550006,-3.929610124181));
#42216=CARTESIAN_POINT('Ctrl Pts',(-9.081493445008,4.532103772651,-2.528226623306));
#42217=CARTESIAN_POINT('Ctrl Pts',(-9.000243445008,5.427393695574,-4.006447743584E-7));
#42218=CARTESIAN_POINT('Ctrl Pts',(-8.918993445008,4.532101862406,2.528228225885));
#42219=CARTESIAN_POINT('Ctrl Pts',(-8.837743445008,2.245263190987,3.929604515154));
#42220=CARTESIAN_POINT('Ctrl Pts',(-8.756493445008,-0.4138588112444,3.579524492034));
#42221=CARTESIAN_POINT('Ctrl Pts',(-8.675243445008,-2.260072268762,1.634021447877));
#42222=CARTESIAN_POINT('Ctrl Pts',(-8.593993445008,-2.470504856815,-1.039778142259));
#42223=CARTESIAN_POINT('Ctrl Pts',(-8.512743445008,-0.9513650912439,-3.250140219087));
#42224=CARTESIAN_POINT('Ctrl Pts',(-8.431493445008,1.620254169577,-4.011888547782));
#42225=CARTESIAN_POINT('Ctrl Pts',(-8.350243445008,4.098161448473,-2.985505746582));
#42226=CARTESIAN_POINT('Ctrl Pts',(-8.268993445008,5.377933457354,-0.6284589198844));
#42227=CARTESIAN_POINT('Ctrl Pts',(-8.187743445008,4.88916547493,2.008697123506));
#42228=CARTESIAN_POINT('Ctrl Pts',(-8.106493445008,2.849705338822,3.750560634537));
#42229=CARTESIAN_POINT('Ctrl Pts',(-8.025243445008,0.1685569045517,3.820768977142));
#42230=CARTESIAN_POINT('Ctrl Pts',(-7.943993445008,-1.959270314743,2.188029725996));
#42231=CARTESIAN_POINT('Ctrl Pts',(-7.862743445008,-2.585386541213,-0.4199320470833));
#42232=CARTESIAN_POINT('Ctrl Pts',(-7.781493445008,-1.430726713904,-2.840726714381));
#42233=CARTESIAN_POINT('Ctrl Pts',(-7.700243445008,0.9900679498094,-3.995386542412));
#42234=CARTESIAN_POINT('Ctrl Pts',(-7.618993445008,3.598029737948,-3.369270309471));
#42235=CARTESIAN_POINT('Ctrl Pts',(-7.537743445008,5.230768932443,-1.241443115336));
#42236=CARTESIAN_POINT('Ctrl Pts',(-7.456493445008,5.160560801384,1.439705413104));
#42237=CARTESIAN_POINT('Ctrl Pts',(-7.375243445008,3.418696500819,3.479165197693));
#42238=CARTESIAN_POINT('Ctrl Pts',(-7.293993445008,0.7815434040185,3.96793449202));
#42239=CARTESIAN_POINT('Ctrl Pts',(-7.212743445008,-1.575514419506,2.688157587048));
#42240=CARTESIAN_POINT('Ctrl Pts',(-7.131493445008,-2.601856179989,0.2102685806102));
#42241=CARTESIAN_POINT('Ctrl Pts',(-7.050243445008,-1.840261017337,-2.361418873952));
#42242=CARTESIAN_POINT('Ctrl Pts',(-6.968993445008,0.3706726829451,-3.880304137017));
#42243=CARTESIAN_POINT('Ctrl Pts',(-6.914826778341,2.151783524521,-3.740648955836));
#42244=CARTESIAN_POINT('Ctrl Pts',(-6.887743445008,2.922638690214,-3.397442123851));
#42245=CARTESIAN_POINT('Ctrl Pts',(-9.394170442699,-0.6806876086837,2.877584625945));
#42246=CARTESIAN_POINT('Ctrl Pts',(-9.367087109366,-1.333590849641,2.403222654717));
#42247=CARTESIAN_POINT('Ctrl Pts',(-9.312920442699,-2.301009810423,0.9947418214436));
#42248=CARTESIAN_POINT('Ctrl Pts',(-9.231670442699,-2.10023207207,-1.562884793063));
#42249=CARTESIAN_POINT('Ctrl Pts',(-9.150420442699,-0.3343472621158,-3.423508148791));
#42250=CARTESIAN_POINT('Ctrl Pts',(-9.069170442699,2.208854940398,-3.758356902288));
#42251=CARTESIAN_POINT('Ctrl Pts',(-8.987920442699,4.396041844558,-2.418045984201));
#42252=CARTESIAN_POINT('Ctrl Pts',(-8.906670442699,5.252314847485,-3.831845932778E-7));
#42253=CARTESIAN_POINT('Ctrl Pts',(-8.825420442699,4.396040017561,2.418047516939));
#42254=CARTESIAN_POINT('Ctrl Pts',(-8.744170442699,2.208862248383,3.758351537704));
#42255=CARTESIAN_POINT('Ctrl Pts',(-8.662920442699,-0.3343746670588,3.423528074391));
#42256=CARTESIAN_POINT('Ctrl Pts',(-8.581670442699,-2.100129760283,1.562810455248));
#42257=CARTESIAN_POINT('Ctrl Pts',(-8.500420442699,-2.301391652629,-0.9944643957835));
#42258=CARTESIAN_POINT('Ctrl Pts',(-8.419170442699,-0.8484563122144,-3.108498436179));
#42259=CARTESIAN_POINT('Ctrl Pts',(-8.337920442699,1.611091249384,-3.837049615173));
#42260=CARTESIAN_POINT('Ctrl Pts',(-8.256670442699,3.981010816611,-2.855396788715));
#42261=CARTESIAN_POINT('Ctrl Pts',(-8.175420442699,5.205010096676,-0.6010705501845));
#42262=CARTESIAN_POINT('Ctrl Pts',(-8.094170442699,4.737542724007,1.921157687446));
#42263=CARTESIAN_POINT('Ctrl Pts',(-8.012920442699,2.786962682412,3.587110426432));
#42264=CARTESIAN_POINT('Ctrl Pts',(-7.931670442699,0.2226592513938,3.654259074947));
#42265=CARTESIAN_POINT('Ctrl Pts',(-7.850420442699,-1.812436817629,2.092674938032));
#42266=CARTESIAN_POINT('Ctrl Pts',(-7.769170442699,-2.411266769463,-0.4016313216255));
#42267=CARTESIAN_POINT('Ctrl Pts',(-7.687920442699,-1.306927256222,-2.716927256679));
#42268=CARTESIAN_POINT('Ctrl Pts',(-7.606670442699,1.008368675403,-3.821266770609));
#42269=CARTESIAN_POINT('Ctrl Pts',(-7.525420442699,3.502674949463,-3.222436812587));
#42270=CARTESIAN_POINT('Ctrl Pts',(-7.444170442699,5.064259032195,-1.187340767628));
#42271=CARTESIAN_POINT('Ctrl Pts',(-7.362920442699,4.997110586008,1.376962753456));
#42272=CARTESIAN_POINT('Ctrl Pts',(-7.281670442699,3.331157091895,3.327542458853));
#42273=CARTESIAN_POINT('Ctrl Pts',(-7.200420442699,0.8089316724422,3.795011086251));
#42274=CARTESIAN_POINT('Ctrl Pts',(-7.119170442699,-1.445405083671,2.571007123468));
#42275=CARTESIAN_POINT('Ctrl Pts',(-7.037920442699,-2.427018657974,0.2011050323817));
#42276=CARTESIAN_POINT('Ctrl Pts',(-6.956670442699,-1.698613970016,-2.258507751061));
#42277=CARTESIAN_POINT('Ctrl Pts',(-6.875420442699,0.4159667823653,-3.711199680242));
#42278=CARTESIAN_POINT('Ctrl Pts',(-6.821253776032,2.119456445115,-3.577630700739));
#42279=CARTESIAN_POINT('Ctrl Pts',(-6.794170442699,2.856717583266,-3.24938089347));
#42280=CARTESIAN_POINT('',(-6.86905988805729,1.40999999992759,-3.59999993640925));
#42281=CARTESIAN_POINT('Ctrl Pts',(-9.36908159826537,-1.70608638503483,
1.79907071129373));
#42282=CARTESIAN_POINT('Ctrl Pts',(-9.35656564768497,-1.89532982405453,
1.47248218597209));
#42283=CARTESIAN_POINT('Ctrl Pts',(-9.3420183949866,-2.06808132628875,1.06106946402822));
#42284=CARTESIAN_POINT('Ctrl Pts',(-9.30955126796911,-2.2174468266351,0.0942360700323995));
#42285=CARTESIAN_POINT('Ctrl Pts',(-9.29393475271798,-2.19733524992031,
-0.385795687504502));
#42286=CARTESIAN_POINT('Ctrl Pts',(-9.26248954825925,-1.97759186945788,
-1.30821422968742));
#42287=CARTESIAN_POINT('Ctrl Pts',(-9.24704728409788,-1.7777422252897,-1.73815589466842));
#42288=CARTESIAN_POINT('Ctrl Pts',(-9.2159995527642,-1.22380952851887,-2.4931386603676));
#42289=CARTESIAN_POINT('Ctrl Pts',(-9.2007178856219,-0.880327472077824,
-2.81351240010764));
#42290=CARTESIAN_POINT('Ctrl Pts',(-9.16706020219686,-0.0201454942556584,
-3.35073711466933));
#42291=CARTESIAN_POINT('Ctrl Pts',(-9.15140080005762,0.44237879573454,-3.48733627110526));
#42292=CARTESIAN_POINT('Ctrl Pts',(-9.12359464961302,1.27037395437227,-3.62272692428968));
#42293=CARTESIAN_POINT('Ctrl Pts',(-9.10868269931163,1.7279038239651,-3.61408512036349));
#42294=CARTESIAN_POINT('Ctrl Pts',(-9.07793444640764,2.63331213616281,-3.41907230663781));
#42295=CARTESIAN_POINT('Ctrl Pts',(-9.06213235429575,3.07790206736608,-3.22265134720342));
#42296=CARTESIAN_POINT('Ctrl Pts',(-9.03340558182475,3.78929212861789,-2.72756811571599));
#42297=CARTESIAN_POINT('Ctrl Pts',(-9.01810701650085,4.13772490077611,-2.41136229140776));
#42298=CARTESIAN_POINT('Ctrl Pts',(-8.98463857946408,4.6845423916094,-1.56386495711759));
#42299=CARTESIAN_POINT('Ctrl Pts',(-8.96902258646002,4.86168791594835,-1.11730839831426));
#42300=CARTESIAN_POINT('Ctrl Pts',(-8.93757513255501,5.0367005821264,-0.185338695322908));
#42301=CARTESIAN_POINT('Ctrl Pts',(-8.92212964462973,5.02931382570696,0.288815461922182));
#42302=CARTESIAN_POINT('Ctrl Pts',(-8.89107630633225,4.83089760378159,1.20411899127373));
#42303=CARTESIAN_POINT('Ctrl Pts',(-8.87579303405328,4.64768240357197,1.63666659383711));
#42304=CARTESIAN_POINT('Ctrl Pts',(-8.84214219201624,4.08104577128213,2.47750689993866));
#42305=CARTESIAN_POINT('Ctrl Pts',(-8.82648728537404,3.71444438472003,2.79062938894396));
#42306=CARTESIAN_POINT('Ctrl Pts',(-8.79867522834333,3.01325307179544,3.25164727376078));
#42307=CARTESIAN_POINT('Ctrl Pts',(-8.78376661051786,2.59196492057786,3.4300699355234));
#42308=CARTESIAN_POINT('Ctrl Pts',(-8.75302374795712,1.68581697483343,3.62085553562213));
#42309=CARTESIAN_POINT('Ctrl Pts',(-8.73722090140883,1.19975277292987,3.62259872586791));
#42310=CARTESIAN_POINT('Ctrl Pts',(-8.70850151358385,0.348598058934352,
3.46032176848038));
#42311=CARTESIAN_POINT('Ctrl Pts',(-8.69320377234091,-0.0984315066368902,
3.31357798233121));
#42312=CARTESIAN_POINT('Ctrl Pts',(-8.65973338876775,-0.943177717951456,
2.76242525451423));
#42313=CARTESIAN_POINT('Ctrl Pts',(-8.64411533253879,-1.28693865774261,
2.42674063682566));
#42314=CARTESIAN_POINT('Ctrl Pts',(-8.61266882970619,-1.82646306968818,
1.64695414520521));
#42315=CARTESIAN_POINT('Ctrl Pts',(-8.59722630917321,-2.01291298468063,
1.21103527034422));
#42316=CARTESIAN_POINT('Ctrl Pts',(-8.56616958007247,-2.20468934191018,
0.294218193195971));
#42317=CARTESIAN_POINT('Ctrl Pts',(-8.55088334171275,-2.21359613350388,
-0.175543737550325));
#42318=CARTESIAN_POINT('Ctrl Pts',(-8.51723599099668,-2.03870729715697,
-1.17419294066118));
#42319=CARTESIAN_POINT('Ctrl Pts',(-8.50158448221408,-1.83160449981305,
-1.60944010832624));
#42320=CARTESIAN_POINT('Ctrl Pts',(-8.47376671229103,-1.37897885840423,
-2.31628097671549));
#42321=CARTESIAN_POINT('Ctrl Pts',(-8.4588622495886,-1.06701032516302,-2.65076002294469));
#42322=CARTESIAN_POINT('Ctrl Pts',(-8.42812579438174,-0.317446084704319,
-3.19417423343644));
#42323=CARTESIAN_POINT('Ctrl Pts',(-8.41232206896895,0.125743998114912,
-3.39384267259265));
#42324=CARTESIAN_POINT('Ctrl Pts',(-8.38361063283124,0.968921924879503,
-3.59243206163479));
#42325=CARTESIAN_POINT('Ctrl Pts',(-8.36831397111268,1.43691188026915,-3.64066439324238));
#42326=CARTESIAN_POINT('Ctrl Pts',(-8.3348419287405,2.4329921564059,-3.48167859570911));
#42327=CARTESIAN_POINT('Ctrl Pts',(-8.31922153650926,2.88378118790839,-3.31519900874101));
#42328=CARTESIAN_POINT('Ctrl Pts',(-8.2877761342433,3.69423168855654,-2.82298744252997));
#42329=CARTESIAN_POINT('Ctrl Pts',(-8.27233698452426,4.04210919775717,-2.50100896810474));
#42330=CARTESIAN_POINT('Ctrl Pts',(-8.24127638223185,4.59096715371533,-1.74186823207487));
#42331=CARTESIAN_POINT('Ctrl Pts',(-8.22598675889404,4.79058036633025,-1.31641162082661));
#42332=CARTESIAN_POINT('Ctrl Pts',(-8.19234301257582,5.03780997820345,-0.333276150020885));
#42333=CARTESIAN_POINT('Ctrl Pts',(-8.17669533552577,5.02614425340102,0.148461360209209));
#42334=CARTESIAN_POINT('Ctrl Pts',(-8.1488714338802,4.9008256457112,0.97858026135804));
#42335=CARTESIAN_POINT('Ctrl Pts',(-8.13397175644994,4.75227370220379,1.41101213498212));
#42336=CARTESIAN_POINT('Ctrl Pts',(-8.10414802819902,4.3031092050443,2.1889878650182));
#42337=CARTESIAN_POINT('Ctrl Pts',(-8.08924835076851,4.00288818883332,2.53385355868917));
#42338=CARTESIAN_POINT('Ctrl Pts',(-8.0614244491227,3.34664343612139,3.05744210708993));
#42339=CARTESIAN_POINT('Ctrl Pts',(-8.0457767720724,2.93527937670709,3.3084136762376));
#42340=CARTESIAN_POINT('Ctrl Pts',(-8.01213302575411,1.96024427769048,3.58587428719052));
#42341=CARTESIAN_POINT('Ctrl Pts',(-7.99684340241638,1.49198143783378,3.62573247975904));
#42342=CARTESIAN_POINT('Ctrl Pts',(-7.96578280012404,0.560117297405531,
3.52997791484458));
#42343=CARTESIAN_POINT('Ctrl Pts',(-7.95034365040512,0.107337004481917,
3.38969639168411));
#42344=CARTESIAN_POINT('Ctrl Pts',(-7.91889824813912,-0.724155966216583,
2.93393145271846));
#42345=CARTESIAN_POINT('Ctrl Pts',(-7.90327785590776,-1.09372603349349,
2.62677649317387));
#42346=CARTESIAN_POINT('Ctrl Pts',(-7.8698058135354,-1.7294519110665,1.8436385685972));
#42347=CARTESIAN_POINT('Ctrl Pts',(-7.85450915181672,-1.9216764643054,1.41423121270976));
#42348=CARTESIAN_POINT('Ctrl Pts',(-7.82579771567903,-2.17128197185496,
0.584723013699983));
#42349=CARTESIAN_POINT('Ctrl Pts',(-7.80999399026637,-2.21995907262114,
0.101074923695152));
#42350=CARTESIAN_POINT('Ctrl Pts',(-7.77925753505961,-2.12413068178684,
-0.819773855556165));
#42351=CARTESIAN_POINT('Ctrl Pts',(-7.76435307235719,-1.99044759733926,
-1.25718605363892));
#42352=CARTESIAN_POINT('Ctrl Pts',(-7.73653530243412,-1.60461826958533,
-2.00259179169769));
#42353=CARTESIAN_POINT('Ctrl Pts',(-7.72088379365142,-1.33123456413399,
-2.39957165922486));
#42354=CARTESIAN_POINT('Ctrl Pts',(-7.68723644293545,-0.553823402944156,
-3.05035443589483));
#42355=CARTESIAN_POINT('Ctrl Pts',(-7.67195020457591,-0.142544241390169,
-3.27752189348149));
#42356=CARTESIAN_POINT('Ctrl Pts',(-7.64089347547534,0.747330816658283,
-3.56984723484916));
#42357=CARTESIAN_POINT('Ctrl Pts',(-7.62545095494251,1.21807259377298,-3.62633630936248));
#42358=CARTESIAN_POINT('Ctrl Pts',(-7.59400445210985,2.16314971101678,-3.5489877084657));
#42359=CARTESIAN_POINT('Ctrl Pts',(-7.57838639588073,2.62574158749038,-3.41912431062186));
#42360=CARTESIAN_POINT('Ctrl Pts',(-7.54491601230753,3.52542695680217,-2.96312899578098));
#42361=CARTESIAN_POINT('Ctrl Pts',(-7.52961827106464,3.87602558624036,-2.64936192882806));
#42362=CARTESIAN_POINT('Ctrl Pts',(-7.50089888323972,4.44213891078422,-1.99337880265076));
#42363=CARTESIAN_POINT('Ctrl Pts',(-7.48509603669147,4.68366136469929,-1.57156326080923));
#42364=CARTESIAN_POINT('Ctrl Pts',(-7.45435317413076,4.97151016120934,-0.691423320158279));
#42365=CARTESIAN_POINT('Ctrl Pts',(-7.43944455630529,5.0276356791207,-0.237365748009259));
#42366=CARTESIAN_POINT('Ctrl Pts',(-7.41163249927462,4.97897813573245,0.600392684304703));
#42367=CARTESIAN_POINT('Ctrl Pts',(-7.39597759263248,4.89110679903858,1.07444004263272));
#42368=CARTESIAN_POINT('Ctrl Pts',(-7.36232675059545,4.44623604957346,1.98558191396119));
#42369=CARTESIAN_POINT('Ctrl Pts',(-7.34704347831648,4.16324643751228,2.36052473298373));
#42370=CARTESIAN_POINT('Ctrl Pts',(-7.31599014001889,3.46977843988281,2.99000998636961));
#42371=CARTESIAN_POINT('Ctrl Pts',(-7.30054465209352,3.06284227260819,3.23348418370286));
#42372=CARTESIAN_POINT('Ctrl Pts',(-7.2690971981882,2.16822650117104,3.54790362030417));
#42373=CARTESIAN_POINT('Ctrl Pts',(-7.25348120518384,1.69292441485116,3.61776937546153));
#42374=CARTESIAN_POINT('Ctrl Pts',(-7.22001276814687,0.685561448299564,
3.56796020431102));
#42375=CARTESIAN_POINT('Ctrl Pts',(-7.20471420282298,0.237502785544977,
3.42431148426495));
#42376=CARTESIAN_POINT('Ctrl Pts',(-7.17598743035216,-0.546946900536664,
3.05577123496466));
#42377=CARTESIAN_POINT('Ctrl Pts',(-7.16018533824052,-0.939347406844226,
2.76895553999291));
#42378=CARTESIAN_POINT('Ctrl Pts',(-7.12943708533679,-1.56093761369267,
2.08235534769489));
#42379=CARTESIAN_POINT('Ctrl Pts',(-7.11452513503551,-1.79718657022345,
1.69044375960058));
#42380=CARTESIAN_POINT('Ctrl Pts',(-7.08671898459106,-2.09393240444935,
0.905683591417752));
#42381=CARTESIAN_POINT('Ctrl Pts',(-7.07105958245186,-2.20689620983523,
0.436826228201019));
#42382=CARTESIAN_POINT('Ctrl Pts',(-7.03740189902686,-2.17173694839478,
-0.5767255737513));
#42383=CARTESIAN_POINT('Ctrl Pts',(-7.02212023188454,-2.06602617929488,
-1.03437663024341));
#42384=CARTESIAN_POINT('Ctrl Pts',(-6.99107250055076,-1.68915827316509,
-1.89158780048353));
#42385=CARTESIAN_POINT('Ctrl Pts',(-6.97563023638929,-1.41674269123004,
-2.27963350176109));
#42386=CARTESIAN_POINT('Ctrl Pts',(-6.94418503193041,-0.727776491008685,
-2.93114612264658));
#42387=CARTESIAN_POINT('Ctrl Pts',(-6.92856851667922,-0.322112582715683,
-3.18857913776017));
#42388=CARTESIAN_POINT('Ctrl Pts',(-6.89610138755526,0.589872507054565,
-3.54264153998035));
#42389=CARTESIAN_POINT('Ctrl Pts',(-6.8815541332902,1.03254217835801,-3.59874070293085));
#42390=CARTESIAN_POINT('Ctrl Pts',(-6.86903818168747,1.40999788827261,-3.59814532525062));
#42391=CARTESIAN_POINT('',(-7.1,1.41,-4.));
#42392=CARTESIAN_POINT('Ctrl Pts',(-7.174889449625,-0.2344809041097,-3.693564584614));
#42393=CARTESIAN_POINT('Ctrl Pts',(-7.147806116292,0.6035623166656,-4.066685466031));
#42394=CARTESIAN_POINT('Ctrl Pts',(-7.093639449625,2.539915515895,-4.218513050568));
#42395=CARTESIAN_POINT('Ctrl Pts',(-7.012389449625,4.943555111978,-2.567241119733));
#42396=CARTESIAN_POINT('Ctrl Pts',(-6.931139449625,5.771531224017,0.2285956770673));
#42397=CARTESIAN_POINT('Ctrl Pts',(-6.849889449625,4.655733091177,2.922458514209));
#42398=CARTESIAN_POINT('Ctrl Pts',(-6.768639449625,2.093233132829,4.313781303558));
#42399=CARTESIAN_POINT('Ctrl Pts',(-6.687389449625,-0.7737753186654,3.782410675374));
#42400=CARTESIAN_POINT('Ctrl Pts',(-6.606139449625,-2.667461232137,1.5651907324));
#42401=CARTESIAN_POINT('Ctrl Pts',(-6.524889449625,-2.743788732938,-1.349647810754));
#42402=CARTESIAN_POINT('Ctrl Pts',(-6.443639449625,-0.9687393149189,-3.662937303239));
#42403=CARTESIAN_POINT('Ctrl Pts',(-6.362389449625,1.866533501377,-4.343626086017));
#42404=CARTESIAN_POINT('Ctrl Pts',(-6.281139449625,4.498325629267,-3.088325629786));
#42405=CARTESIAN_POINT('Ctrl Pts',(-6.199889449625,5.753626084714,-0.4565334979991));
#42406=CARTESIAN_POINT('Ctrl Pts',(-6.118639449625,5.072937308971,2.378739301925));
#42407=CARTESIAN_POINT('Ctrl Pts',(-6.037389449625,2.759647789132,4.153788781534));
#42408=CARTESIAN_POINT('Ctrl Pts',(-5.956139449625,-0.155190651644,4.077461050748));
#42409=CARTESIAN_POINT('Ctrl Pts',(-5.874889449625,-2.372410976774,2.183775995627));
#42410=CARTESIAN_POINT('Ctrl Pts',(-5.793639449625,-2.903780178711,-0.6832356592843));
#42411=CARTESIAN_POINT('Ctrl Pts',(-5.712389449625,-1.512462712197,-3.245723662317));
#42412=CARTESIAN_POINT('Ctrl Pts',(-5.631139449625,1.181419990037,-4.361566413001));
#42413=CARTESIAN_POINT('Ctrl Pts',(-5.549889449625,3.977182649303,-3.533423784903));
#42414=CARTESIAN_POINT('Ctrl Pts',(-5.468639449625,5.628731265186,-1.130405635211));
#42415=CARTESIAN_POINT('Ctrl Pts',(-5.387389449625,5.39995728572,1.776443433137));
#42416=CARTESIAN_POINT('Ctrl Pts',(-5.306139449625,3.392827099615,3.89151732732));
#42417=CARTESIAN_POINT('Ctrl Pts',(-5.224889449625,0.501934923806,4.272110470055));
#42418=CARTESIAN_POINT('Ctrl Pts',(-5.143639449625,-1.984225552094,2.748589643777));
#42419=CARTESIAN_POINT('Ctrl Pts',(-5.062389449625,-2.957551391752,-4.355651576082E-7));
#42420=CARTESIAN_POINT('Ctrl Pts',(-4.981139449625,-1.984227628837,-2.748587901516));
#42421=CARTESIAN_POINT('Ctrl Pts',(-4.899889449625,0.5019432307773,-4.272116567967));
#42422=CARTESIAN_POINT('Ctrl Pts',(-4.818639449625,3.392795948473,-3.891494677932));
#42423=CARTESIAN_POINT('Ctrl Pts',(-4.737389449625,5.400073583318,-1.776527932779));
#42424=CARTESIAN_POINT('Ctrl Pts',(-4.656139449625,5.628297225935,1.130720984389));
#42425=CARTESIAN_POINT('Ctrl Pts',(-4.601972782958,4.528634081117,2.731738253352));
#42426=CARTESIAN_POINT('Ctrl Pts',(-4.574889449625,3.786480308739,3.270944531304));
#42427=CARTESIAN_POINT('Ctrl Pts',(-7.081316447316,-0.1685597971619,-3.545503354232));
#42428=CARTESIAN_POINT('Ctrl Pts',(-7.054233113983,0.6358893960722,-3.903667210934));
#42429=CARTESIAN_POINT('Ctrl Pts',(-7.000066447316,2.494621416475,-4.049408593792));
#42430=CARTESIAN_POINT('Ctrl Pts',(-6.918816447316,4.801908064657,-2.464329996843));
#42431=CARTESIAN_POINT('Ctrl Pts',(-6.837566447316,5.596693702003,0.2194321288388));
#42432=CARTESIAN_POINT('Ctrl Pts',(-6.756316447316,4.525623755341,2.805308050628));
#42433=CARTESIAN_POINT('Ctrl Pts',(-6.675066447316,2.065844864405,4.140857897789));
#42434=CARTESIAN_POINT('Ctrl Pts',(-6.593816447316,-0.686235909742,3.630787936533));
#42435=CARTESIAN_POINT('Ctrl Pts',(-6.512566447316,-2.504011016761,1.502448072752));
#42436=CARTESIAN_POINT('Ctrl Pts',(-6.431316447316,-2.57727883269,-1.295545463045));
#42437=CARTESIAN_POINT('Ctrl Pts',(-6.350066447316,-0.8733845264335,-3.516103806355));
#42438=CARTESIAN_POINT('Ctrl Pts',(-6.268816447316,1.848232775784,-4.169506314214));
#42439=CARTESIAN_POINT('Ctrl Pts',(-6.187566447316,4.374526171585,-2.964526172083));
#42440=CARTESIAN_POINT('Ctrl Pts',(-6.106316447316,5.579506312963,-0.4382327725412));
#42441=CARTESIAN_POINT('Ctrl Pts',(-6.025066447316,4.926103811857,2.283384513961));
#42442=CARTESIAN_POINT('Ctrl Pts',(-5.943816447316,2.70554544229,3.987278879338));
#42443=CARTESIAN_POINT('Ctrl Pts',(-5.862566447316,-0.09244799523316,3.914010842643));
#42444=CARTESIAN_POINT('Ctrl Pts',(-5.781316447316,-2.220788225852,2.096236559566));
#42445=CARTESIAN_POINT('Ctrl Pts',(-5.700066447316,-2.730856818033,-0.6558472895844));
#42446=CARTESIAN_POINT('Ctrl Pts',(-5.618816447316,-1.395312080335,-3.11561470445));
#42447=CARTESIAN_POINT('Ctrl Pts',(-5.537566447316,1.19058291023,-4.186727480392));
#42448=CARTESIAN_POINT('Ctrl Pts',(-5.456316447316,3.874273870273,-3.391782001995));
#42449=CARTESIAN_POINT('Ctrl Pts',(-5.375066447316,5.459618061001,-1.085091888735));
#42450=CARTESIAN_POINT('Ctrl Pts',(-5.293816447316,5.240014777241,1.705232440507));
#42451=CARTESIAN_POINT('Ctrl Pts',(-5.212566447316,3.31334295543,3.735520909677));
#42452=CARTESIAN_POINT('Ctrl Pts',(-5.131316447316,0.5383358664096,4.100857492604));
#42453=CARTESIAN_POINT('Ctrl Pts',(-5.050066447316,-1.84816370725,2.638408934831));
#42454=CARTESIAN_POINT('Ctrl Pts',(-4.968816447316,-2.782472543663,-4.181049745989E-7));
#42455=CARTESIAN_POINT('Ctrl Pts',(-4.887566447316,-1.848165700744,-2.638407262411));
#42456=CARTESIAN_POINT('Ctrl Pts',(-4.806316447316,0.5383438403855,-4.100863346074));
#42457=CARTESIAN_POINT('Ctrl Pts',(-4.725066447316,3.313313053021,-3.735499168218));
#42458=CARTESIAN_POINT('Ctrl Pts',(-4.643816447316,5.240126412902,-1.705313552873));
#42459=CARTESIAN_POINT('Ctrl Pts',(-4.562566447316,5.459201420765,1.08539459674));
#42460=CARTESIAN_POINT('Ctrl Pts',(-4.50839978065,4.403619670625,2.622233053807));
#42461=CARTESIAN_POINT('Ctrl Pts',(-4.481316447316,3.691216075387,3.139824562851));
#42462=CARTESIAN_POINT('Ctrl Pts',(-6.987743445008,-0.1026386902142,-3.397442123851));
#42463=CARTESIAN_POINT('Ctrl Pts',(-6.960660111674,0.6682164754788,-3.740648955836));
#42464=CARTESIAN_POINT('Ctrl Pts',(-6.906493445008,2.449327317055,-3.880304137017));
#42465=CARTESIAN_POINT('Ctrl Pts',(-6.825243445008,4.660261017337,-2.361418873952));
#42466=CARTESIAN_POINT('Ctrl Pts',(-6.743993445008,5.421856179989,0.2102685806102));
#42467=CARTESIAN_POINT('Ctrl Pts',(-6.662743445008,4.395514419506,2.688157587048));
#42468=CARTESIAN_POINT('Ctrl Pts',(-6.581493445008,2.038456595982,3.96793449202));
#42469=CARTESIAN_POINT('Ctrl Pts',(-6.500243445008,-0.5986965008186,3.479165197693));
#42470=CARTESIAN_POINT('Ctrl Pts',(-6.418993445008,-2.340560801384,1.439705413104));
#42471=CARTESIAN_POINT('Ctrl Pts',(-6.337743445008,-2.410768932443,-1.241443115336));
#42472=CARTESIAN_POINT('Ctrl Pts',(-6.256493445008,-0.7780297379481,-3.369270309471));
#42473=CARTESIAN_POINT('Ctrl Pts',(-6.175243445008,1.829932050191,-3.995386542412));
#42474=CARTESIAN_POINT('Ctrl Pts',(-6.093993445008,4.250726713904,-2.840726714381));
#42475=CARTESIAN_POINT('Ctrl Pts',(-6.012743445008,5.405386541213,-0.4199320470834));
#42476=CARTESIAN_POINT('Ctrl Pts',(-5.931493445008,4.779270314743,2.188029725996));
#42477=CARTESIAN_POINT('Ctrl Pts',(-5.850243445008,2.651443095448,3.820768977142));
#42478=CARTESIAN_POINT('Ctrl Pts',(-5.768993445008,-0.02970533882237,3.750560634537));
#42479=CARTESIAN_POINT('Ctrl Pts',(-5.687743445008,-2.06916547493,2.008697123506));
#42480=CARTESIAN_POINT('Ctrl Pts',(-5.606493445008,-2.557933457354,-0.6284589198844));
#42481=CARTESIAN_POINT('Ctrl Pts',(-5.525243445008,-1.278161448473,-2.985505746582));
#42482=CARTESIAN_POINT('Ctrl Pts',(-5.443993445008,1.199745830423,-4.011888547782));
#42483=CARTESIAN_POINT('Ctrl Pts',(-5.362743445008,3.771365091244,-3.250140219087));
#42484=CARTESIAN_POINT('Ctrl Pts',(-5.281493445008,5.290504856815,-1.039778142259));
#42485=CARTESIAN_POINT('Ctrl Pts',(-5.200243445008,5.080072268762,1.634021447877));
#42486=CARTESIAN_POINT('Ctrl Pts',(-5.118993445008,3.233858811244,3.579524492034));
#42487=CARTESIAN_POINT('Ctrl Pts',(-5.037743445008,0.5747368090133,3.929604515154));
#42488=CARTESIAN_POINT('Ctrl Pts',(-4.956493445008,-1.712101862406,2.528228225885));
#42489=CARTESIAN_POINT('Ctrl Pts',(-4.875243445008,-2.607393695574,-4.00644791597E-7));
#42490=CARTESIAN_POINT('Ctrl Pts',(-4.793993445008,-1.712103772651,-2.528226623306));
#42491=CARTESIAN_POINT('Ctrl Pts',(-4.712743445008,0.5747444499936,-3.929610124181));
#42492=CARTESIAN_POINT('Ctrl Pts',(-4.631493445008,3.233830157568,-3.579503658505));
#42493=CARTESIAN_POINT('Ctrl Pts',(-4.550243445008,5.080179242486,-1.634099172968));
#42494=CARTESIAN_POINT('Ctrl Pts',(-4.468993445008,5.290105615594,1.040068209092));
#42495=CARTESIAN_POINT('Ctrl Pts',(-4.414826778341,4.278605260133,2.512727854262));
#42496=CARTESIAN_POINT('Ctrl Pts',(-4.387743445008,3.595951842036,3.008704594398));
#42497=CARTESIAN_POINT('Ctrl Pts',(-6.894170442699,-0.03671758326641,-3.24938089347));
#42498=CARTESIAN_POINT('Ctrl Pts',(-6.867087109366,0.7005435548854,-3.577630700739));
#42499=CARTESIAN_POINT('Ctrl Pts',(-6.812920442699,2.404033217635,-3.711199680242));
#42500=CARTESIAN_POINT('Ctrl Pts',(-6.731670442699,4.518613970016,-2.258507751061));
#42501=CARTESIAN_POINT('Ctrl Pts',(-6.650420442699,5.247018657974,0.2011050323816));
#42502=CARTESIAN_POINT('Ctrl Pts',(-6.569170442699,4.265405083671,2.571007123468));
#42503=CARTESIAN_POINT('Ctrl Pts',(-6.487920442699,2.011068327558,3.795011086251));
#42504=CARTESIAN_POINT('Ctrl Pts',(-6.406670442699,-0.5111570918951,3.327542458853));
#42505=CARTESIAN_POINT('Ctrl Pts',(-6.325420442699,-2.177110586008,1.376962753456));
#42506=CARTESIAN_POINT('Ctrl Pts',(-6.244170442699,-2.244259032195,-1.187340767628));
#42507=CARTESIAN_POINT('Ctrl Pts',(-6.162920442699,-0.6826749494628,-3.222436812587));
#42508=CARTESIAN_POINT('Ctrl Pts',(-6.081670442699,1.811631324597,-3.821266770609));
#42509=CARTESIAN_POINT('Ctrl Pts',(-6.000420442699,4.126927256222,-2.716927256679));
#42510=CARTESIAN_POINT('Ctrl Pts',(-5.919170442699,5.231266769463,-0.4016313216255));
#42511=CARTESIAN_POINT('Ctrl Pts',(-5.837920442699,4.632436817629,2.092674938032));
#42512=CARTESIAN_POINT('Ctrl Pts',(-5.756670442699,2.597340748606,3.654259074947));
#42513=CARTESIAN_POINT('Ctrl Pts',(-5.675420442699,0.03303731758842,3.587110426432));
#42514=CARTESIAN_POINT('Ctrl Pts',(-5.594170442699,-1.917542724007,1.921157687446));
#42515=CARTESIAN_POINT('Ctrl Pts',(-5.512920442699,-2.385010096676,-0.6010705501845));
#42516=CARTESIAN_POINT('Ctrl Pts',(-5.431670442699,-1.161010816611,-2.855396788715));
#42517=CARTESIAN_POINT('Ctrl Pts',(-5.350420442699,1.208908750616,-3.837049615173));
#42518=CARTESIAN_POINT('Ctrl Pts',(-5.269170442699,3.668456312214,-3.108498436179));
#42519=CARTESIAN_POINT('Ctrl Pts',(-5.187920442699,5.121391652629,-0.9944643957835));
#42520=CARTESIAN_POINT('Ctrl Pts',(-5.106670442699,4.920129760283,1.562810455248));
#42521=CARTESIAN_POINT('Ctrl Pts',(-5.025420442699,3.154374667059,3.423528074391));
#42522=CARTESIAN_POINT('Ctrl Pts',(-4.944170442699,0.6111377516169,3.758351537704));
#42523=CARTESIAN_POINT('Ctrl Pts',(-4.862920442699,-1.576040017561,2.418047516939));
#42524=CARTESIAN_POINT('Ctrl Pts',(-4.781670442699,-2.432314847485,-3.831846085989E-7));
#42525=CARTESIAN_POINT('Ctrl Pts',(-4.700420442699,-1.576041844558,-2.418045984201));
#42526=CARTESIAN_POINT('Ctrl Pts',(-4.619170442699,0.6111450596018,-3.758356902288));
#42527=CARTESIAN_POINT('Ctrl Pts',(-4.537920442699,3.154347262116,-3.423508148791));
#42528=CARTESIAN_POINT('Ctrl Pts',(-4.456670442699,4.92023207207,-1.562884793063));
#42529=CARTESIAN_POINT('Ctrl Pts',(-4.375420442699,5.121009810423,0.9947418214435));
#42530=CARTESIAN_POINT('Ctrl Pts',(-4.321253776032,4.153590849641,2.403222654717));
#42531=CARTESIAN_POINT('Ctrl Pts',(-4.294170442699,3.500687608684,2.877584625945));
#42532=CARTESIAN_POINT('',(-4.36903811233822,4.52608525564794,1.79907266111361));
#42533=CARTESIAN_POINT('Ctrl Pts',(-6.86908159826512,1.41000225333245,-3.59814532547397));
#42534=CARTESIAN_POINT('Ctrl Pts',(-6.85656564768471,1.78745793235516,-3.59874068850376));
#42535=CARTESIAN_POINT('Ctrl Pts',(-6.84201839498573,2.23012755211558,-3.54264151700861));
#42536=CARTESIAN_POINT('Ctrl Pts',(-6.80955126796814,3.14211258271628,-3.1885791377597));
#42537=CARTESIAN_POINT('Ctrl Pts',(-6.79393475271691,3.5477764910093,-2.93114612264598));
#42538=CARTESIAN_POINT('Ctrl Pts',(-6.7624895482582,4.23674269123054,-2.27963350176036));
#42539=CARTESIAN_POINT('Ctrl Pts',(-6.74704728409703,4.50915827316548,-1.89158780048281));
#42540=CARTESIAN_POINT('Ctrl Pts',(-6.71599955276356,4.88602617929508,-1.03437663024274));
#42541=CARTESIAN_POINT('Ctrl Pts',(-6.70071788562139,4.99173694839489,-0.576725573750675));
#42542=CARTESIAN_POINT('Ctrl Pts',(-6.66706020219651,5.02689620983516,0.436826228201624));
#42543=CARTESIAN_POINT('Ctrl Pts',(-6.65140080005729,4.91393240444917,0.90568359141837));
#42544=CARTESIAN_POINT('Ctrl Pts',(-6.62359464961269,4.61718657022314,1.69044375960114));
#42545=CARTESIAN_POINT('Ctrl Pts',(-6.60868269931122,4.38093761369227,2.08235534769542));
#42546=CARTESIAN_POINT('Ctrl Pts',(-6.57793444640711,3.75934740684366,2.76895553999336));
#42547=CARTESIAN_POINT('Ctrl Pts',(-6.56213235429517,3.36694690053603,3.05577123496503));
#42548=CARTESIAN_POINT('Ctrl Pts',(-6.53340558182412,2.58249721445423,3.4243114842652));
#42549=CARTESIAN_POINT('Ctrl Pts',(-6.51810701650023,2.13443855169954,3.56796020431119));
#42550=CARTESIAN_POINT('Ctrl Pts',(-6.48463857946336,1.12707558514785,3.61776937546146));
#42551=CARTESIAN_POINT('Ctrl Pts',(-6.46902258645918,0.651773498827994,
3.54790362030401));
#42552=CARTESIAN_POINT('Ctrl Pts',(-6.43757513255404,-0.24284227260902,
3.23348418370255));
#42553=CARTESIAN_POINT('Ctrl Pts',(-6.42212964462873,-0.649778439883527,
2.99000998636925));
#42554=CARTESIAN_POINT('Ctrl Pts',(-6.39107630633123,-1.3432464375128,2.3605247329833));
#42555=CARTESIAN_POINT('Ctrl Pts',(-6.37579303405225,-1.62623604957389,
1.98558191396071));
#42556=CARTESIAN_POINT('Ctrl Pts',(-6.34214219201528,-2.07110679903882,
1.07444004263209));
#42557=CARTESIAN_POINT('Ctrl Pts',(-6.32648728537324,-2.15897813573259,
0.600392684303986));
#42558=CARTESIAN_POINT('Ctrl Pts',(-6.29867522834268,-2.20763567912064,
-0.237365748009939));
#42559=CARTESIAN_POINT('Ctrl Pts',(-6.28376661051732,-2.15151016120919,
-0.691423320158909));
#42560=CARTESIAN_POINT('Ctrl Pts',(-6.25302374795656,-1.86366136469891,
-1.57156326080986));
#42561=CARTESIAN_POINT('Ctrl Pts',(-6.23722090140809,-1.62213891078368,
-1.99337880265141));
#42562=CARTESIAN_POINT('Ctrl Pts',(-6.20850151358295,-1.05602558623953,
-2.64936192882867));
#42563=CARTESIAN_POINT('Ctrl Pts',(-6.19320377233992,-0.705426956801188,
-2.96312899578155));
#42564=CARTESIAN_POINT('Ctrl Pts',(-6.15973338876674,0.194258412510738,
-3.41912431062218));
#42565=CARTESIAN_POINT('Ctrl Pts',(-6.14411533253787,0.656850288984262,
-3.54898770846589));
#42566=CARTESIAN_POINT('Ctrl Pts',(-6.11266882970534,1.60192740622801,-3.62633630936245));
#42567=CARTESIAN_POINT('Ctrl Pts',(-6.09722630917239,2.07266918334271,-3.56984723484898));
#42568=CARTESIAN_POINT('Ctrl Pts',(-6.06616958007161,2.96254424139103,-3.27752189348108));
#42569=CARTESIAN_POINT('Ctrl Pts',(-6.05088334171184,3.37382340294493,-3.05035443589433));
#42570=CARTESIAN_POINT('Ctrl Pts',(-6.01723599099568,4.1512345641346,-2.39957165922417));
#42571=CARTESIAN_POINT('Ctrl Pts',(-6.00158448221301,4.42461826958585,-2.0025917916969));
#42572=CARTESIAN_POINT('Ctrl Pts',(-5.9737667122899,4.81044759733959,-1.25718605363803));
#42573=CARTESIAN_POINT('Ctrl Pts',(-5.95886224958743,4.94413068178708,-0.819773855555199));
#42574=CARTESIAN_POINT('Ctrl Pts',(-5.92812579438059,5.0399590726211,0.101074923696212));
#42575=CARTESIAN_POINT('Ctrl Pts',(-5.91232206896784,4.99128197185478,0.584723013701021));
#42576=CARTESIAN_POINT('Ctrl Pts',(-5.8836106328302,4.74167646430498,1.41423121271077));
#42577=CARTESIAN_POINT('Ctrl Pts',(-5.86831397111165,4.54945191106594,1.84363856859817));
#42578=CARTESIAN_POINT('Ctrl Pts',(-5.83484192873968,3.91372603349253,2.62677649317481));
#42579=CARTESIAN_POINT('Ctrl Pts',(-5.81922153650868,3.54415596621539,2.93393145271936));
#42580=CARTESIAN_POINT('Ctrl Pts',(-5.78777613424304,2.7126629955164,3.38969639168488));
#42581=CARTESIAN_POINT('Ctrl Pts',(-5.77233698452416,2.25988270259248,3.52997791484526));
#42582=CARTESIAN_POINT('Ctrl Pts',(-5.74127638223186,1.32801856216453,3.62573247975942));
#42583=CARTESIAN_POINT('Ctrl Pts',(-5.72598675889398,0.859755722308294,
3.58587428719093));
#42584=CARTESIAN_POINT('Ctrl Pts',(-5.69234301257561,-0.115279376707324,
3.30841367623825));
#42585=CARTESIAN_POINT('Ctrl Pts',(-5.67669533552535,-0.526643436121224,
3.05744210709078));
#42586=CARTESIAN_POINT('Ctrl Pts',(-5.64887143387965,-1.18288818883317,
2.53385355868996));
#42587=CARTESIAN_POINT('Ctrl Pts',(-5.63397175644942,-1.48310920504433,
2.18898786501864));
#42588=CARTESIAN_POINT('Ctrl Pts',(-5.60414802819858,-1.932273702204,1.41101213498186));
#42589=CARTESIAN_POINT('Ctrl Pts',(-5.58924835076831,-2.08082564571144,
0.978580261357411));
#42590=CARTESIAN_POINT('Ctrl Pts',(-5.56142444912252,-2.20614425340107,
0.148461360208148));
#42591=CARTESIAN_POINT('Ctrl Pts',(-5.5457767720722,-2.21780997820335,-0.333276150021961));
#42592=CARTESIAN_POINT('Ctrl Pts',(-5.51213302575366,-1.97058036632984,
-1.31641162082767));
#42593=CARTESIAN_POINT('Ctrl Pts',(-5.49684340241566,-1.77096715371477,
-1.7418682320759));
#42594=CARTESIAN_POINT('Ctrl Pts',(-5.46578280012323,-1.22210919775633,
-2.50100896810563));
#42595=CARTESIAN_POINT('Ctrl Pts',(-5.45034365040435,-0.874231688555608,
-2.82298744253071));
#42596=CARTESIAN_POINT('Ctrl Pts',(-5.41889824813859,-0.0637811879073202,
-3.31519900874149));
#42597=CARTESIAN_POINT('Ctrl Pts',(-5.4032778559075,0.387007843595256,-3.48167859570946));
#42598=CARTESIAN_POINT('Ctrl Pts',(-5.36980581353536,1.38308811973198,-3.64066439324238));
#42599=CARTESIAN_POINT('Ctrl Pts',(-5.3545091518167,1.85107807512154,-3.59243206163464));
#42600=CARTESIAN_POINT('Ctrl Pts',(-5.3257977156791,2.69425600188595,-3.39384267259226));
#42601=CARTESIAN_POINT('Ctrl Pts',(-5.30999399026649,3.13744608470506,-3.19417423343593));
#42602=CARTESIAN_POINT('Ctrl Pts',(-5.27925753505974,3.88701032516358,-2.65076002294397));
#42603=CARTESIAN_POINT('Ctrl Pts',(-5.26435307235728,4.19897885840477,-2.31628097671465));
#42604=CARTESIAN_POINT('Ctrl Pts',(-5.23653530243416,4.65160449981346,-1.60944010832521));
#42605=CARTESIAN_POINT('Ctrl Pts',(-5.22088379365139,4.85870729715726,-1.17419294066014));
#42606=CARTESIAN_POINT('Ctrl Pts',(-5.18723644293534,5.0335961335039,-0.175543737549326));
#42607=CARTESIAN_POINT('Ctrl Pts',(-5.17195020457575,5.02468934191009,0.29421819319692));
#42608=CARTESIAN_POINT('Ctrl Pts',(-5.14089347547514,4.83291298468031,1.21103527034499));
#42609=CARTESIAN_POINT('Ctrl Pts',(-5.12545095494229,4.64646306968778,1.64695414520581));
#42610=CARTESIAN_POINT('Ctrl Pts',(-5.09400445210965,4.10693865774205,2.42674063682608));
#42611=CARTESIAN_POINT('Ctrl Pts',(-5.07838639588057,3.76317771795078,2.76242525451461));
#42612=CARTESIAN_POINT('Ctrl Pts',(-5.04491601230736,2.91843150663598,3.31357798233151));
#42613=CARTESIAN_POINT('Ctrl Pts',(-5.02961827106443,2.47140194106463,3.46032176848062));
#42614=CARTESIAN_POINT('Ctrl Pts',(-5.0008988832394,1.62024722706905,3.62259872586796));
#42615=CARTESIAN_POINT('Ctrl Pts',(-4.98509603669101,1.13418302516555,3.62085553562207));
#42616=CARTESIAN_POINT('Ctrl Pts',(-4.95435317413029,0.228035079421312,
3.43006993552313));
#42617=CARTESIAN_POINT('Ctrl Pts',(-4.93944455630491,-0.193253071796147,
3.25164727376046));
#42618=CARTESIAN_POINT('Ctrl Pts',(-4.91163249927437,-0.894444384720605,
2.79062938894352));
#42619=CARTESIAN_POINT('Ctrl Pts',(-4.89597759263239,-1.26104577128262,
2.47750689993816));
#42620=CARTESIAN_POINT('Ctrl Pts',(-4.86232675059547,-1.8276824035723,1.63666659383646));
#42621=CARTESIAN_POINT('Ctrl Pts',(-4.84704347831652,-2.01089760378185,
1.20411899127301));
#42622=CARTESIAN_POINT('Ctrl Pts',(-4.81599014001893,-2.20931382570703,
0.288815461921366));
#42623=CARTESIAN_POINT('Ctrl Pts',(-4.80054465209355,-2.21670058212636,
-0.185338695323713));
#42624=CARTESIAN_POINT('Ctrl Pts',(-4.76909719818808,-2.0416879159481,-1.11730839831502));
#42625=CARTESIAN_POINT('Ctrl Pts',(-4.75348120518357,-1.86454239160905,
-1.56386495711833));
#42626=CARTESIAN_POINT('Ctrl Pts',(-4.72001276814644,-1.31772490077557,
-2.41136229140834));
#42627=CARTESIAN_POINT('Ctrl Pts',(-4.70471420282251,-0.969292128617286,
-2.72756811571648));
#42628=CARTESIAN_POINT('Ctrl Pts',(-4.67598743035164,-0.25790206736538,
-3.22265134720376));
#42629=CARTESIAN_POINT('Ctrl Pts',(-4.66018533824,0.186687863837955,-3.41907230663808));
#42630=CARTESIAN_POINT('Ctrl Pts',(-4.6294370853362,1.09209617603565,-3.61408512036354));
#42631=CARTESIAN_POINT('Ctrl Pts',(-4.61452513503486,1.54962604562839,-3.62272692428965));
#42632=CARTESIAN_POINT('Ctrl Pts',(-4.58671898459036,2.37762120426606,-3.48733627110506));
#42633=CARTESIAN_POINT('Ctrl Pts',(-4.57105958245111,2.84014549425619,-3.35073711466903));
#42634=CARTESIAN_POINT('Ctrl Pts',(-4.53740189902619,3.70032747207835,-2.81351240010708));
#42635=CARTESIAN_POINT('Ctrl Pts',(-4.52212023188399,4.04380952851943,-2.49313866036687));
#42636=CARTESIAN_POINT('Ctrl Pts',(-4.49107250055042,4.59774222529018,-1.73815589466743));
#42637=CARTESIAN_POINT('Ctrl Pts',(-4.47563023638915,4.79759186945824,-1.30821422968639));
#42638=CARTESIAN_POINT('Ctrl Pts',(-4.44418503193031,5.01733524992042,-0.38579568750342));
#42639=CARTESIAN_POINT('Ctrl Pts',(-4.42856851667902,5.03744682663507,0.0942360700334575));
#42640=CARTESIAN_POINT('Ctrl Pts',(-4.39610133443088,4.88808107219921,1.06107110873269));
#42641=CARTESIAN_POINT('Ctrl Pts',(-4.38155405604991,4.71532880232278,1.47248441266071));
#42642=CARTESIAN_POINT('Ctrl Pts',(-4.3690381116678,4.52608525532423,1.79907266090034));
#42643=CARTESIAN_POINT('Ctrl Pts',(-4.60069824814697,4.87339643710536,1.99959286527304));
#42644=CARTESIAN_POINT('Ctrl Pts',(-4.56225271749423,4.81575785116069,1.96631521216219));
#42645=CARTESIAN_POINT('Ctrl Pts',(-4.52380718684145,4.75811926521517,1.93303755905287));
#42646=CARTESIAN_POINT('Ctrl Pts',(-4.44658714145964,4.64234887144461,1.86619749104525));
#42647=CARTESIAN_POINT('Ctrl Pts',(-4.40781262673061,4.58421706361958,1.83263507614692));
#42648=CARTESIAN_POINT('Ctrl Pts',(-4.36903811200149,4.5260852557937,1.79907266125016));
#42649=CARTESIAN_POINT('Ctrl Pts',(-4.60038478407041,4.87292780285437,1.99931896219052));
#42650=CARTESIAN_POINT('Ctrl Pts',(-4.6035703024737,4.92593446793067,1.90795956928389));
#42651=CARTESIAN_POINT('Ctrl Pts',(-4.60672386917096,4.97533475390575,1.81450692734378));
#42652=CARTESIAN_POINT('Ctrl Pts',(-4.61408610987978,5.08335468073265,1.58866596006262));
#42653=CARTESIAN_POINT('Ctrl Pts',(-4.61820792381689,5.13828760357301,1.45536284527102));
#42654=CARTESIAN_POINT('Ctrl Pts',(-4.62751113351263,5.24542152639251,1.14850112082971));
#42655=CARTESIAN_POINT('Ctrl Pts',(-4.63270616058839,5.29296121703815,0.974576465761229));
#42656=CARTESIAN_POINT('Ctrl Pts',(-4.6488842581937,5.40000279831522,0.442314977411726));
#42657=CARTESIAN_POINT('Ctrl Pts',(-4.66017405850537,5.4230197842342,0.0773920769223206));
#42658=CARTESIAN_POINT('Ctrl Pts',(-4.67632980023208,5.38624878581296,-0.448695553793838));
#42659=CARTESIAN_POINT('Ctrl Pts',(-4.68135338643631,5.36466139121163,-0.612897342153464));
#42660=CARTESIAN_POINT('Ctrl Pts',(-4.69224737003279,5.29454390370242,-0.972005719990289));
#42661=CARTESIAN_POINT('Ctrl Pts',(-4.69797243738255,5.24147084555266,-1.16480913145431));
#42662=CARTESIAN_POINT('Ctrl Pts',(-4.70781276117758,5.12471824454401,-1.4894595964008));
#42663=CARTESIAN_POINT('Ctrl Pts',(-4.71194275738303,5.06844846719185,-1.62241111450313));
#42664=CARTESIAN_POINT('Ctrl Pts',(-4.72745569362673,4.83664530764845,-2.09553888496919));
#42665=CARTESIAN_POINT('Ctrl Pts',(-4.73934447005763,4.61886330285552,-2.4143241259663));
#42666=CARTESIAN_POINT('Ctrl Pts',(-4.7563410268637,4.24570641361292,-2.82363794847257));
#42667=CARTESIAN_POINT('Ctrl Pts',(-4.76158384758496,4.12177941933755,-2.94337786218929));
#42668=CARTESIAN_POINT('Ctrl Pts',(-4.77264780630134,3.83937965718473,-3.18302488007073));
#42669=CARTESIAN_POINT('Ctrl Pts',(-4.77834885694988,3.67928048231338,-3.29947962163654));
#42670=CARTESIAN_POINT('Ctrl Pts',(-4.78809945679421,3.38876454575258,-3.47877623962825));
#42671=CARTESIAN_POINT('Ctrl Pts',(-4.79217579565211,3.26332005198182,-3.54705929676832));
#42672=CARTESIAN_POINT('Ctrl Pts',(-4.80867299637761,2.75596636334532,-3.78825845997545));
#42673=CARTESIAN_POINT('Ctrl Pts',(-4.82175168624108,2.34935327217074,-3.90791317220951));
#42674=CARTESIAN_POINT('Ctrl Pts',(-4.83955889519952,1.7728527316371,-3.98502389205297));
#42675=CARTESIAN_POINT('Ctrl Pts',(-4.84451582113769,1.60973684337904,-3.99690828055661));
#42676=CARTESIAN_POINT('Ctrl Pts',(-4.85484353222898,1.26258219512494,-4.00083450847173));
#42677=CARTESIAN_POINT('Ctrl Pts',(-4.8601103831318,1.07950933164658,-3.99015666742414));
#42678=CARTESIAN_POINT('Ctrl Pts',(-4.8694309966141,0.755751468539741,-3.94831972406825));
#42679=CARTESIAN_POINT('Ctrl Pts',(-4.87349818263631,0.615624898732014,
-3.92240616106197));
#42680=CARTESIAN_POINT('Ctrl Pts',(-4.88997937013341,0.0701586442008021,
-3.79040136171959));
#42681=CARTESIAN_POINT('Ctrl Pts',(-4.90305151960809,-0.320841553370625,
-3.6274226805427));
#42682=CARTESIAN_POINT('Ctrl Pts',(-4.92084575374689,-0.816921118602842,
-3.32458772652715));
#42683=CARTESIAN_POINT('Ctrl Pts',(-4.92579691850775,-0.950982573522889,
-3.23123973971505));
#42684=CARTESIAN_POINT('Ctrl Pts',(-4.93610604655926,-1.22270830914031,
-3.01614227416233));
#42685=CARTESIAN_POINT('Ctrl Pts',(-4.94136080897506,-1.35793532184405,
-2.89291433481441));
#42686=CARTESIAN_POINT('Ctrl Pts',(-4.95067147605834,-1.58298771247924,
-2.65693772910767));
#42687=CARTESIAN_POINT('Ctrl Pts',(-4.9547406724232,-1.6756334049896,-2.54856669999476));
#42688=CARTESIAN_POINT('Ctrl Pts',(-4.97122336166442,-2.01652107619069,
-2.10267894897076));
#42689=CARTESIAN_POINT('Ctrl Pts',(-4.98429462215974,-2.21783034751745,
-1.72998304527702));
#42690=CARTESIAN_POINT('Ctrl Pts',(-5.00208975083267,-2.41281820332782,
-1.18242790784559));
#42691=CARTESIAN_POINT('Ctrl Pts',(-5.00704233971896,-2.45827713873544,
-1.02547320963265));
#42692=CARTESIAN_POINT('Ctrl Pts',(-5.01735347034643,-2.53410514603836,
-0.687247815140309));
#42693=CARTESIAN_POINT('Ctrl Pts',(-5.02260884847203,-2.56165265704727,
-0.506362404759346));
#42694=CARTESIAN_POINT('Ctrl Pts',(-5.03191996922711,-2.58805099729946,
-0.181331217235873));
#42695=CARTESIAN_POINT('Ctrl Pts',(-5.03598902394775,-2.59185186661705,
-0.0388130227363775));
#42696=CARTESIAN_POINT('Ctrl Pts',(-5.05247169419802,-2.57617378243136,
0.522232472389581));
#42697=CARTESIAN_POINT('Ctrl Pts',(-5.06554311807892,-2.49808026283208,
0.938564511662007));
#42698=CARTESIAN_POINT('Ctrl Pts',(-5.08333835677935,-2.3050325751149,1.48681008555445));
#42699=CARTESIAN_POINT('Ctrl Pts',(-5.08829093116806,-2.2415881606383,1.63739542350894));
#42700=CARTESIAN_POINT('Ctrl Pts',(-5.09860344882482,-2.08764891710839,
1.94800992102914));
#42701=CARTESIAN_POINT('Ctrl Pts',(-5.10386010760204,-1.99519812734779,
2.10596059914832));
#42702=CARTESIAN_POINT('Ctrl Pts',(-5.11317255998373,-1.81113127679454,
2.3752064708769));
#42703=CARTESIAN_POINT('Ctrl Pts',(-5.117241671025,-1.72439197945323,2.48835510650853));
#42704=CARTESIAN_POINT('Ctrl Pts',(-5.13372236742965,-1.35916593970459,
2.91444128970349));
#42705=CARTESIAN_POINT('Ctrl Pts',(-5.14679144608301,-1.03652730430544,
3.18879932984976));
#42706=CARTESIAN_POINT('Ctrl Pts',(-5.16458502497042,-0.541536684159376,
3.49336223301086));
#42707=CARTESIAN_POINT('Ctrl Pts',(-5.16953807765692,-0.39745380021034,
3.57047257538952));
#42708=CARTESIAN_POINT('Ctrl Pts',(-5.17985296404238,-0.0822776288367675,
3.715026423268));
#42709=CARTESIAN_POINT('Ctrl Pts',(-5.18511137697027,0.0890299587085872,
3.7796172228988));
#42710=CARTESIAN_POINT('Ctrl Pts',(-5.1944260539882,0.401595391251225,3.87303712917641));
#42711=CARTESIAN_POINT('Ctrl Pts',(-5.19849564684741,0.540226854777863,
3.90638218415407));
#42712=CARTESIAN_POINT('Ctrl Pts',(-5.21497062076652,1.09200879209013,4.00761093973977));
#42713=CARTESIAN_POINT('Ctrl Pts',(-5.22803248743137,1.51517703941989,4.01779722385531));
#42714=CARTESIAN_POINT('Ctrl Pts',(-5.24582133764916,2.09137133000897,3.94307223682389));
#42715=CARTESIAN_POINT('Ctrl Pts',(-5.25077620067333,2.25192966344508,3.91233032534663));
#42716=CARTESIAN_POINT('Ctrl Pts',(-5.26110079628887,2.58815230117755,3.82627314298496));
#42717=CARTESIAN_POINT('Ctrl Pts',(-5.26636653046677,2.76217799178062,3.76857817963031));
#42718=CARTESIAN_POINT('Ctrl Pts',(-5.2756900115597,3.06414979897996,3.64432388388499));
#42719=CARTESIAN_POINT('Ctrl Pts',(-5.27976113441245,3.19290558586765,3.58295724120763));
#42720=CARTESIAN_POINT('Ctrl Pts',(-5.29621568984227,3.68474781087186,3.31465467918565));
#42721=CARTESIAN_POINT('Ctrl Pts',(-5.30925207780753,4.01942115211145,3.05680262026333));
#42722=CARTESIAN_POINT('Ctrl Pts',(-5.3270240666099,4.41995990930571,2.63671459348876));
#42723=CARTESIAN_POINT('Ctrl Pts',(-5.33198519886083,4.52555986500751,2.51167232241837));
#42724=CARTESIAN_POINT('Ctrl Pts',(-5.34234341881043,4.73343265160419,2.23238333634713));
#42725=CARTESIAN_POINT('Ctrl Pts',(-5.3476344989158,4.83284681560513,2.07726484198014));
#42726=CARTESIAN_POINT('Ctrl Pts',(-5.35698863604942,4.98973040992224,1.78965928054136));
#42727=CARTESIAN_POINT('Ctrl Pts',(-5.36106522943616,5.05118636144953,1.66076044044048));
#42728=CARTESIAN_POINT('Ctrl Pts',(-5.37744732649883,5.2633223778622,1.14499878322517));
#42729=CARTESIAN_POINT('Ctrl Pts',(-5.39039335278322,5.36069205985606,0.73682290711044));
#42730=CARTESIAN_POINT('Ctrl Pts',(-5.40810573856788,5.40831514934431,0.160415114133084));
#42731=CARTESIAN_POINT('Ctrl Pts',(-5.41308938382183,5.41191584677786,-0.00390323901843598));
#42732=CARTESIAN_POINT('Ctrl Pts',(-5.42421436439621,5.3970440644381,-0.37740627340514));
#42733=CARTESIAN_POINT('Ctrl Pts',(-5.43017430376117,5.37219769669584,-0.584878068079895));
#42734=CARTESIAN_POINT('Ctrl Pts',(-5.44059768696027,5.30003297783807,-0.94248047016988));
#42735=CARTESIAN_POINT('Ctrl Pts',(-5.44506936436755,5.2603688794165,-1.09244637138767));
#42736=CARTESIAN_POINT('Ctrl Pts',(-5.4575443025882,5.12911243891207,-1.49191504831283));
#42737=CARTESIAN_POINT('Ctrl Pts',(-5.46568414727179,5.02122485529483,-1.73539122055828));
#42738=CARTESIAN_POINT('Ctrl Pts',(-5.48339908952568,4.73802558627545,-2.23658981625679));
#42739=CARTESIAN_POINT('Ctrl Pts',(-5.49297899782281,4.55410700945141,-2.48980476118052));
#42740=CARTESIAN_POINT('Ctrl Pts',(-5.50643445553346,4.24478756921484,-2.82495907783755));
#42741=CARTESIAN_POINT('Ctrl Pts',(-5.51058694952351,4.14085454108225,-2.9257765305949));
#42742=CARTESIAN_POINT('Ctrl Pts',(-5.52093657132699,3.86715748668139,-3.1633391894806));
#42743=CARTESIAN_POINT('Ctrl Pts',(-5.52715592007245,3.69210444161323,-3.29142779376694));
#42744=CARTESIAN_POINT('Ctrl Pts',(-5.53887399793356,3.35785980814675,-3.49621692938352));
#42745=CARTESIAN_POINT('Ctrl Pts',(-5.5441982500115,3.20308442348093,-3.57763549592054));
#42746=CARTESIAN_POINT('Ctrl Pts',(-5.56135647719954,2.69271752671186,-3.80555207068678));
#42747=CARTESIAN_POINT('Ctrl Pts',(-5.57331646009684,2.31910384288624,-3.91268855134794));
#42748=CARTESIAN_POINT('Ctrl Pts',(-5.58875002182019,1.79863387109188,-3.98302727131656));
#42749=CARTESIAN_POINT('Ctrl Pts',(-5.59275676580047,1.65887923890933,-3.99432367499748));
#42750=CARTESIAN_POINT('Ctrl Pts',(-5.60250657021499,1.31753324769005,-4.00359563815722));
#42751=CARTESIAN_POINT('Ctrl Pts',(-5.60827100141685,1.11713568192516,-3.99361579889223));
#42752=CARTESIAN_POINT('Ctrl Pts',(-5.61936844413469,0.748214458404577,
-3.94700732189921));
#42753=CARTESIAN_POINT('Ctrl Pts',(-5.62456782955319,0.580248495540013,
-3.91474781102115));
#42754=CARTESIAN_POINT('Ctrl Pts',(-5.64202869109998,0.0290543765692642,
-3.77245075419703));
#42755=CARTESIAN_POINT('Ctrl Pts',(-5.65445023878742,-0.342633980042864,
-3.61593464317991));
#42756=CARTESIAN_POINT('Ctrl Pts',(-5.67025629988414,-0.801958619087569,
-3.33505824895108));
#42757=CARTESIAN_POINT('Ctrl Pts',(-5.67423327412791,-0.916739185197197,
-3.25616569249984));
#42758=CARTESIAN_POINT('Ctrl Pts',(-5.68383956709192,-1.18349584160813,
-3.05113704587091));
#42759=CARTESIAN_POINT('Ctrl Pts',(-5.68948992730527,-1.32989561326599,
-2.91994828187451));
#42760=CARTESIAN_POINT('Ctrl Pts',(-5.70043449629585,-1.58417587641841,
-2.65547498388635));
#42761=CARTESIAN_POINT('Ctrl Pts',(-5.70560480027989,-1.69404300947267,
-2.52556125762722));
#42762=CARTESIAN_POINT('Ctrl Pts',(-5.7231383602013,-2.03522283953223,-2.06675560043406));
#42763=CARTESIAN_POINT('Ctrl Pts',(-5.73567052056328,-2.22748273832145,
-1.70825689135514));
#42764=CARTESIAN_POINT('Ctrl Pts',(-5.75156599480494,-2.40844954261256,
-1.19782329208381));
#42765=CARTESIAN_POINT('Ctrl Pts',(-5.75553633797694,-2.44787629006441,
-1.06445733848564));
#42766=CARTESIAN_POINT('Ctrl Pts',(-5.76510922149235,-2.52574739702303,
-0.738350992429132));
#42767=CARTESIAN_POINT('Ctrl Pts',(-5.77073271771454,-2.55679954926609,
-0.545209132280826));
#42768=CARTESIAN_POINT('Ctrl Pts',(-5.78164143197985,-2.58798656491482,
-0.180822322261445));
#42769=CARTESIAN_POINT('Ctrl Pts',(-5.78680500296509,-2.59167201613416,
-0.0109269046440773));
#42770=CARTESIAN_POINT('Ctrl Pts',(-5.8043555217336,-2.5683175062015,0.560935398308547));
#42771=CARTESIAN_POINT('Ctrl Pts',(-5.81691346823071,-2.49203377848039,
0.961348119108141));
#42772=CARTESIAN_POINT('Ctrl Pts',(-5.83282970047609,-2.31113156818679,
1.47258554747236));
#42773=CARTESIAN_POINT('Ctrl Pts',(-5.83679844779872,-2.25784635991363,
1.60099011966924));
#42774=CARTESIAN_POINT('Ctrl Pts',(-5.84636369073377,-2.11322477722094,
1.90317348646012));
#42775=CARTESIAN_POINT('Ctrl Pts',(-5.85198112237257,-2.01591397093011,
2.07262645731367));
#42776=CARTESIAN_POINT('Ctrl Pts',(-5.86288169834542,-1.81100355903198,
2.37523014621238));
#42777=CARTESIAN_POINT('Ctrl Pts',(-5.86804370107018,-1.70698989363315,
2.50955392441075));
#42778=CARTESIAN_POINT('Ctrl Pts',(-5.88559858416176,-1.32890077945757,
2.93942774296589));
#42779=CARTESIAN_POINT('Ctrl Pts',(-5.89816297819076,-1.01748136516023,
3.20274123435002));
#42780=CARTESIAN_POINT('Ctrl Pts',(-5.91408450248805,-0.554989599631195,
3.48627930074549));
#42781=CARTESIAN_POINT('Ctrl Pts',(-5.91805294469507,-0.43277713688448,
3.55252544851183));
#42782=CARTESIAN_POINT('Ctrl Pts',(-5.92761567211628,-0.130291101233887,
3.6963027695397));
#42783=CARTESIAN_POINT('Ctrl Pts',(-5.93323089022474,0.0518993214266012,
3.76672268133318));
#42784=CARTESIAN_POINT('Ctrl Pts',(-5.9441288630142,0.401494391228572,3.87291892401509));
#42785=CARTESIAN_POINT('Ctrl Pts',(-5.94929068481812,0.566854576580979,
3.91185314358545));
#42786=CARTESIAN_POINT('Ctrl Pts',(-5.96684585399282,1.13122133112492,4.0080058126726));
#42787=CARTESIAN_POINT('Ctrl Pts',(-5.97941074223079,1.53896471436482,4.0166650742138));
#42788=CARTESIAN_POINT('Ctrl Pts',(-5.99533278553194,2.07684470530957,3.94596574783833));
#42789=CARTESIAN_POINT('Ctrl Pts',(-5.99930129158615,2.21351485643232,3.92053930061174));
#42790=CARTESIAN_POINT('Ctrl Pts',(-6.00886367698267,2.53906472412968,3.84192106855853));
#42791=CARTESIAN_POINT('Ctrl Pts',(-6.0144784660986,2.72495947040826,3.78199858149246));
#42792=CARTESIAN_POINT('Ctrl Pts',(-6.02537458446193,3.06342520767069,3.64455124343639));
#42793=CARTESIAN_POINT('Ctrl Pts',(-6.03053491878416,3.21639598830336,3.57077129989299));
#42794=CARTESIAN_POINT('Ctrl Pts',(-6.04808979702491,3.71550980607629,3.29036196952939));
#42795=CARTESIAN_POINT('Ctrl Pts',(-6.06065621085059,4.03787773741545,3.04047995927916));
#42796=CARTESIAN_POINT('Ctrl Pts',(-6.076577503432,4.41139051034082,2.64706678040645));
#42797=CARTESIAN_POINT('Ctrl Pts',(-6.08054420752007,4.50156629507322,2.54135041529522));
#42798=CARTESIAN_POINT('Ctrl Pts',(-6.09011473601431,4.70529165940308,2.27515594889692));
#42799=CARTESIAN_POINT('Ctrl Pts',(-6.09573957130656,4.81223518646438,2.11129130400017));
#42800=CARTESIAN_POINT('Ctrl Pts',(-6.10665168319297,4.98896997997358,1.79096739541931));
#42801=CARTESIAN_POINT('Ctrl Pts',(-6.11181736549454,5.06145478402435,1.63718324939772));
#42802=CARTESIAN_POINT('Ctrl Pts',(-6.12938479342604,5.27285389105025,1.10470664553907));
#42803=CARTESIAN_POINT('Ctrl Pts',(-6.14195794858033,5.36602121342009,0.707359995913639));
#42804=CARTESIAN_POINT('Ctrl Pts',(-6.15789451213981,5.40848143073685,0.166017902455362));
#42805=CARTESIAN_POINT('Ctrl Pts',(-6.16186945335005,5.41195385370929,0.026823199581638));
#42806=CARTESIAN_POINT('Ctrl Pts',(-6.17139040514569,5.40256970591803,-0.306399653629353));
#42807=CARTESIAN_POINT('Ctrl Pts',(-6.17695711370529,5.382795545833,-0.498933285560094));
#42808=CARTESIAN_POINT('Ctrl Pts',(-6.18779443377622,5.31932381804776,-0.856657734443659));
#42809=CARTESIAN_POINT('Ctrl Pts',(-6.19294824148474,5.27914226898062,-1.02143551381684));
#42810=CARTESIAN_POINT('Ctrl Pts',(-6.21045140434731,5.10960376729697,-1.56645372157515));
#42811=CARTESIAN_POINT('Ctrl Pts',(-6.22297077464372,4.93337268328259,-1.93258635133501));
#42812=CARTESIAN_POINT('Ctrl Pts',(-6.23883466678608,4.62820099619023,-2.3787079638203));
#42813=CARTESIAN_POINT('Ctrl Pts',(-6.2427868842605,4.54408161512812,-2.48868157881534));
#42814=CARTESIAN_POINT('Ctrl Pts',(-6.25247848709626,4.32366283402261,-2.74731254107122));
#42815=CARTESIAN_POINT('Ctrl Pts',(-6.25823857463207,4.18208549069023,-2.88963895180828));
#42816=CARTESIAN_POINT('Ctrl Pts',(-6.2692813387163,3.90172397801768,-3.13164072520095));
#42817=CARTESIAN_POINT('Ctrl Pts',(-6.2744275556656,3.76670573621986,-3.23398973321062));
#42818=CARTESIAN_POINT('Ctrl Pts',(-6.29060925724983,3.32709283935529,-3.52600566838254));
#42819=CARTESIAN_POINT('Ctrl Pts',(-6.30178238136156,3.00176773346185,-3.68511173604148));
#42820=CARTESIAN_POINT('Ctrl Pts',(-6.31774503108853,2.49257762064374,-3.85413806611805));
#42821=CARTESIAN_POINT('Ctrl Pts',(-6.32284351431939,2.32099062755695,-3.89853576151291));
#42822=CARTESIAN_POINT('Ctrl Pts',(-6.33202810551563,2.00558964524924,-3.95766919450422));
#42823=CARTESIAN_POINT('Ctrl Pts',(-6.33612306616013,1.86369523672523,-3.97632621268576));
#42824=CARTESIAN_POINT('Ctrl Pts',(-6.34339855690956,1.61715754079666,-3.99507587614472));
#42825=CARTESIAN_POINT('Ctrl Pts',(-6.34649196870305,1.51356084580697,-3.99886470380823));
#42826=CARTESIAN_POINT('Ctrl Pts',(-6.34961610278363,1.4099734843268,-3.9986428669731));
#42827=CARTESIAN_POINT('Ctrl Pts',(-6.655829557301,-0.03671758326641,-3.24938089347));
#42828=CARTESIAN_POINT('Ctrl Pts',(-6.628746223968,0.7005435548854,-3.577630700739));
#42829=CARTESIAN_POINT('Ctrl Pts',(-6.574579557301,2.404033217635,-3.711199680242));
#42830=CARTESIAN_POINT('Ctrl Pts',(-6.493329557301,4.518613970016,-2.258507751061));
#42831=CARTESIAN_POINT('Ctrl Pts',(-6.412079557301,5.247018657974,0.2011050323816));
#42832=CARTESIAN_POINT('Ctrl Pts',(-6.330829557301,4.265405083671,2.571007123468));
#42833=CARTESIAN_POINT('Ctrl Pts',(-6.249579557301,2.011068327558,3.795011086251));
#42834=CARTESIAN_POINT('Ctrl Pts',(-6.168329557301,-0.5111570918951,3.327542458853));
#42835=CARTESIAN_POINT('Ctrl Pts',(-6.087079557301,-2.177110586008,1.376962753456));
#42836=CARTESIAN_POINT('Ctrl Pts',(-6.005829557301,-2.244259032195,-1.187340767628));
#42837=CARTESIAN_POINT('Ctrl Pts',(-5.924579557301,-0.6826749494628,-3.222436812587));
#42838=CARTESIAN_POINT('Ctrl Pts',(-5.843329557301,1.811631324597,-3.821266770609));
#42839=CARTESIAN_POINT('Ctrl Pts',(-5.762079557301,4.126927256222,-2.716927256679));
#42840=CARTESIAN_POINT('Ctrl Pts',(-5.680829557301,5.231266769463,-0.4016313216255));
#42841=CARTESIAN_POINT('Ctrl Pts',(-5.599579557301,4.632436817629,2.092674938032));
#42842=CARTESIAN_POINT('Ctrl Pts',(-5.518329557301,2.597340748606,3.654259074947));
#42843=CARTESIAN_POINT('Ctrl Pts',(-5.437079557301,0.03303731758841,3.587110426432));
#42844=CARTESIAN_POINT('Ctrl Pts',(-5.355829557301,-1.917542724007,1.921157687446));
#42845=CARTESIAN_POINT('Ctrl Pts',(-5.274579557301,-2.385010096676,-0.6010705501845));
#42846=CARTESIAN_POINT('Ctrl Pts',(-5.193329557301,-1.161010816611,-2.855396788715));
#42847=CARTESIAN_POINT('Ctrl Pts',(-5.112079557301,1.208908750616,-3.837049615173));
#42848=CARTESIAN_POINT('Ctrl Pts',(-5.030829557301,3.668456312214,-3.108498436179));
#42849=CARTESIAN_POINT('Ctrl Pts',(-4.949579557301,5.121391652629,-0.9944643957835));
#42850=CARTESIAN_POINT('Ctrl Pts',(-4.868329557301,4.920129760283,1.562810455248));
#42851=CARTESIAN_POINT('Ctrl Pts',(-4.787079557301,3.154374667059,3.423528074391));
#42852=CARTESIAN_POINT('Ctrl Pts',(-4.705829557301,0.611137751617,3.758351537704));
#42853=CARTESIAN_POINT('Ctrl Pts',(-4.624579557301,-1.576040017561,2.418047516939));
#42854=CARTESIAN_POINT('Ctrl Pts',(-4.543329557301,-2.432314847485,-3.831846085989E-7));
#42855=CARTESIAN_POINT('Ctrl Pts',(-4.462079557301,-1.576041844558,-2.418045984201));
#42856=CARTESIAN_POINT('Ctrl Pts',(-4.380829557301,0.6111450596018,-3.758356902288));
#42857=CARTESIAN_POINT('Ctrl Pts',(-4.299579557301,3.154347262116,-3.423508148791));
#42858=CARTESIAN_POINT('Ctrl Pts',(-4.218329557301,4.92023207207,-1.562884793063));
#42859=CARTESIAN_POINT('Ctrl Pts',(-4.137079557301,5.121009810423,0.9947418214435));
#42860=CARTESIAN_POINT('Ctrl Pts',(-4.082912890634,4.153590849641,2.403222654717));
#42861=CARTESIAN_POINT('Ctrl Pts',(-4.055829557301,3.500687608684,2.877584625945));
#42862=CARTESIAN_POINT('Ctrl Pts',(-6.562256554992,-0.1026386902142,-3.397442123851));
#42863=CARTESIAN_POINT('Ctrl Pts',(-6.535173221659,0.6682164754788,-3.740648955836));
#42864=CARTESIAN_POINT('Ctrl Pts',(-6.481006554992,2.449327317055,-3.880304137017));
#42865=CARTESIAN_POINT('Ctrl Pts',(-6.399756554992,4.660261017337,-2.361418873952));
#42866=CARTESIAN_POINT('Ctrl Pts',(-6.318506554992,5.421856179989,0.2102685806102));
#42867=CARTESIAN_POINT('Ctrl Pts',(-6.237256554992,4.395514419506,2.688157587048));
#42868=CARTESIAN_POINT('Ctrl Pts',(-6.156006554992,2.038456595982,3.96793449202));
#42869=CARTESIAN_POINT('Ctrl Pts',(-6.074756554992,-0.5986965008186,3.479165197693));
#42870=CARTESIAN_POINT('Ctrl Pts',(-5.993506554992,-2.340560801384,1.439705413104));
#42871=CARTESIAN_POINT('Ctrl Pts',(-5.912256554992,-2.410768932443,-1.241443115336));
#42872=CARTESIAN_POINT('Ctrl Pts',(-5.831006554992,-0.7780297379481,-3.369270309471));
#42873=CARTESIAN_POINT('Ctrl Pts',(-5.749756554992,1.829932050191,-3.995386542412));
#42874=CARTESIAN_POINT('Ctrl Pts',(-5.668506554992,4.250726713904,-2.840726714381));
#42875=CARTESIAN_POINT('Ctrl Pts',(-5.587256554992,5.405386541213,-0.4199320470834));
#42876=CARTESIAN_POINT('Ctrl Pts',(-5.506006554992,4.779270314743,2.188029725996));
#42877=CARTESIAN_POINT('Ctrl Pts',(-5.424756554992,2.651443095448,3.820768977142));
#42878=CARTESIAN_POINT('Ctrl Pts',(-5.343506554992,-0.02970533882238,3.750560634537));
#42879=CARTESIAN_POINT('Ctrl Pts',(-5.262256554992,-2.06916547493,2.008697123506));
#42880=CARTESIAN_POINT('Ctrl Pts',(-5.181006554992,-2.557933457354,-0.6284589198844));
#42881=CARTESIAN_POINT('Ctrl Pts',(-5.099756554992,-1.278161448473,-2.985505746582));
#42882=CARTESIAN_POINT('Ctrl Pts',(-5.018506554992,1.199745830423,-4.011888547782));
#42883=CARTESIAN_POINT('Ctrl Pts',(-4.937256554992,3.771365091244,-3.250140219087));
#42884=CARTESIAN_POINT('Ctrl Pts',(-4.856006554992,5.290504856815,-1.039778142259));
#42885=CARTESIAN_POINT('Ctrl Pts',(-4.774756554992,5.080072268762,1.634021447877));
#42886=CARTESIAN_POINT('Ctrl Pts',(-4.693506554992,3.233858811244,3.579524492034));
#42887=CARTESIAN_POINT('Ctrl Pts',(-4.612256554992,0.5747368090133,3.929604515154));
#42888=CARTESIAN_POINT('Ctrl Pts',(-4.531006554992,-1.712101862406,2.528228225885));
#42889=CARTESIAN_POINT('Ctrl Pts',(-4.449756554992,-2.607393695574,-4.006447915689E-7));
#42890=CARTESIAN_POINT('Ctrl Pts',(-4.368506554992,-1.712103772651,-2.528226623306));
#42891=CARTESIAN_POINT('Ctrl Pts',(-4.287256554992,0.5747444499936,-3.929610124181));
#42892=CARTESIAN_POINT('Ctrl Pts',(-4.206006554992,3.233830157568,-3.579503658505));
#42893=CARTESIAN_POINT('Ctrl Pts',(-4.124756554992,5.080179242486,-1.634099172968));
#42894=CARTESIAN_POINT('Ctrl Pts',(-4.043506554992,5.290105615594,1.040068209092));
#42895=CARTESIAN_POINT('Ctrl Pts',(-3.989339888326,4.278605260133,2.512727854262));
#42896=CARTESIAN_POINT('Ctrl Pts',(-3.962256554992,3.595951842036,3.008704594398));
#42897=CARTESIAN_POINT('Ctrl Pts',(-6.468683552684,-0.1685597971619,-3.545503354232));
#42898=CARTESIAN_POINT('Ctrl Pts',(-6.44160021935,0.6358893960722,-3.903667210934));
#42899=CARTESIAN_POINT('Ctrl Pts',(-6.387433552684,2.494621416475,-4.049408593792));
#42900=CARTESIAN_POINT('Ctrl Pts',(-6.306183552684,4.801908064657,-2.464329996843));
#42901=CARTESIAN_POINT('Ctrl Pts',(-6.224933552684,5.596693702003,0.2194321288388));
#42902=CARTESIAN_POINT('Ctrl Pts',(-6.143683552684,4.525623755341,2.805308050628));
#42903=CARTESIAN_POINT('Ctrl Pts',(-6.062433552684,2.065844864405,4.140857897789));
#42904=CARTESIAN_POINT('Ctrl Pts',(-5.981183552684,-0.686235909742,3.630787936533));
#42905=CARTESIAN_POINT('Ctrl Pts',(-5.899933552684,-2.504011016761,1.502448072752));
#42906=CARTESIAN_POINT('Ctrl Pts',(-5.818683552684,-2.57727883269,-1.295545463045));
#42907=CARTESIAN_POINT('Ctrl Pts',(-5.737433552684,-0.8733845264335,-3.516103806355));
#42908=CARTESIAN_POINT('Ctrl Pts',(-5.656183552684,1.848232775784,-4.169506314214));
#42909=CARTESIAN_POINT('Ctrl Pts',(-5.574933552684,4.374526171585,-2.964526172083));
#42910=CARTESIAN_POINT('Ctrl Pts',(-5.493683552684,5.579506312963,-0.4382327725412));
#42911=CARTESIAN_POINT('Ctrl Pts',(-5.412433552684,4.926103811857,2.283384513961));
#42912=CARTESIAN_POINT('Ctrl Pts',(-5.331183552684,2.70554544229,3.987278879338));
#42913=CARTESIAN_POINT('Ctrl Pts',(-5.249933552684,-0.09244799523316,3.914010842643));
#42914=CARTESIAN_POINT('Ctrl Pts',(-5.168683552684,-2.220788225852,2.096236559566));
#42915=CARTESIAN_POINT('Ctrl Pts',(-5.087433552684,-2.730856818033,-0.6558472895844));
#42916=CARTESIAN_POINT('Ctrl Pts',(-5.006183552684,-1.395312080335,-3.11561470445));
#42917=CARTESIAN_POINT('Ctrl Pts',(-4.924933552684,1.19058291023,-4.186727480392));
#42918=CARTESIAN_POINT('Ctrl Pts',(-4.843683552684,3.874273870273,-3.391782001995));
#42919=CARTESIAN_POINT('Ctrl Pts',(-4.762433552684,5.459618061001,-1.085091888735));
#42920=CARTESIAN_POINT('Ctrl Pts',(-4.681183552684,5.240014777241,1.705232440507));
#42921=CARTESIAN_POINT('Ctrl Pts',(-4.599933552684,3.31334295543,3.735520909677));
#42922=CARTESIAN_POINT('Ctrl Pts',(-4.518683552684,0.5383358664096,4.100857492604));
#42923=CARTESIAN_POINT('Ctrl Pts',(-4.437433552684,-1.84816370725,2.638408934831));
#42924=CARTESIAN_POINT('Ctrl Pts',(-4.356183552684,-2.782472543663,-4.181049747422E-7));
#42925=CARTESIAN_POINT('Ctrl Pts',(-4.274933552684,-1.848165700744,-2.638407262411));
#42926=CARTESIAN_POINT('Ctrl Pts',(-4.193683552684,0.5383438403855,-4.100863346074));
#42927=CARTESIAN_POINT('Ctrl Pts',(-4.112433552684,3.313313053021,-3.735499168218));
#42928=CARTESIAN_POINT('Ctrl Pts',(-4.031183552684,5.240126412902,-1.705313552873));
#42929=CARTESIAN_POINT('Ctrl Pts',(-3.949933552684,5.459201420765,1.08539459674));
#42930=CARTESIAN_POINT('Ctrl Pts',(-3.895766886017,4.403619670625,2.622233053807));
#42931=CARTESIAN_POINT('Ctrl Pts',(-3.868683552684,3.691216075387,3.139824562851));
#42932=CARTESIAN_POINT('Ctrl Pts',(-6.375110550375,-0.2344809041097,-3.693564584614));
#42933=CARTESIAN_POINT('Ctrl Pts',(-6.348027217042,0.6035623166656,-4.066685466031));
#42934=CARTESIAN_POINT('Ctrl Pts',(-6.293860550375,2.539915515895,-4.218513050568));
#42935=CARTESIAN_POINT('Ctrl Pts',(-6.212610550375,4.943555111978,-2.567241119733));
#42936=CARTESIAN_POINT('Ctrl Pts',(-6.131360550375,5.771531224017,0.2285956770673));
#42937=CARTESIAN_POINT('Ctrl Pts',(-6.050110550375,4.655733091177,2.922458514209));
#42938=CARTESIAN_POINT('Ctrl Pts',(-5.968860550375,2.093233132829,4.313781303558));
#42939=CARTESIAN_POINT('Ctrl Pts',(-5.887610550375,-0.7737753186654,3.782410675374));
#42940=CARTESIAN_POINT('Ctrl Pts',(-5.806360550375,-2.667461232137,1.5651907324));
#42941=CARTESIAN_POINT('Ctrl Pts',(-5.725110550375,-2.743788732938,-1.349647810754));
#42942=CARTESIAN_POINT('Ctrl Pts',(-5.643860550375,-0.9687393149189,-3.662937303239));
#42943=CARTESIAN_POINT('Ctrl Pts',(-5.562610550375,1.866533501377,-4.343626086017));
#42944=CARTESIAN_POINT('Ctrl Pts',(-5.481360550375,4.498325629267,-3.088325629786));
#42945=CARTESIAN_POINT('Ctrl Pts',(-5.400110550375,5.753626084714,-0.4565334979991));
#42946=CARTESIAN_POINT('Ctrl Pts',(-5.318860550375,5.072937308971,2.378739301925));
#42947=CARTESIAN_POINT('Ctrl Pts',(-5.237610550375,2.759647789132,4.153788781534));
#42948=CARTESIAN_POINT('Ctrl Pts',(-5.156360550375,-0.155190651644,4.077461050748));
#42949=CARTESIAN_POINT('Ctrl Pts',(-5.075110550375,-2.372410976774,2.183775995627));
#42950=CARTESIAN_POINT('Ctrl Pts',(-4.993860550375,-2.903780178711,-0.6832356592843));
#42951=CARTESIAN_POINT('Ctrl Pts',(-4.912610550375,-1.512462712197,-3.245723662317));
#42952=CARTESIAN_POINT('Ctrl Pts',(-4.831360550375,1.181419990037,-4.361566413001));
#42953=CARTESIAN_POINT('Ctrl Pts',(-4.750110550375,3.977182649303,-3.533423784903));
#42954=CARTESIAN_POINT('Ctrl Pts',(-4.668860550375,5.628731265186,-1.130405635211));
#42955=CARTESIAN_POINT('Ctrl Pts',(-4.587610550375,5.39995728572,1.776443433137));
#42956=CARTESIAN_POINT('Ctrl Pts',(-4.506360550375,3.392827099615,3.89151732732));
#42957=CARTESIAN_POINT('Ctrl Pts',(-4.425110550375,0.501934923806,4.272110470055));
#42958=CARTESIAN_POINT('Ctrl Pts',(-4.343860550375,-1.984225552094,2.748589643777));
#42959=CARTESIAN_POINT('Ctrl Pts',(-4.262610550375,-2.957551391752,-4.355651578303E-7));
#42960=CARTESIAN_POINT('Ctrl Pts',(-4.181360550375,-1.984227628837,-2.748587901516));
#42961=CARTESIAN_POINT('Ctrl Pts',(-4.100110550375,0.5019432307773,-4.272116567967));
#42962=CARTESIAN_POINT('Ctrl Pts',(-4.018860550375,3.392795948473,-3.891494677932));
#42963=CARTESIAN_POINT('Ctrl Pts',(-3.937610550375,5.400073583318,-1.776527932779));
#42964=CARTESIAN_POINT('Ctrl Pts',(-3.856360550375,5.628297225935,1.130720984389));
#42965=CARTESIAN_POINT('Ctrl Pts',(-3.802193883708,4.528634081117,2.731738253352));
#42966=CARTESIAN_POINT('Ctrl Pts',(-3.775110550375,3.786480308739,3.270944531304));
#42967=CARTESIAN_POINT('',(-4.08091832637295,4.52608525559028,1.79907266118024));
#42968=CARTESIAN_POINT('Ctrl Pts',(-4.0809183266954,4.52608525577217,1.79907266123773));
#42969=CARTESIAN_POINT('Ctrl Pts',(-4.04214744347317,4.58421161914435,1.83263193277767));
#42970=CARTESIAN_POINT('Ctrl Pts',(-4.00337656025091,4.64233798251616,1.86619120431821));
#42971=CARTESIAN_POINT('Ctrl Pts',(-3.92599972798394,4.75834343545228,1.93316698379834));
#42972=CARTESIAN_POINT('Ctrl Pts',(-3.88739377893924,4.81622252501658,1.96658349173795));
#42973=CARTESIAN_POINT('Ctrl Pts',(-3.84878782989446,4.8741016145805,1.99999999967813));
#42974=CARTESIAN_POINT('Ctrl Pts',(-6.58096181831254,1.41000211172738,-3.59814532525062));
#42975=CARTESIAN_POINT('Ctrl Pts',(-6.56844586670982,1.78745782164221,-3.59874070293084));
#42976=CARTESIAN_POINT('Ctrl Pts',(-6.55389861244537,2.23012749294581,-3.54264153998024));
#42977=CARTESIAN_POINT('Ctrl Pts',(-6.52143148332145,3.14211258271626,-3.18857913775972));
#42978=CARTESIAN_POINT('Ctrl Pts',(-6.50581496807022,3.54777649100928,-2.93114612264599));
#42979=CARTESIAN_POINT('Ctrl Pts',(-6.47436976361129,4.23674269123053,-2.27963350176037));
#42980=CARTESIAN_POINT('Ctrl Pts',(-6.45892749944977,4.50915827316548,-1.89158780048282));
#42981=CARTESIAN_POINT('Ctrl Pts',(-6.42787976811596,4.88602617929508,-1.03437663024274));
#42982=CARTESIAN_POINT('Ctrl Pts',(-6.41259810097365,4.99173694839489,-0.576725573750677));
#42983=CARTESIAN_POINT('Ctrl Pts',(-6.37894041754866,5.02689620983516,0.436826228201623));
#42984=CARTESIAN_POINT('Ctrl Pts',(-6.36328101540946,4.91393240444917,0.905683591418369));
#42985=CARTESIAN_POINT('Ctrl Pts',(-6.33547486496501,4.61718657022314,1.69044375960113));
#42986=CARTESIAN_POINT('Ctrl Pts',(-6.32056291466375,4.38093761369228,2.08235534769541));
#42987=CARTESIAN_POINT('Ctrl Pts',(-6.28981466176003,3.75934740684368,2.76895553999334));
#42988=CARTESIAN_POINT('Ctrl Pts',(-6.27401256964841,3.36694690053605,3.05577123496502));
#42989=CARTESIAN_POINT('Ctrl Pts',(-6.24528579717759,2.58249721445425,3.4243114842652));
#42990=CARTESIAN_POINT('Ctrl Pts',(-6.22998723185367,2.13443855169956,3.56796020431119));
#42991=CARTESIAN_POINT('Ctrl Pts',(-6.19651879481664,1.12707558514787,3.61776937546146));
#42992=CARTESIAN_POINT('Ctrl Pts',(-6.18090280181225,0.651773498828013,
3.54790362030401));
#42993=CARTESIAN_POINT('Ctrl Pts',(-6.1494553479069,-0.242842272609004,
3.23348418370255));
#42994=CARTESIAN_POINT('Ctrl Pts',(-6.13400985998153,-0.649778439883511,
2.99000998636926));
#42995=CARTESIAN_POINT('Ctrl Pts',(-6.10295652168396,-1.34324643751278,
2.36052473298331));
#42996=CARTESIAN_POINT('Ctrl Pts',(-6.08767324940502,-1.62623604957388,
1.98558191396073));
#42997=CARTESIAN_POINT('Ctrl Pts',(-6.05402240736802,-2.07110679903882,
1.0744400426321));
#42998=CARTESIAN_POINT('Ctrl Pts',(-6.03836750072588,-2.15897813573258,
0.600392684303999));
#42999=CARTESIAN_POINT('Ctrl Pts',(-6.01055544369523,-2.20763567912064,
-0.237365748009926));
#43000=CARTESIAN_POINT('Ctrl Pts',(-5.99564682586976,-2.1515101612092,-0.691423320158894));
#43001=CARTESIAN_POINT('Ctrl Pts',(-5.96490396330907,-1.86366136469892,
-1.57156326080984));
#43002=CARTESIAN_POINT('Ctrl Pts',(-5.94910111676084,-1.62213891078369,
-1.99337880265138));
#43003=CARTESIAN_POINT('Ctrl Pts',(-5.92038172893592,-1.05602558623955,
-2.64936192882865));
#43004=CARTESIAN_POINT('Ctrl Pts',(-5.90508398769301,-0.705426956801211,
-2.96312899578154));
#43005=CARTESIAN_POINT('Ctrl Pts',(-5.87161360411978,0.194258412510714,
-3.41912431062218));
#43006=CARTESIAN_POINT('Ctrl Pts',(-5.85599554789065,0.656850288984242,
-3.54898770846588));
#43007=CARTESIAN_POINT('Ctrl Pts',(-5.82454904505799,1.60192740622799,-3.62633630936245));
#43008=CARTESIAN_POINT('Ctrl Pts',(-5.80910652452517,2.07266918334268,-3.56984723484898));
#43009=CARTESIAN_POINT('Ctrl Pts',(-5.77804979542462,2.962544241391,-3.2775218934811));
#43010=CARTESIAN_POINT('Ctrl Pts',(-5.76276355706507,3.3738234029449,-3.05035443589435));
#43011=CARTESIAN_POINT('Ctrl Pts',(-5.7291162063491,4.15123456413457,-2.3995716592242));
#43012=CARTESIAN_POINT('Ctrl Pts',(-5.71346469756639,4.42461826958582,-2.00259179169693));
#43013=CARTESIAN_POINT('Ctrl Pts',(-5.68564692764332,4.81044759733957,-1.25718605363807));
#43014=CARTESIAN_POINT('Ctrl Pts',(-5.6707424649409,4.94413068178707,-0.819773855555241));
#43015=CARTESIAN_POINT('Ctrl Pts',(-5.64000600973413,5.0399590726211,0.101074923696168));
#43016=CARTESIAN_POINT('Ctrl Pts',(-5.62420228432147,4.99128197185479,0.584723013700979));
#43017=CARTESIAN_POINT('Ctrl Pts',(-5.59549084818378,4.74167646430499,1.41423121271074));
#43018=CARTESIAN_POINT('Ctrl Pts',(-5.58019418646508,4.54945191106595,1.84363856859814));
#43019=CARTESIAN_POINT('Ctrl Pts',(-5.5467221440927,3.91372603349255,2.6267764931748));
#43020=CARTESIAN_POINT('Ctrl Pts',(-5.53110175186135,3.5441559662154,2.93393145271935));
#43021=CARTESIAN_POINT('Ctrl Pts',(-5.49965634959531,2.71266299551641,3.38969639168488));
#43022=CARTESIAN_POINT('Ctrl Pts',(-5.4842171998763,2.25988270259248,3.52997791484526));
#43023=CARTESIAN_POINT('Ctrl Pts',(-5.45315659758382,1.32801856216453,3.62573247975942));
#43024=CARTESIAN_POINT('Ctrl Pts',(-5.43786697424592,0.859755722308295,
3.58587428719093));
#43025=CARTESIAN_POINT('Ctrl Pts',(-5.40422322792756,-0.115279376707325,
3.30841367623825));
#43026=CARTESIAN_POINT('Ctrl Pts',(-5.38857555087741,-0.526643436121224,
3.05744210709078));
#43027=CARTESIAN_POINT('Ctrl Pts',(-5.36075164923175,-1.18288818883317,
2.53385355868996));
#43028=CARTESIAN_POINT('Ctrl Pts',(-5.34585197180141,-1.48310920504433,
2.18898786501864));
#43029=CARTESIAN_POINT('Ctrl Pts',(-5.31602824355059,-1.932273702204,1.41101213498186));
#43030=CARTESIAN_POINT('Ctrl Pts',(-5.30112856612032,-2.08082564571144,
0.978580261357411));
#43031=CARTESIAN_POINT('Ctrl Pts',(-5.27330466447475,-2.20614425340107,
0.148461360208153));
#43032=CARTESIAN_POINT('Ctrl Pts',(-5.25765698742468,-2.21780997820335,
-0.33327615002195));
#43033=CARTESIAN_POINT('Ctrl Pts',(-5.22401324110646,-1.97058036632985,
-1.31641162082765));
#43034=CARTESIAN_POINT('Ctrl Pts',(-5.20872361776865,-1.77096715371478,
-1.74186823207588));
#43035=CARTESIAN_POINT('Ctrl Pts',(-5.17766301547623,-1.22210919775635,
-2.5010089681056));
#43036=CARTESIAN_POINT('Ctrl Pts',(-5.16222386575719,-0.874231688555634,
-2.82298744253069));
#43037=CARTESIAN_POINT('Ctrl Pts',(-5.13077846349123,-0.0637811879073495,
-3.31519900874147));
#43038=CARTESIAN_POINT('Ctrl Pts',(-5.11515807126,0.387007843595224,-3.48167859570945));
#43039=CARTESIAN_POINT('Ctrl Pts',(-5.08168602888781,1.38308811973195,-3.64066439324238));
#43040=CARTESIAN_POINT('Ctrl Pts',(-5.06638936716926,1.85107807512151,-3.59243206163465));
#43041=CARTESIAN_POINT('Ctrl Pts',(-5.03767793103155,2.69425600188593,-3.39384267259227));
#43042=CARTESIAN_POINT('Ctrl Pts',(-5.02187420561876,3.13744608470504,-3.19417423343594));
#43043=CARTESIAN_POINT('Ctrl Pts',(-4.9911377504119,3.88701032516357,-2.65076002294398));
#43044=CARTESIAN_POINT('Ctrl Pts',(-4.97623328770948,4.19897885840476,-2.31628097671466));
#43045=CARTESIAN_POINT('Ctrl Pts',(-4.94841551778642,4.65160449981345,-1.60944010832522));
#43046=CARTESIAN_POINT('Ctrl Pts',(-4.93276400900382,4.85870729715726,-1.17419294066014));
#43047=CARTESIAN_POINT('Ctrl Pts',(-4.89911665828775,5.0335961335039,-0.175543737549332));
#43048=CARTESIAN_POINT('Ctrl Pts',(-4.88383041992803,5.02468934191009,0.294218193196915));
#43049=CARTESIAN_POINT('Ctrl Pts',(-4.85277369082731,4.83291298468031,1.21103527034498));
#43050=CARTESIAN_POINT('Ctrl Pts',(-4.83733117029437,4.64646306968778,1.6469541452058));
#43051=CARTESIAN_POINT('Ctrl Pts',(-4.80588466746181,4.10693865774205,2.42674063682608));
#43052=CARTESIAN_POINT('Ctrl Pts',(-4.79026661123289,3.76317771795078,2.7624252545146));
#43053=CARTESIAN_POINT('Ctrl Pts',(-4.7567962276597,2.91843150663598,3.3135779823315));
#43054=CARTESIAN_POINT('Ctrl Pts',(-4.74149848641669,2.47140194106464,3.46032176848061));
#43055=CARTESIAN_POINT('Ctrl Pts',(-4.71277909859167,1.62024722706906,3.62259872586796));
#43056=CARTESIAN_POINT('Ctrl Pts',(-4.69697625204335,1.13418302516555,3.62085553562207));
#43057=CARTESIAN_POINT('Ctrl Pts',(-4.6662333894826,0.228035079421316,3.43006993552313));
#43058=CARTESIAN_POINT('Ctrl Pts',(-4.65132477165713,-0.193253071796144,
3.25164727376046));
#43059=CARTESIAN_POINT('Ctrl Pts',(-4.62351271462644,-0.8944443847206,2.79062938894352));
#43060=CARTESIAN_POINT('Ctrl Pts',(-4.60785780798426,-1.26104577128261,
2.47750689993816));
#43061=CARTESIAN_POINT('Ctrl Pts',(-4.57420696594723,-1.8276824035723,1.63666659383647));
#43062=CARTESIAN_POINT('Ctrl Pts',(-4.55892369366826,-2.01089760378185,
1.20411899127301));
#43063=CARTESIAN_POINT('Ctrl Pts',(-4.52787035537078,-2.20931382570703,
0.288815461921373));
#43064=CARTESIAN_POINT('Ctrl Pts',(-4.51242486744549,-2.21670058212636,
-0.185338695323704));
#43065=CARTESIAN_POINT('Ctrl Pts',(-4.48097741354048,-2.04168791594811,
-1.11730839831501));
#43066=CARTESIAN_POINT('Ctrl Pts',(-4.46536142053643,-1.86454239160906,
-1.56386495711831));
#43067=CARTESIAN_POINT('Ctrl Pts',(-4.43189298349968,-1.31772490077559,
-2.41136229140832));
#43068=CARTESIAN_POINT('Ctrl Pts',(-4.4165944181758,-0.969292128617316,
-2.72756811571645));
#43069=CARTESIAN_POINT('Ctrl Pts',(-4.38786764570481,-0.257902067365425,
-3.22265134720374));
#43070=CARTESIAN_POINT('Ctrl Pts',(-4.3720655535929,0.186687863837912,-3.41907230663807));
#43071=CARTESIAN_POINT('Ctrl Pts',(-4.34131730068888,1.09209617603561,-3.61408512036354));
#43072=CARTESIAN_POINT('Ctrl Pts',(-4.32640535038746,1.54962604562836,-3.62272692428965));
#43073=CARTESIAN_POINT('Ctrl Pts',(-4.29859919994289,2.37762120426604,-3.48733627110506));
#43074=CARTESIAN_POINT('Ctrl Pts',(-4.28293979780371,2.84014549425617,-3.35073711466903));
#43075=CARTESIAN_POINT('Ctrl Pts',(-4.24928211437871,3.70032747207834,-2.81351240010709));
#43076=CARTESIAN_POINT('Ctrl Pts',(-4.2340004472364,4.04380952851942,-2.49313866036689));
#43077=CARTESIAN_POINT('Ctrl Pts',(-4.20295271590267,4.59774222529018,-1.73815589466744));
#43078=CARTESIAN_POINT('Ctrl Pts',(-4.18751045174126,4.79759186945824,-1.3082142296864));
#43079=CARTESIAN_POINT('Ctrl Pts',(-4.1560652472825,5.01733524992041,-0.385795687503433));
#43080=CARTESIAN_POINT('Ctrl Pts',(-4.14044873203137,5.03744682663507,0.0942360700334427));
#43081=CARTESIAN_POINT('Ctrl Pts',(-4.10798155174798,4.88808108123792,1.0610710502257));
#43082=CARTESIAN_POINT('Ctrl Pts',(-4.09343427343297,4.71532883305283,1.4724843596549));
#43083=CARTESIAN_POINT('Ctrl Pts',(-4.08091832701493,4.52608525525901,1.79907266101289));
#43084=CARTESIAN_POINT('Ctrl Pts',(-6.968838791574,-0.05425191507289,-3.288763647513));
#43085=CARTESIAN_POINT('Ctrl Pts',(-6.941755458241,0.6919448865242,-3.62099186847));
#43086=CARTESIAN_POINT('Ctrl Pts',(-6.887588791574,2.41608097904,-3.756179714594));
#43087=CARTESIAN_POINT('Ctrl Pts',(-6.806338791574,4.556290617787,-2.28588104406));
#43088=CARTESIAN_POINT('Ctrl Pts',(-6.725088791574,5.293523628312,0.2035424413179));
#43089=CARTESIAN_POINT('Ctrl Pts',(-6.643838791574,4.300012819665,2.602167933636));
#43090=CARTESIAN_POINT('Ctrl Pts',(-6.562588791574,2.018353323341,3.841006921488));
#43091=CARTESIAN_POINT('Ctrl Pts',(-6.481338791574,-0.5344416681603,3.367872537265));
#43092=CARTESIAN_POINT('Ctrl Pts',(-6.400088791574,-2.2205866507,1.393651651195));
#43093=CARTESIAN_POINT('Ctrl Pts',(-6.318838791574,-2.288548941379,-1.201731431865));
#43094=CARTESIAN_POINT('Ctrl Pts',(-6.237588791574,-0.7080383357597,-3.261493002233));
#43095=CARTESIAN_POINT('Ctrl Pts',(-6.156338791574,1.816499128093,-3.867580826823));
#43096=CARTESIAN_POINT('Ctrl Pts',(-6.075088791574,4.159856629968,-2.74985663043));
#43097=CARTESIAN_POINT('Ctrl Pts',(-5.993838791574,5.277580825662,-0.4064991250853));
#43098=CARTESIAN_POINT('Ctrl Pts',(-5.912588791574,4.671493007336,2.11803832419));
#43099=CARTESIAN_POINT('Ctrl Pts',(-5.831338791574,2.611731412613,3.698548984649));
#43100=CARTESIAN_POINT('Ctrl Pts',(-5.750088791574,0.01634842071054,3.630586489191));
#43101=CARTESIAN_POINT('Ctrl Pts',(-5.668838791574,-1.957872805634,1.944442270929));
#43102=CARTESIAN_POINT('Ctrl Pts',(-5.587588791574,-2.43100591992,-0.6083555729063));
#43103=CARTESIAN_POINT('Ctrl Pts',(-5.506338791574,-1.19217167154,-2.890004424173));
#43104=CARTESIAN_POINT('Ctrl Pts',(-5.425088791574,1.20647150873,-3.883554960714));
#43105=CARTESIAN_POINT('Ctrl Pts',(-5.343838791574,3.695828981771,-3.146173683671));
#43106=CARTESIAN_POINT('Ctrl Pts',(-5.262588791574,5.166374013702,-1.006517383103));
#43107=CARTESIAN_POINT('Ctrl Pts',(-5.181338791574,4.962672811265,1.581751841867));
#43108=CARTESIAN_POINT('Ctrl Pts',(-5.100088791574,3.175516626319,3.465021506074));
#43109=CARTESIAN_POINT('Ctrl Pts',(-5.018838791574,0.6014554778319,3.803903056307));
#43110=CARTESIAN_POINT('Ctrl Pts',(-4.937588791574,-1.612231059311,2.44735444455));
#43111=CARTESIAN_POINT('Ctrl Pts',(-4.856338791574,-2.47888400806,-3.87828836268E-7));
#43112=CARTESIAN_POINT('Ctrl Pts',(-4.775088791574,-1.61223290845,-2.447352893234));
#43113=CARTESIAN_POINT('Ctrl Pts',(-4.693838791574,0.6014628743901,-3.80390848591));
#43114=CARTESIAN_POINT('Ctrl Pts',(-4.612588791574,3.175488889226,-3.465001338974));
#43115=CARTESIAN_POINT('Ctrl Pts',(-4.531338791574,4.962776363079,-1.581827080662));
#43116=CARTESIAN_POINT('Ctrl Pts',(-4.450088791574,5.165987543538,1.006798171184));
#43117=CARTESIAN_POINT('Ctrl Pts',(-4.395922124908,4.186843388254,2.432349903822));
#43118=CARTESIAN_POINT('Ctrl Pts',(-4.368838791574,3.526026908253,2.91246117975));
#43119=CARTESIAN_POINT('Ctrl Pts',(-6.839612930525,-0.05425191507289,-3.288763647513));
#43120=CARTESIAN_POINT('Ctrl Pts',(-6.812529597191,0.6919448865242,-3.62099186847));
#43121=CARTESIAN_POINT('Ctrl Pts',(-6.758362930525,2.41608097904,-3.756179714594));
#43122=CARTESIAN_POINT('Ctrl Pts',(-6.677112930525,4.556290617787,-2.28588104406));
#43123=CARTESIAN_POINT('Ctrl Pts',(-6.595862930525,5.293523628312,0.2035424413179));
#43124=CARTESIAN_POINT('Ctrl Pts',(-6.514612930525,4.300012819665,2.602167933636));
#43125=CARTESIAN_POINT('Ctrl Pts',(-6.433362930525,2.018353323341,3.841006921488));
#43126=CARTESIAN_POINT('Ctrl Pts',(-6.352112930525,-0.5344416681603,3.367872537265));
#43127=CARTESIAN_POINT('Ctrl Pts',(-6.270862930525,-2.2205866507,1.393651651195));
#43128=CARTESIAN_POINT('Ctrl Pts',(-6.189612930525,-2.288548941379,-1.201731431865));
#43129=CARTESIAN_POINT('Ctrl Pts',(-6.108362930525,-0.7080383357597,-3.261493002233));
#43130=CARTESIAN_POINT('Ctrl Pts',(-6.027112930525,1.816499128093,-3.867580826823));
#43131=CARTESIAN_POINT('Ctrl Pts',(-5.945862930525,4.159856629968,-2.74985663043));
#43132=CARTESIAN_POINT('Ctrl Pts',(-5.864612930525,5.277580825662,-0.4064991250853));
#43133=CARTESIAN_POINT('Ctrl Pts',(-5.783362930525,4.671493007336,2.11803832419));
#43134=CARTESIAN_POINT('Ctrl Pts',(-5.702112930525,2.611731412613,3.698548984649));
#43135=CARTESIAN_POINT('Ctrl Pts',(-5.620862930525,0.01634842071054,3.630586489191));
#43136=CARTESIAN_POINT('Ctrl Pts',(-5.539612930525,-1.957872805634,1.944442270929));
#43137=CARTESIAN_POINT('Ctrl Pts',(-5.458362930525,-2.43100591992,-0.6083555729063));
#43138=CARTESIAN_POINT('Ctrl Pts',(-5.377112930525,-1.19217167154,-2.890004424173));
#43139=CARTESIAN_POINT('Ctrl Pts',(-5.295862930525,1.20647150873,-3.883554960714));
#43140=CARTESIAN_POINT('Ctrl Pts',(-5.214612930525,3.695828981771,-3.146173683671));
#43141=CARTESIAN_POINT('Ctrl Pts',(-5.133362930525,5.166374013702,-1.006517383103));
#43142=CARTESIAN_POINT('Ctrl Pts',(-5.052112930525,4.962672811265,1.581751841867));
#43143=CARTESIAN_POINT('Ctrl Pts',(-4.970862930525,3.175516626319,3.465021506074));
#43144=CARTESIAN_POINT('Ctrl Pts',(-4.889612930525,0.6014554778319,3.803903056307));
#43145=CARTESIAN_POINT('Ctrl Pts',(-4.808362930525,-1.612231059311,2.44735444455));
#43146=CARTESIAN_POINT('Ctrl Pts',(-4.727112930525,-2.47888400806,-3.87828836268E-7));
#43147=CARTESIAN_POINT('Ctrl Pts',(-4.645862930525,-1.61223290845,-2.447352893234));
#43148=CARTESIAN_POINT('Ctrl Pts',(-4.564612930525,0.6014628743901,-3.80390848591));
#43149=CARTESIAN_POINT('Ctrl Pts',(-4.483362930525,3.175488889226,-3.465001338974));
#43150=CARTESIAN_POINT('Ctrl Pts',(-4.402112930525,4.962776363079,-1.581827080662));
#43151=CARTESIAN_POINT('Ctrl Pts',(-4.320862930525,5.165987543538,1.006798171184));
#43152=CARTESIAN_POINT('Ctrl Pts',(-4.266696263858,4.186843388254,2.432349903822));
#43153=CARTESIAN_POINT('Ctrl Pts',(-4.239612930525,3.526026908253,2.91246117975));
#43154=CARTESIAN_POINT('Ctrl Pts',(-6.710387069475,-0.05425191507289,-3.288763647513));
#43155=CARTESIAN_POINT('Ctrl Pts',(-6.683303736142,0.6919448865242,-3.62099186847));
#43156=CARTESIAN_POINT('Ctrl Pts',(-6.629137069475,2.41608097904,-3.756179714594));
#43157=CARTESIAN_POINT('Ctrl Pts',(-6.547887069475,4.556290617787,-2.28588104406));
#43158=CARTESIAN_POINT('Ctrl Pts',(-6.466637069475,5.293523628312,0.2035424413179));
#43159=CARTESIAN_POINT('Ctrl Pts',(-6.385387069475,4.300012819665,2.602167933636));
#43160=CARTESIAN_POINT('Ctrl Pts',(-6.304137069475,2.018353323341,3.841006921488));
#43161=CARTESIAN_POINT('Ctrl Pts',(-6.222887069475,-0.5344416681603,3.367872537265));
#43162=CARTESIAN_POINT('Ctrl Pts',(-6.141637069475,-2.2205866507,1.393651651195));
#43163=CARTESIAN_POINT('Ctrl Pts',(-6.060387069475,-2.288548941379,-1.201731431865));
#43164=CARTESIAN_POINT('Ctrl Pts',(-5.979137069475,-0.7080383357597,-3.261493002233));
#43165=CARTESIAN_POINT('Ctrl Pts',(-5.897887069475,1.816499128093,-3.867580826823));
#43166=CARTESIAN_POINT('Ctrl Pts',(-5.816637069475,4.159856629968,-2.74985663043));
#43167=CARTESIAN_POINT('Ctrl Pts',(-5.735387069475,5.277580825662,-0.4064991250853));
#43168=CARTESIAN_POINT('Ctrl Pts',(-5.654137069475,4.671493007336,2.11803832419));
#43169=CARTESIAN_POINT('Ctrl Pts',(-5.572887069475,2.611731412613,3.698548984649));
#43170=CARTESIAN_POINT('Ctrl Pts',(-5.491637069475,0.01634842071054,3.630586489191));
#43171=CARTESIAN_POINT('Ctrl Pts',(-5.410387069475,-1.957872805634,1.944442270929));
#43172=CARTESIAN_POINT('Ctrl Pts',(-5.329137069475,-2.43100591992,-0.6083555729063));
#43173=CARTESIAN_POINT('Ctrl Pts',(-5.247887069475,-1.19217167154,-2.890004424173));
#43174=CARTESIAN_POINT('Ctrl Pts',(-5.166637069475,1.20647150873,-3.883554960714));
#43175=CARTESIAN_POINT('Ctrl Pts',(-5.085387069475,3.695828981771,-3.146173683671));
#43176=CARTESIAN_POINT('Ctrl Pts',(-5.004137069475,5.166374013702,-1.006517383103));
#43177=CARTESIAN_POINT('Ctrl Pts',(-4.922887069475,4.962672811265,1.581751841867));
#43178=CARTESIAN_POINT('Ctrl Pts',(-4.841637069475,3.175516626319,3.465021506074));
#43179=CARTESIAN_POINT('Ctrl Pts',(-4.760387069475,0.6014554778319,3.803903056307));
#43180=CARTESIAN_POINT('Ctrl Pts',(-4.679137069475,-1.612231059311,2.44735444455));
#43181=CARTESIAN_POINT('Ctrl Pts',(-4.597887069475,-2.47888400806,-3.87828836268E-7));
#43182=CARTESIAN_POINT('Ctrl Pts',(-4.516637069475,-1.61223290845,-2.447352893234));
#43183=CARTESIAN_POINT('Ctrl Pts',(-4.435387069475,0.6014628743901,-3.80390848591));
#43184=CARTESIAN_POINT('Ctrl Pts',(-4.354137069475,3.175488889226,-3.465001338974));
#43185=CARTESIAN_POINT('Ctrl Pts',(-4.272887069475,4.962776363079,-1.581827080662));
#43186=CARTESIAN_POINT('Ctrl Pts',(-4.191637069475,5.165987543538,1.006798171184));
#43187=CARTESIAN_POINT('Ctrl Pts',(-4.137470402809,4.186843388254,2.432349903822));
#43188=CARTESIAN_POINT('Ctrl Pts',(-4.110387069475,3.526026908253,2.91246117975));
#43189=CARTESIAN_POINT('Ctrl Pts',(-6.581161208426,-0.05425191507289,-3.288763647513));
#43190=CARTESIAN_POINT('Ctrl Pts',(-6.554077875092,0.6919448865242,-3.62099186847));
#43191=CARTESIAN_POINT('Ctrl Pts',(-6.499911208426,2.41608097904,-3.756179714594));
#43192=CARTESIAN_POINT('Ctrl Pts',(-6.418661208426,4.556290617787,-2.28588104406));
#43193=CARTESIAN_POINT('Ctrl Pts',(-6.337411208426,5.293523628312,0.2035424413179));
#43194=CARTESIAN_POINT('Ctrl Pts',(-6.256161208426,4.300012819665,2.602167933636));
#43195=CARTESIAN_POINT('Ctrl Pts',(-6.174911208426,2.018353323341,3.841006921488));
#43196=CARTESIAN_POINT('Ctrl Pts',(-6.093661208426,-0.5344416681603,3.367872537265));
#43197=CARTESIAN_POINT('Ctrl Pts',(-6.012411208426,-2.2205866507,1.393651651195));
#43198=CARTESIAN_POINT('Ctrl Pts',(-5.931161208426,-2.288548941379,-1.201731431865));
#43199=CARTESIAN_POINT('Ctrl Pts',(-5.849911208426,-0.7080383357597,-3.261493002233));
#43200=CARTESIAN_POINT('Ctrl Pts',(-5.768661208426,1.816499128093,-3.867580826823));
#43201=CARTESIAN_POINT('Ctrl Pts',(-5.687411208426,4.159856629968,-2.74985663043));
#43202=CARTESIAN_POINT('Ctrl Pts',(-5.606161208426,5.277580825662,-0.4064991250853));
#43203=CARTESIAN_POINT('Ctrl Pts',(-5.524911208426,4.671493007336,2.11803832419));
#43204=CARTESIAN_POINT('Ctrl Pts',(-5.443661208426,2.611731412613,3.698548984649));
#43205=CARTESIAN_POINT('Ctrl Pts',(-5.362411208426,0.01634842071054,3.630586489191));
#43206=CARTESIAN_POINT('Ctrl Pts',(-5.281161208426,-1.957872805634,1.944442270929));
#43207=CARTESIAN_POINT('Ctrl Pts',(-5.199911208426,-2.43100591992,-0.6083555729063));
#43208=CARTESIAN_POINT('Ctrl Pts',(-5.118661208426,-1.19217167154,-2.890004424173));
#43209=CARTESIAN_POINT('Ctrl Pts',(-5.037411208426,1.20647150873,-3.883554960714));
#43210=CARTESIAN_POINT('Ctrl Pts',(-4.956161208426,3.695828981771,-3.146173683671));
#43211=CARTESIAN_POINT('Ctrl Pts',(-4.874911208426,5.166374013702,-1.006517383103));
#43212=CARTESIAN_POINT('Ctrl Pts',(-4.793661208426,4.962672811265,1.581751841867));
#43213=CARTESIAN_POINT('Ctrl Pts',(-4.712411208426,3.175516626319,3.465021506074));
#43214=CARTESIAN_POINT('Ctrl Pts',(-4.631161208426,0.6014554778319,3.803903056307));
#43215=CARTESIAN_POINT('Ctrl Pts',(-4.549911208426,-1.612231059311,2.44735444455));
#43216=CARTESIAN_POINT('Ctrl Pts',(-4.468661208426,-2.47888400806,-3.87828836268E-7));
#43217=CARTESIAN_POINT('Ctrl Pts',(-4.387411208426,-1.61223290845,-2.447352893234));
#43218=CARTESIAN_POINT('Ctrl Pts',(-4.306161208426,0.6014628743901,-3.80390848591));
#43219=CARTESIAN_POINT('Ctrl Pts',(-4.224911208426,3.175488889226,-3.465001338974));
#43220=CARTESIAN_POINT('Ctrl Pts',(-4.143661208426,4.962776363079,-1.581827080662));
#43221=CARTESIAN_POINT('Ctrl Pts',(-4.062411208426,5.165987543538,1.006798171184));
#43222=CARTESIAN_POINT('Ctrl Pts',(-4.008244541759,4.186843388254,2.432349903822));
#43223=CARTESIAN_POINT('Ctrl Pts',(-3.981161208426,3.526026908253,2.91246117975));
#43224=CARTESIAN_POINT('',(-6.869059892324,1.41,-3.6));
#43225=CARTESIAN_POINT('Ctrl Pts',(-4.36903811233822,4.52608525529002,1.79907266095937));
#43226=CARTESIAN_POINT('Ctrl Pts',(-4.32102540822548,4.52608525529002,1.79907266095937));
#43227=CARTESIAN_POINT('Ctrl Pts',(-4.27301270411274,4.52608525529002,1.79907266095937));
#43228=CARTESIAN_POINT('Ctrl Pts',(-4.17697277545765,4.52608525529002,1.79907266095937));
#43229=CARTESIAN_POINT('Ctrl Pts',(-4.1289455509153,4.52608525529002,1.79907266095937));
#43230=CARTESIAN_POINT('Ctrl Pts',(-4.08091832637295,4.52608525529002,1.79907266095937));
#43231=CARTESIAN_POINT('Ctrl Pts',(-9.468838791574,-0.7060269082529,2.91246117975));
#43232=CARTESIAN_POINT('Ctrl Pts',(-9.441755458241,-1.366843388254,2.432349903822));
#43233=CARTESIAN_POINT('Ctrl Pts',(-9.387588791574,-2.345987543538,1.006798171184));
#43234=CARTESIAN_POINT('Ctrl Pts',(-9.306338791574,-2.142776363079,-1.581827080662));
#43235=CARTESIAN_POINT('Ctrl Pts',(-9.225088791574,-0.3554888892263,-3.465001338974));
#43236=CARTESIAN_POINT('Ctrl Pts',(-9.143838791574,2.21853712561,-3.80390848591));
#43237=CARTESIAN_POINT('Ctrl Pts',(-9.062588791574,4.43223290845,-2.447352893234));
#43238=CARTESIAN_POINT('Ctrl Pts',(-8.981338791574,5.29888400806,-3.878288208359E-7));
#43239=CARTESIAN_POINT('Ctrl Pts',(-8.900088791574,4.432231059311,2.44735444455));
#43240=CARTESIAN_POINT('Ctrl Pts',(-8.818838791574,2.218544522168,3.803903056307));
#43241=CARTESIAN_POINT('Ctrl Pts',(-8.737588791574,-0.3555166263194,3.465021506074));
#43242=CARTESIAN_POINT('Ctrl Pts',(-8.656338791574,-2.142672811265,1.581751841867));
#43243=CARTESIAN_POINT('Ctrl Pts',(-8.575088791574,-2.346374013702,-1.006517383103));
#43244=CARTESIAN_POINT('Ctrl Pts',(-8.493838791574,-0.8758289817713,-3.146173683671));
#43245=CARTESIAN_POINT('Ctrl Pts',(-8.412588791574,1.61352849127,-3.883554960714));
#43246=CARTESIAN_POINT('Ctrl Pts',(-8.331338791574,4.01217167154,-2.890004424173));
#43247=CARTESIAN_POINT('Ctrl Pts',(-8.250088791574,5.25100591992,-0.6083555729063));
#43248=CARTESIAN_POINT('Ctrl Pts',(-8.168838791574,4.777872805634,1.944442270929));
#43249=CARTESIAN_POINT('Ctrl Pts',(-8.087588791574,2.803651579289,3.63058648919));
#43250=CARTESIAN_POINT('Ctrl Pts',(-8.006338791574,0.208268587387,3.698548984649));
#43251=CARTESIAN_POINT('Ctrl Pts',(-7.925088791574,-1.851493007336,2.11803832419));
#43252=CARTESIAN_POINT('Ctrl Pts',(-7.843838791574,-2.457580825662,-0.4064991250853));
#43253=CARTESIAN_POINT('Ctrl Pts',(-7.762588791574,-1.339856629968,-2.74985663043));
#43254=CARTESIAN_POINT('Ctrl Pts',(-7.681338791574,1.003500871907,-3.867580826823));
#43255=CARTESIAN_POINT('Ctrl Pts',(-7.600088791574,3.52803833576,-3.261493002233));
#43256=CARTESIAN_POINT('Ctrl Pts',(-7.518838791574,5.108548941379,-1.201731431865));
#43257=CARTESIAN_POINT('Ctrl Pts',(-7.437588791574,5.0405866507,1.393651651195));
#43258=CARTESIAN_POINT('Ctrl Pts',(-7.356338791574,3.35444166816,3.367872537265));
#43259=CARTESIAN_POINT('Ctrl Pts',(-7.275088791574,0.8016466766589,3.841006921488));
#43260=CARTESIAN_POINT('Ctrl Pts',(-7.193838791574,-1.480012819665,2.602167933636));
#43261=CARTESIAN_POINT('Ctrl Pts',(-7.112588791574,-2.473523628312,0.203542441318));
#43262=CARTESIAN_POINT('Ctrl Pts',(-7.031338791574,-1.736290617787,-2.28588104406));
#43263=CARTESIAN_POINT('Ctrl Pts',(-6.950088791574,0.4039190209595,-3.756179714594));
#43264=CARTESIAN_POINT('Ctrl Pts',(-6.895922124908,2.128055113476,-3.62099186847));
#43265=CARTESIAN_POINT('Ctrl Pts',(-6.868838791574,2.874251915073,-3.288763647513));
#43266=CARTESIAN_POINT('Ctrl Pts',(-9.339612930525,-0.7060269082529,2.91246117975));
#43267=CARTESIAN_POINT('Ctrl Pts',(-9.312529597191,-1.366843388254,2.432349903822));
#43268=CARTESIAN_POINT('Ctrl Pts',(-9.258362930525,-2.345987543538,1.006798171184));
#43269=CARTESIAN_POINT('Ctrl Pts',(-9.177112930525,-2.142776363079,-1.581827080662));
#43270=CARTESIAN_POINT('Ctrl Pts',(-9.095862930525,-0.3554888892263,-3.465001338974));
#43271=CARTESIAN_POINT('Ctrl Pts',(-9.014612930525,2.21853712561,-3.80390848591));
#43272=CARTESIAN_POINT('Ctrl Pts',(-8.933362930525,4.43223290845,-2.447352893234));
#43273=CARTESIAN_POINT('Ctrl Pts',(-8.852112930525,5.29888400806,-3.878288208359E-7));
#43274=CARTESIAN_POINT('Ctrl Pts',(-8.770862930525,4.432231059311,2.44735444455));
#43275=CARTESIAN_POINT('Ctrl Pts',(-8.689612930525,2.218544522168,3.803903056307));
#43276=CARTESIAN_POINT('Ctrl Pts',(-8.608362930525,-0.3555166263194,3.465021506074));
#43277=CARTESIAN_POINT('Ctrl Pts',(-8.527112930525,-2.142672811265,1.581751841867));
#43278=CARTESIAN_POINT('Ctrl Pts',(-8.445862930525,-2.346374013702,-1.006517383103));
#43279=CARTESIAN_POINT('Ctrl Pts',(-8.364612930525,-0.8758289817713,-3.146173683671));
#43280=CARTESIAN_POINT('Ctrl Pts',(-8.283362930525,1.61352849127,-3.883554960714));
#43281=CARTESIAN_POINT('Ctrl Pts',(-8.202112930525,4.01217167154,-2.890004424173));
#43282=CARTESIAN_POINT('Ctrl Pts',(-8.120862930525,5.25100591992,-0.6083555729063));
#43283=CARTESIAN_POINT('Ctrl Pts',(-8.039612930525,4.777872805634,1.944442270929));
#43284=CARTESIAN_POINT('Ctrl Pts',(-7.958362930525,2.803651579289,3.63058648919));
#43285=CARTESIAN_POINT('Ctrl Pts',(-7.877112930525,0.208268587387,3.698548984649));
#43286=CARTESIAN_POINT('Ctrl Pts',(-7.795862930525,-1.851493007336,2.11803832419));
#43287=CARTESIAN_POINT('Ctrl Pts',(-7.714612930525,-2.457580825662,-0.4064991250853));
#43288=CARTESIAN_POINT('Ctrl Pts',(-7.633362930525,-1.339856629968,-2.74985663043));
#43289=CARTESIAN_POINT('Ctrl Pts',(-7.552112930525,1.003500871907,-3.867580826823));
#43290=CARTESIAN_POINT('Ctrl Pts',(-7.470862930525,3.52803833576,-3.261493002233));
#43291=CARTESIAN_POINT('Ctrl Pts',(-7.389612930525,5.108548941379,-1.201731431865));
#43292=CARTESIAN_POINT('Ctrl Pts',(-7.308362930525,5.0405866507,1.393651651195));
#43293=CARTESIAN_POINT('Ctrl Pts',(-7.227112930525,3.35444166816,3.367872537265));
#43294=CARTESIAN_POINT('Ctrl Pts',(-7.145862930525,0.8016466766589,3.841006921488));
#43295=CARTESIAN_POINT('Ctrl Pts',(-7.064612930525,-1.480012819665,2.602167933636));
#43296=CARTESIAN_POINT('Ctrl Pts',(-6.983362930525,-2.473523628312,0.203542441318));
#43297=CARTESIAN_POINT('Ctrl Pts',(-6.902112930525,-1.736290617787,-2.28588104406));
#43298=CARTESIAN_POINT('Ctrl Pts',(-6.820862930525,0.4039190209595,-3.756179714594));
#43299=CARTESIAN_POINT('Ctrl Pts',(-6.766696263858,2.128055113476,-3.62099186847));
#43300=CARTESIAN_POINT('Ctrl Pts',(-6.739612930525,2.874251915073,-3.288763647513));
#43301=CARTESIAN_POINT('Ctrl Pts',(-9.210387069475,-0.7060269082529,2.91246117975));
#43302=CARTESIAN_POINT('Ctrl Pts',(-9.183303736142,-1.366843388254,2.432349903822));
#43303=CARTESIAN_POINT('Ctrl Pts',(-9.129137069475,-2.345987543538,1.006798171184));
#43304=CARTESIAN_POINT('Ctrl Pts',(-9.047887069475,-2.142776363079,-1.581827080662));
#43305=CARTESIAN_POINT('Ctrl Pts',(-8.966637069475,-0.3554888892263,-3.465001338974));
#43306=CARTESIAN_POINT('Ctrl Pts',(-8.885387069475,2.21853712561,-3.80390848591));
#43307=CARTESIAN_POINT('Ctrl Pts',(-8.804137069475,4.43223290845,-2.447352893234));
#43308=CARTESIAN_POINT('Ctrl Pts',(-8.722887069475,5.29888400806,-3.878288207249E-7));
#43309=CARTESIAN_POINT('Ctrl Pts',(-8.641637069475,4.432231059311,2.44735444455));
#43310=CARTESIAN_POINT('Ctrl Pts',(-8.560387069475,2.218544522168,3.803903056307));
#43311=CARTESIAN_POINT('Ctrl Pts',(-8.479137069475,-0.3555166263194,3.465021506074));
#43312=CARTESIAN_POINT('Ctrl Pts',(-8.397887069475,-2.142672811265,1.581751841867));
#43313=CARTESIAN_POINT('Ctrl Pts',(-8.316637069475,-2.346374013702,-1.006517383103));
#43314=CARTESIAN_POINT('Ctrl Pts',(-8.235387069475,-0.8758289817713,-3.146173683671));
#43315=CARTESIAN_POINT('Ctrl Pts',(-8.154137069475,1.61352849127,-3.883554960714));
#43316=CARTESIAN_POINT('Ctrl Pts',(-8.072887069475,4.01217167154,-2.890004424173));
#43317=CARTESIAN_POINT('Ctrl Pts',(-7.991637069475,5.25100591992,-0.6083555729063));
#43318=CARTESIAN_POINT('Ctrl Pts',(-7.910387069475,4.777872805634,1.944442270929));
#43319=CARTESIAN_POINT('Ctrl Pts',(-7.829137069475,2.803651579289,3.63058648919));
#43320=CARTESIAN_POINT('Ctrl Pts',(-7.747887069475,0.208268587387,3.698548984649));
#43321=CARTESIAN_POINT('Ctrl Pts',(-7.666637069475,-1.851493007336,2.11803832419));
#43322=CARTESIAN_POINT('Ctrl Pts',(-7.585387069475,-2.457580825662,-0.4064991250853));
#43323=CARTESIAN_POINT('Ctrl Pts',(-7.504137069475,-1.339856629968,-2.74985663043));
#43324=CARTESIAN_POINT('Ctrl Pts',(-7.422887069475,1.003500871907,-3.867580826823));
#43325=CARTESIAN_POINT('Ctrl Pts',(-7.341637069475,3.52803833576,-3.261493002233));
#43326=CARTESIAN_POINT('Ctrl Pts',(-7.260387069475,5.108548941379,-1.201731431865));
#43327=CARTESIAN_POINT('Ctrl Pts',(-7.179137069475,5.0405866507,1.393651651195));
#43328=CARTESIAN_POINT('Ctrl Pts',(-7.097887069475,3.35444166816,3.367872537265));
#43329=CARTESIAN_POINT('Ctrl Pts',(-7.016637069475,0.8016466766589,3.841006921488));
#43330=CARTESIAN_POINT('Ctrl Pts',(-6.935387069475,-1.480012819665,2.602167933636));
#43331=CARTESIAN_POINT('Ctrl Pts',(-6.854137069475,-2.473523628312,0.203542441318));
#43332=CARTESIAN_POINT('Ctrl Pts',(-6.772887069475,-1.736290617787,-2.28588104406));
#43333=CARTESIAN_POINT('Ctrl Pts',(-6.691637069475,0.4039190209595,-3.756179714594));
#43334=CARTESIAN_POINT('Ctrl Pts',(-6.637470402809,2.128055113476,-3.62099186847));
#43335=CARTESIAN_POINT('Ctrl Pts',(-6.610387069475,2.874251915073,-3.288763647513));
#43336=CARTESIAN_POINT('Ctrl Pts',(-9.081161208426,-0.7060269082529,2.91246117975));
#43337=CARTESIAN_POINT('Ctrl Pts',(-9.054077875092,-1.366843388254,2.432349903822));
#43338=CARTESIAN_POINT('Ctrl Pts',(-8.999911208426,-2.345987543538,1.006798171184));
#43339=CARTESIAN_POINT('Ctrl Pts',(-8.918661208426,-2.142776363079,-1.581827080662));
#43340=CARTESIAN_POINT('Ctrl Pts',(-8.837411208426,-0.3554888892263,-3.465001338974));
#43341=CARTESIAN_POINT('Ctrl Pts',(-8.756161208426,2.21853712561,-3.80390848591));
#43342=CARTESIAN_POINT('Ctrl Pts',(-8.674911208426,4.43223290845,-2.447352893234));
#43343=CARTESIAN_POINT('Ctrl Pts',(-8.593661208426,5.29888400806,-3.878288207249E-7));
#43344=CARTESIAN_POINT('Ctrl Pts',(-8.512411208426,4.432231059311,2.44735444455));
#43345=CARTESIAN_POINT('Ctrl Pts',(-8.431161208426,2.218544522168,3.803903056307));
#43346=CARTESIAN_POINT('Ctrl Pts',(-8.349911208426,-0.3555166263194,3.465021506074));
#43347=CARTESIAN_POINT('Ctrl Pts',(-8.268661208426,-2.142672811265,1.581751841867));
#43348=CARTESIAN_POINT('Ctrl Pts',(-8.187411208426,-2.346374013702,-1.006517383103));
#43349=CARTESIAN_POINT('Ctrl Pts',(-8.106161208426,-0.8758289817713,-3.146173683671));
#43350=CARTESIAN_POINT('Ctrl Pts',(-8.024911208426,1.61352849127,-3.883554960714));
#43351=CARTESIAN_POINT('Ctrl Pts',(-7.943661208426,4.01217167154,-2.890004424173));
#43352=CARTESIAN_POINT('Ctrl Pts',(-7.862411208426,5.25100591992,-0.6083555729063));
#43353=CARTESIAN_POINT('Ctrl Pts',(-7.781161208426,4.777872805634,1.944442270929));
#43354=CARTESIAN_POINT('Ctrl Pts',(-7.699911208426,2.803651579289,3.63058648919));
#43355=CARTESIAN_POINT('Ctrl Pts',(-7.618661208426,0.208268587387,3.698548984649));
#43356=CARTESIAN_POINT('Ctrl Pts',(-7.537411208426,-1.851493007336,2.11803832419));
#43357=CARTESIAN_POINT('Ctrl Pts',(-7.456161208426,-2.457580825662,-0.4064991250853));
#43358=CARTESIAN_POINT('Ctrl Pts',(-7.374911208426,-1.339856629968,-2.74985663043));
#43359=CARTESIAN_POINT('Ctrl Pts',(-7.293661208426,1.003500871907,-3.867580826823));
#43360=CARTESIAN_POINT('Ctrl Pts',(-7.212411208426,3.52803833576,-3.261493002233));
#43361=CARTESIAN_POINT('Ctrl Pts',(-7.131161208426,5.108548941379,-1.201731431865));
#43362=CARTESIAN_POINT('Ctrl Pts',(-7.049911208426,5.0405866507,1.393651651195));
#43363=CARTESIAN_POINT('Ctrl Pts',(-6.968661208426,3.35444166816,3.367872537265));
#43364=CARTESIAN_POINT('Ctrl Pts',(-6.887411208426,0.8016466766589,3.841006921488));
#43365=CARTESIAN_POINT('Ctrl Pts',(-6.806161208426,-1.480012819665,2.602167933636));
#43366=CARTESIAN_POINT('Ctrl Pts',(-6.724911208426,-2.473523628312,0.203542441318));
#43367=CARTESIAN_POINT('Ctrl Pts',(-6.643661208426,-1.736290617787,-2.28588104406));
#43368=CARTESIAN_POINT('Ctrl Pts',(-6.562411208426,0.4039190209595,-3.756179714594));
#43369=CARTESIAN_POINT('Ctrl Pts',(-6.508244541759,2.128055113476,-3.62099186847));
#43370=CARTESIAN_POINT('Ctrl Pts',(-6.481161208426,2.874251915073,-3.288763647513));
#43371=CARTESIAN_POINT('Origin',(-4.6,4.874101615138,2.));
#43372=CARTESIAN_POINT('Origin',(-3.1,0.,0.));
#43373=CARTESIAN_POINT('',(-3.1,1.41,-6.));
#43374=CARTESIAN_POINT('Origin',(-3.1,1.41,0.));
#43375=CARTESIAN_POINT('Origin',(5.25,1.41,0.));
#43376=CARTESIAN_POINT('',(4.25,1.41,-6.));
#43377=CARTESIAN_POINT('',(5.25,1.41,-6.));
#43378=CARTESIAN_POINT('Origin',(4.25,1.41,0.));
#43379=CARTESIAN_POINT('',(0.,5.68,-4.215103794689));
#43380=CARTESIAN_POINT('',(1.63085988542761E-16,5.68,4.21510379468881));
#43381=CARTESIAN_POINT('Ctrl Pts',(0.,5.68,-4.21510379468881));
#43382=CARTESIAN_POINT('Ctrl Pts',(-0.266706680138663,5.68,-4.21510379468881));
#43383=CARTESIAN_POINT('Ctrl Pts',(-0.552196963605974,5.71567698479767,
-4.17989549259779));
#43384=CARTESIAN_POINT('Ctrl Pts',(-1.08458290107335,5.85511893191279,-4.03129022106372));
#43385=CARTESIAN_POINT('Ctrl Pts',(-1.33144862194443,5.95819559552318,-3.9171419061609));
#43386=CARTESIAN_POINT('Ctrl Pts',(-1.81218560208282,6.21764548689165,-3.59767135677579));
#43387=CARTESIAN_POINT('Ctrl Pts',(-2.03213201249546,6.38798517315582,-3.36454771509492));
#43388=CARTESIAN_POINT('Ctrl Pts',(-2.38147333747754,6.71484535620929,-2.82119365553778));
#43389=CARTESIAN_POINT('Ctrl Pts',(-2.51052533147875,6.871296113951,-2.51070089780968));
#43390=CARTESIAN_POINT('Ctrl Pts',(-2.79703133737243,7.26257643241256,-1.50498437334144));
#43391=CARTESIAN_POINT('Ctrl Pts',(-2.86057686489981,7.41,-0.73226230454066));
#43392=CARTESIAN_POINT('Ctrl Pts',(-2.86057686489981,7.41,0.));
#43393=CARTESIAN_POINT('Ctrl Pts',(-2.86057686489981,7.41,0.732262304540659));
#43394=CARTESIAN_POINT('Ctrl Pts',(-2.79703133737243,7.26257643241256,1.50498437334144));
#43395=CARTESIAN_POINT('Ctrl Pts',(-2.51052533147875,6.871296113951,2.51070089780968));
#43396=CARTESIAN_POINT('Ctrl Pts',(-2.38147333747754,6.71484535620929,2.82119365553778));
#43397=CARTESIAN_POINT('Ctrl Pts',(-2.03213201249546,6.38798517315582,3.36454771509492));
#43398=CARTESIAN_POINT('Ctrl Pts',(-1.81218560208282,6.21764548689165,3.59767135677579));
#43399=CARTESIAN_POINT('Ctrl Pts',(-1.33144862194443,5.95819559552318,3.9171419061609));
#43400=CARTESIAN_POINT('Ctrl Pts',(-1.08458290107335,5.85511893191279,4.03129022106372));
#43401=CARTESIAN_POINT('Ctrl Pts',(-0.552196963605975,5.71567698479767,
4.17989549259779));
#43402=CARTESIAN_POINT('Ctrl Pts',(-0.266706680138664,5.68,4.21510379468881));
#43403=CARTESIAN_POINT('Ctrl Pts',(-1.38777878078145E-16,5.68,4.21510379468881));
#43404=CARTESIAN_POINT('Ctrl Pts',(-6.93889390390723E-17,5.68,4.21510379468881));
#43405=CARTESIAN_POINT('Ctrl Pts',(0.266706680138664,5.68,4.21510379468881));
#43406=CARTESIAN_POINT('Ctrl Pts',(0.552196963605975,5.71567698479767,4.17989549259779));
#43407=CARTESIAN_POINT('Ctrl Pts',(1.08458290107335,5.85511893191279,4.03129022106372));
#43408=CARTESIAN_POINT('Ctrl Pts',(1.33144862194444,5.95819559552317,3.9171419061609));
#43409=CARTESIAN_POINT('Ctrl Pts',(1.81218560208282,6.21764548689165,3.59767135677579));
#43410=CARTESIAN_POINT('Ctrl Pts',(2.03213201249546,6.38798517315582,3.36454771509492));
#43411=CARTESIAN_POINT('Ctrl Pts',(2.38147333747754,6.71484535620929,2.82119365553778));
#43412=CARTESIAN_POINT('Ctrl Pts',(2.51052533147875,6.871296113951,2.51070089780968));
#43413=CARTESIAN_POINT('Ctrl Pts',(2.79703133737243,7.26257643241256,1.50498437334144));
#43414=CARTESIAN_POINT('Ctrl Pts',(2.86057686489981,7.41,0.73226230454066));
#43415=CARTESIAN_POINT('Ctrl Pts',(2.86057686489981,7.41,-0.73226230454066));
#43416=CARTESIAN_POINT('Ctrl Pts',(2.79703133737243,7.26257643241256,-1.50498437334144));
#43417=CARTESIAN_POINT('Ctrl Pts',(2.51052533147875,6.871296113951,-2.51070089780968));
#43418=CARTESIAN_POINT('Ctrl Pts',(2.38147333747754,6.71484535620929,-2.82119365553778));
#43419=CARTESIAN_POINT('Ctrl Pts',(2.03213201249546,6.38798517315582,-3.36454771509492));
#43420=CARTESIAN_POINT('Ctrl Pts',(1.81218560208282,6.21764548689165,-3.59767135677579));
#43421=CARTESIAN_POINT('Ctrl Pts',(1.33144862194444,5.95819559552317,-3.9171419061609));
#43422=CARTESIAN_POINT('Ctrl Pts',(1.08458290107335,5.85511893191279,-4.03129022106372));
#43423=CARTESIAN_POINT('Ctrl Pts',(0.552196963605975,5.71567698479767,-4.17989549259779));
#43424=CARTESIAN_POINT('Ctrl Pts',(0.266706680138664,5.68,-4.21510379468881));
#43425=CARTESIAN_POINT('Ctrl Pts',(0.,5.68,-4.21510379468881));
#43426=CARTESIAN_POINT('Origin',(4.25,0.,0.));
#43427=CARTESIAN_POINT('',(4.25,1.41,-6.75));
#43428=CARTESIAN_POINT('Origin',(4.25,1.41,0.));
#43429=CARTESIAN_POINT('Origin',(5.25,1.41,0.));
#43430=CARTESIAN_POINT('',(5.25,1.41,-6.75));
#43431=CARTESIAN_POINT('',(5.25,1.41,-6.75));
#43432=CARTESIAN_POINT('Origin',(5.25,1.41,0.));
#43433=CARTESIAN_POINT('Origin',(5.25,0.,0.));
#43434=CARTESIAN_POINT('',(5.24999993301406,7.94670116372702,-7.968642341825));
#43435=CARTESIAN_POINT('',(5.25000007836621,3.63834712397532,-7.50000017632907));
#43436=CARTESIAN_POINT('Ctrl Pts',(5.24999986926046,7.94670116372703,-7.96864234182499));
#43437=CARTESIAN_POINT('Ctrl Pts',(5.24999985979781,7.92042912898641,-7.98057901186823));
#43438=CARTESIAN_POINT('Ctrl Pts',(5.2500000454706,7.89428766094108,-7.99255496414018));
#43439=CARTESIAN_POINT('Ctrl Pts',(5.25000000000006,7.86827447145648,-8.00454117392044));
#43440=CARTESIAN_POINT('Ctrl Pts',(5.24999995731924,7.84385724015657,-8.01579200714822));
#43441=CARTESIAN_POINT('Ctrl Pts',(5.24999970997981,7.81955306918205,-8.0270518445332));
#43442=CARTESIAN_POINT('Ctrl Pts',(5.24999970836727,7.79536070220373,-8.03829312390875));
#43443=CARTESIAN_POINT('Ctrl Pts',(5.24999970656126,7.7682658959929,-8.05088305719287));
#43444=CARTESIAN_POINT('Ctrl Pts',(5.25000003233846,7.74131186309921,-8.06344951879706));
#43445=CARTESIAN_POINT('Ctrl Pts',(5.24999999999984,7.71444580188881,-8.07597690415732));
#43446=CARTESIAN_POINT('Ctrl Pts',(5.24999997270226,7.69176770109085,-8.08655148394815));
#43447=CARTESIAN_POINT('Ctrl Pts',(5.24999969135857,7.66915232604687,-8.09709825967747));
#43448=CARTESIAN_POINT('Ctrl Pts',(5.24999967895586,7.64656997550749,-8.1076038634778));
#43449=CARTESIAN_POINT('Ctrl Pts',(5.24999966354061,7.61850250221676,-8.12066121787298));
#43450=CARTESIAN_POINT('Ctrl Pts',(5.25000012887595,7.59048603449503,-8.13365525534816));
#43451=CARTESIAN_POINT('Ctrl Pts',(5.24999999999693,7.56249376377644,-8.14653794192863));
#43452=CARTESIAN_POINT('Ctrl Pts',(5.24999990234171,7.54128324084016,-8.15629951225435));
#43453=CARTESIAN_POINT('Ctrl Pts',(5.24999945605478,7.52008655804911,-8.16599720495859));
#43454=CARTESIAN_POINT('Ctrl Pts',(5.24999939312249,7.49889424963558,-8.17560645841391));
#43455=CARTESIAN_POINT('Ctrl Pts',(5.24999930603519,7.46956779655631,-8.18890398670037));
#43456=CARTESIAN_POINT('Ctrl Pts',(5.2500001189999,7.44024985607557,-8.20203300835797));
#43457=CARTESIAN_POINT('Ctrl Pts',(5.25000000000006,7.41093053450868,-8.21490731595539));
#43458=CARTESIAN_POINT('Ctrl Pts',(5.249999919518,7.39110126998961,-8.22361447687202));
#43459=CARTESIAN_POINT('Ctrl Pts',(5.24999935941906,7.37127128205611,-8.2322052130014));
#43460=CARTESIAN_POINT('Ctrl Pts',(5.24999921825673,7.35144050969113,-8.24065001429036));
#43461=CARTESIAN_POINT('Ctrl Pts',(5.24999899999811,7.32077909392119,-8.25370697236793));
#43462=CARTESIAN_POINT('Ctrl Pts',(5.25000009769284,7.29011544054891,-8.2664142201975));
#43463=CARTESIAN_POINT('Ctrl Pts',(5.24999999999859,7.25926186112955,-8.27871443681296));
#43464=CARTESIAN_POINT('Ctrl Pts',(5.24999994108235,7.24065506580565,-8.28613229941791));
#43465=CARTESIAN_POINT('Ctrl Pts',(5.24999934539331,7.22197913505664,-8.29340201010748));
#43466=CARTESIAN_POINT('Ctrl Pts',(5.24999915223788,7.20319642441607,-8.30050607557604));
#43467=CARTESIAN_POINT('Ctrl Pts',(5.24999884945851,7.17375372543655,-8.311642000796));
#43468=CARTESIAN_POINT('Ctrl Pts',(5.24999986612592,7.14404673713778,-8.32236961302399));
#43469=CARTESIAN_POINT('Ctrl Pts',(5.25000000790818,7.11368476804691,-8.33262088189463));
#43470=CARTESIAN_POINT('Ctrl Pts',(5.25000002226541,7.11061023868215,-8.33365895116722));
#43471=CARTESIAN_POINT('Ctrl Pts',(5.25000002173508,7.10752899840853,-8.33469209178922));
#43472=CARTESIAN_POINT('Ctrl Pts',(5.24999999999137,7.10444064568076,-8.33572020146925));
#43473=CARTESIAN_POINT('Ctrl Pts',(5.24999987233545,7.08630912824145,-8.34175616634638));
#43474=CARTESIAN_POINT('Ctrl Pts',(5.24999909769908,7.06793226520206,-8.34761949565941));
#43475=CARTESIAN_POINT('Ctrl Pts',(5.24999869097741,7.04923006893192,-8.35328916894757));
#43476=CARTESIAN_POINT('Ctrl Pts',(5.2499981544592,7.02455946657296,-8.36076819724869));
#43477=CARTESIAN_POINT('Ctrl Pts',(5.24999833662105,6.9993222943843,-8.36790723392353));
#43478=CARTESIAN_POINT('Ctrl Pts',(5.24999902610826,6.97331790178632,-8.37455580386236));
#43479=CARTESIAN_POINT('Ctrl Pts',(5.2499993431706,6.96135971981733,-8.37761316460872));
#43480=CARTESIAN_POINT('Ctrl Pts',(5.2499997293887,6.94923965184436,-8.38056625895871));
#43481=CARTESIAN_POINT('Ctrl Pts',(5.24999999992171,6.93694040179796,-8.38339734176588));
#43482=CARTESIAN_POINT('Ctrl Pts',(5.25000041319619,6.91815169250354,-8.38772219016327));
#43483=CARTESIAN_POINT('Ctrl Pts',(5.25000053414591,6.89894432415434,-8.39176277132838));
#43484=CARTESIAN_POINT('Ctrl Pts',(5.25000026927922,6.87924414025345,-8.39546034664865));
#43485=CARTESIAN_POINT('Ctrl Pts',(5.24999994432396,6.85507470427821,-8.39999676673572));
#43486=CARTESIAN_POINT('Ctrl Pts',(5.24999885106252,6.83018347199435,-8.4040151695677));
#43487=CARTESIAN_POINT('Ctrl Pts',(5.24999821940173,6.80454227883525,-8.40730778596991));
#43488=CARTESIAN_POINT('Ctrl Pts',(5.24999773730235,6.78497227616416,-8.40982079351158));
#43489=CARTESIAN_POINT('Ctrl Pts',(5.24999748527141,6.76496617478289,-8.41191057336018));
#43490=CARTESIAN_POINT('Ctrl Pts',(5.24999999607386,6.74453137954786,-8.41347976073673));
#43491=CARTESIAN_POINT('Ctrl Pts',(5.25000244927413,6.72456539410548,-8.4150129482219));
#43492=CARTESIAN_POINT('Ctrl Pts',(5.25000757949653,6.70419049199182,-8.41604885591512));
#43493=CARTESIAN_POINT('Ctrl Pts',(5.25001115564682,6.68341009717958,-8.41649761277241));
#43494=CARTESIAN_POINT('Ctrl Pts',(5.25001634209877,6.65327251609463,-8.41714843997256));
#43495=CARTESIAN_POINT('Ctrl Pts',(5.25001736124167,6.62227681778639,-8.41658575378721));
#43496=CARTESIAN_POINT('Ctrl Pts',(5.25001258721293,6.59061762597165,-8.41468583292122));
#43497=CARTESIAN_POINT('Ctrl Pts',(5.25000925802606,6.56853996969574,-8.4133609159721));
#43498=CARTESIAN_POINT('Ctrl Pts',(5.25000338360853,6.54614003683157,-8.41138640934763));
#43499=CARTESIAN_POINT('Ctrl Pts',(5.24999999458578,6.52347485149968,-8.40873179385859));
#43500=CARTESIAN_POINT('Ctrl Pts',(5.24999696928664,6.50324218541125,-8.40636208242688));
#43501=CARTESIAN_POINT('Ctrl Pts',(5.24999616463599,6.48279758957839,-8.40345058898327));
#43502=CARTESIAN_POINT('Ctrl Pts',(5.24999607720379,6.46220567247638,-8.39999184752192));
#43503=CARTESIAN_POINT('Ctrl Pts',(5.24999595356056,6.43308537815003,-8.39510062885324));
#43504=CARTESIAN_POINT('Ctrl Pts',(5.24999734419153,6.40362599126612,-8.38909780036147));
#43505=CARTESIAN_POINT('Ctrl Pts',(5.2499986539087,6.37396006149583,-8.38210528187685));
#43506=CARTESIAN_POINT('Ctrl Pts',(5.24999989231947,6.34590926717141,-8.37549346490901));
#43507=CARTESIAN_POINT('Ctrl Pts',(5.25000136507078,6.31767342551847,-8.36799762707938));
#43508=CARTESIAN_POINT('Ctrl Pts',(5.25000022613449,6.28931191598885,-8.35972094746712));
#43509=CARTESIAN_POINT('Ctrl Pts',(5.25000016055573,6.28767888988593,-8.35924438489776));
#43510=CARTESIAN_POINT('Ctrl Pts',(5.25000008515903,6.28604543293954,-8.35876523173905));
#43511=CARTESIAN_POINT('Ctrl Pts',(5.24999999892296,6.28441155129405,-8.35828350689833));
#43512=CARTESIAN_POINT('Ctrl Pts',(5.24999899277608,6.26534847426058,-8.35266305221421));
#43513=CARTESIAN_POINT('Ctrl Pts',(5.24999656259104,6.24622792118924,-8.34669240771587));
#43514=CARTESIAN_POINT('Ctrl Pts',(5.2499944902779,6.22707173109384,-8.34041729961635));
#43515=CARTESIAN_POINT('Ctrl Pts',(5.24998960195341,6.18188470255591,-8.32561511362009));
#43516=CARTESIAN_POINT('Ctrl Pts',(5.249989597612,6.13651203359492,-8.30906928328382));
#43517=CARTESIAN_POINT('Ctrl Pts',(5.24999486284137,6.09091967408837,-8.29121673089798));
#43518=CARTESIAN_POINT('Ctrl Pts',(5.24999686514397,6.07358145499244,-8.28442762263429));
#43519=CARTESIAN_POINT('Ctrl Pts',(5.24999919861929,6.05621110809025,-8.27744938914288));
#43520=CARTESIAN_POINT('Ctrl Pts',(5.24999999958938,6.03880643800309,-8.2703055376079));
#43521=CARTESIAN_POINT('Ctrl Pts',(5.25000079658244,6.0214881870133,-8.26319715731128));
#43522=CARTESIAN_POINT('Ctrl Pts',(5.25000001560539,6.00413601494501,-8.25592473803094));
#43523=CARTESIAN_POINT('Ctrl Pts',(5.24999898541405,5.98674097435617,-8.24850965134291));
#43524=CARTESIAN_POINT('Ctrl Pts',(5.2499964517624,5.94395962734543,-8.23027299388325));
#43525=CARTESIAN_POINT('Ctrl Pts',(5.24999411548082,5.90094906844815,-8.21118434813899));
#43526=CARTESIAN_POINT('Ctrl Pts',(5.24999628257442,5.85773628457346,-8.19153407956133));
#43527=CARTESIAN_POINT('Ctrl Pts',(5.24999744061961,5.83464436243185,-8.18103342601924));
#43528=CARTESIAN_POINT('Ctrl Pts',(5.24999948052378,5.81149511755054,-8.1703729347153));
#43529=CARTESIAN_POINT('Ctrl Pts',(5.2499999999919,5.78829678611397,-8.15960055110763));
#43530=CARTESIAN_POINT('Ctrl Pts',(5.25000034546962,5.77286849277986,-8.15243626454413));
#43531=CARTESIAN_POINT('Ctrl Pts',(5.24999995290227,5.75741859124791,-8.14522255069958));
#43532=CARTESIAN_POINT('Ctrl Pts',(5.24999940442921,5.74194736020579,-8.13797052346545));
#43533=CARTESIAN_POINT('Ctrl Pts',(5.24999775717843,5.69548200164799,-8.11619022396715));
#43534=CARTESIAN_POINT('Ctrl Pts',(5.24999615656465,5.64883593126901,-8.09407626703666));
#43535=CARTESIAN_POINT('Ctrl Pts',(5.24999770219945,5.60220799517453,-8.07196864924727));
#43536=CARTESIAN_POINT('Ctrl Pts',(5.24999845313466,5.57955415791413,-8.06122782695136));
#43537=CARTESIAN_POINT('Ctrl Pts',(5.24999964840422,5.55690524771809,-8.05048886902695));
#43538=CARTESIAN_POINT('Ctrl Pts',(5.24999999999646,5.5342879683987,-8.03979216915111));
#43539=CARTESIAN_POINT('Ctrl Pts',(5.25000020599498,5.52103646411359,-8.03352495361915));
#43540=CARTESIAN_POINT('Ctrl Pts',(5.25000009968989,5.50779587343064,-8.02727225737731));
#43541=CARTESIAN_POINT('Ctrl Pts',(5.24999989787751,5.49457103649227,-8.02104089797295));
#43542=CARTESIAN_POINT('Ctrl Pts',(5.24999902774336,5.43755083513988,-7.99417377139956));
#43543=CARTESIAN_POINT('Ctrl Pts',(5.24999833607258,5.38082137601284,-7.96771614392102));
#43544=CARTESIAN_POINT('Ctrl Pts',(5.24999941548658,5.32413575082117,-7.94183310567151));
#43545=CARTESIAN_POINT('Ctrl Pts',(5.24999968327137,5.31007298348315,-7.93541195138993));
#43546=CARTESIAN_POINT('Ctrl Pts',(5.24999994395975,5.29601313071909,-7.92902622523739));
#43547=CARTESIAN_POINT('Ctrl Pts',(5.24999999998534,5.28195281698071,-7.92267859721573));
#43548=CARTESIAN_POINT('Ctrl Pts',(5.25000004390683,5.27093017428062,-7.9177023472559));
#43549=CARTESIAN_POINT('Ctrl Pts',(5.24999995980601,5.25990725211983,-7.91274951373632));
#43550=CARTESIAN_POINT('Ctrl Pts',(5.24999982929753,5.24888230738315,-7.90782095774229));
#43551=CARTESIAN_POINT('Ctrl Pts',(5.2499993030909,5.20443003061332,-7.887949154268));
#43552=CARTESIAN_POINT('Ctrl Pts',(5.24999849170788,5.15993871607658,-7.86848537238923));
#43553=CARTESIAN_POINT('Ctrl Pts',(5.24999892117554,5.11486500000911,-7.84930144838585));
#43554=CARTESIAN_POINT('Ctrl Pts',(5.24999919587201,5.08603491199674,-7.83703101085165));
#43555=CARTESIAN_POINT('Ctrl Pts',(5.24999986607924,5.05696627771669,-7.8248756934888));
#43556=CARTESIAN_POINT('Ctrl Pts',(5.24999999999432,5.02751255560357,-7.81281258125108));
#43557=CARTESIAN_POINT('Ctrl Pts',(5.25000004186963,5.01830236391083,-7.80904044081688));
#43558=CARTESIAN_POINT('Ctrl Pts',(5.2500000224096,5.00905448794408,-7.80527739227639));
#43559=CARTESIAN_POINT('Ctrl Pts',(5.24999997176832,4.99976434331729,-7.80152284206514));
#43560=CARTESIAN_POINT('Ctrl Pts',(5.24999975764146,4.9604827571553,-7.78564745007203));
#43561=CARTESIAN_POINT('Ctrl Pts',(5.2499991504668,4.92044535873102,-7.76992996410811));
#43562=CARTESIAN_POINT('Ctrl Pts',(5.24999920773422,4.87931378761042,-7.75436286495623));
#43563=CARTESIAN_POINT('Ctrl Pts',(5.24999926490981,4.83824817735725,-7.73882073006745));
#43564=CARTESIAN_POINT('Ctrl Pts',(5.25000006250811,4.79609208646318,-7.72342743327411));
#43565=CARTESIAN_POINT('Ctrl Pts',(5.249999999991,4.75249331950356,-7.7082247363706));
#43566=CARTESIAN_POINT('Ctrl Pts',(5.24999998891567,4.74476950044821,-7.70553147488123));
#43567=CARTESIAN_POINT('Ctrl Pts',(5.24999994182541,4.73700036006587,-7.70284434575642));
#43568=CARTESIAN_POINT('Ctrl Pts',(5.24999987261493,4.72918391457014,-7.7001637385431));
#43569=CARTESIAN_POINT('Ctrl Pts',(5.24999946999015,4.68371255323638,-7.68456958398051));
#43570=CARTESIAN_POINT('Ctrl Pts',(5.24999850571767,4.63664612843812,-7.66919091579023));
#43571=CARTESIAN_POINT('Ctrl Pts',(5.2499985244879,4.58787344246801,-7.65423058086207));
#43572=CARTESIAN_POINT('Ctrl Pts',(5.24999854325813,4.53910075649789,-7.63927024593392));
#43573=CARTESIAN_POINT('Ctrl Pts',(5.24999969153135,4.48862171261842,-7.62472744726044));
#43574=CARTESIAN_POINT('Ctrl Pts',(5.24999999999003,4.43632478576696,-7.61086130246294));
#43575=CARTESIAN_POINT('Ctrl Pts',(5.25000003518208,4.43035823099177,-7.60927931442968));
#43576=CARTESIAN_POINT('Ctrl Pts',(5.25000005411519,4.42436801418822,-7.60770620227508));
#43577=CARTESIAN_POINT('Ctrl Pts',(5.25000006066451,4.41835398312687,-7.60614239344774));
#43578=CARTESIAN_POINT('Ctrl Pts',(5.25000010971638,4.37331122899801,-7.59443007340888));
#43579=CARTESIAN_POINT('Ctrl Pts',(5.24999955774809,4.32693296153263,-7.5832489428317));
#43580=CARTESIAN_POINT('Ctrl Pts',(5.24999945792033,4.27908779984327,-7.57278693404784));
#43581=CARTESIAN_POINT('Ctrl Pts',(5.24999936403813,4.23409220879664,-7.56294802344239));
#43582=CARTESIAN_POINT('Ctrl Pts',(5.24999971534387,4.18779916246661,-7.55374493379632));
#43583=CARTESIAN_POINT('Ctrl Pts',(5.24999998994999,4.14010088266014,-7.54537978049226));
#43584=CARTESIAN_POINT('Ctrl Pts',(5.2500001263197,4.11641386353316,-7.54122563600073));
#43585=CARTESIAN_POINT('Ctrl Pts',(5.25000021765403,4.09238032773424,-7.53727888386729));
#43586=CARTESIAN_POINT('Ctrl Pts',(5.2499999999999,4.06798733192949,-7.53356914073385));
#43587=CARTESIAN_POINT('Ctrl Pts',(5.24999996894701,4.06450716288216,-7.53303986858828));
#43588=CARTESIAN_POINT('Ctrl Pts',(5.24999993132666,4.06101967736794,-7.53251542663155));
#43589=CARTESIAN_POINT('Ctrl Pts',(5.24999988805877,4.05752485198541,-7.53199590138679));
#43590=CARTESIAN_POINT('Ctrl Pts',(5.24999929308391,4.00946766391712,-7.5248519329017));
#43591=CARTESIAN_POINT('Ctrl Pts',(5.24999772967613,3.96003396915788,-7.51863731311267));
#43592=CARTESIAN_POINT('Ctrl Pts',(5.24999701437125,3.9092284710242,-7.51362111328977));
#43593=CARTESIAN_POINT('Ctrl Pts',(5.24999633485654,3.86096501835613,-7.50885589827132));
#43594=CARTESIAN_POINT('Ctrl Pts',(5.24999647268159,3.81146348065842,-7.50517209025358));
#43595=CARTESIAN_POINT('Ctrl Pts',(5.24999744301681,3.76075092647382,-7.50284022076318));
#43596=CARTESIAN_POINT('Ctrl Pts',(5.2499982094219,3.72069635688742,-7.50099842773439));
#43597=CARTESIAN_POINT('Ctrl Pts',(5.24999948018792,3.67988668822894,-7.50000070445283));
#43598=CARTESIAN_POINT('Ctrl Pts',(5.25000017632343,3.63834712397696,-7.50000017632941));
#43599=CARTESIAN_POINT('',(5.25,10.41979065301,-7.968642341825));
#43600=CARTESIAN_POINT('',(5.25,10.41979065301,-7.968642341825));
#43601=CARTESIAN_POINT('',(5.24999999999988,10.4571163879047,-7.96641903838753));
#43602=CARTESIAN_POINT('Ctrl Pts',(5.24999999999953,10.45711625936,-7.966419053641));
#43603=CARTESIAN_POINT('Ctrl Pts',(5.24999999999953,10.45297744471,-7.96691054287));
#43604=CARTESIAN_POINT('Ctrl Pts',(5.24999999999955,10.448836167275,-7.9673236221365));
#43605=CARTESIAN_POINT('Ctrl Pts',(5.24999999999956,10.4446918747092,-7.96765338841725));
#43606=CARTESIAN_POINT('Ctrl Pts',(5.24999999999957,10.4405475821433,-7.967983154698));
#43607=CARTESIAN_POINT('Ctrl Pts',(5.24999999999957,10.4364002744467,-7.968229607993));
#43608=CARTESIAN_POINT('Ctrl Pts',(5.24999999999958,10.4322500589158,-7.9683944361125));
#43609=CARTESIAN_POINT('Ctrl Pts',(5.24999999999958,10.428099843385,-7.96855926423199));
#43610=CARTESIAN_POINT('Ctrl Pts',(5.24999999999958,10.42394672002,-7.968642467176));
#43611=CARTESIAN_POINT('Ctrl Pts',(5.24999999999958,10.41979065301,-7.968642341825));
#43612=CARTESIAN_POINT('',(5.24999999999997,12.1609694417917,-7.72257626142715));
#43613=CARTESIAN_POINT('Ctrl Pts',(5.25,12.1609694417906,-7.72257626142175));
#43614=CARTESIAN_POINT('Ctrl Pts',(5.25,12.0834979181545,-7.73841082136219));
#43615=CARTESIAN_POINT('Ctrl Pts',(5.25,11.9234509679755,-7.76813457545424));
#43616=CARTESIAN_POINT('Ctrl Pts',(5.25,11.67408343811,-7.808462753035));
#43617=CARTESIAN_POINT('Ctrl Pts',(5.25,11.39910660014,-7.848332324994));
#43618=CARTESIAN_POINT('Ctrl Pts',(5.25,11.09804785384,-7.888268548859));
#43619=CARTESIAN_POINT('Ctrl Pts',(5.25,10.7798535275883,-7.9278253552661));
#43620=CARTESIAN_POINT('Ctrl Pts',(5.25,10.5655600593217,-7.95355186396394));
#43621=CARTESIAN_POINT('Ctrl Pts',(5.25,10.4571163879049,-7.96641903838876));
#43622=CARTESIAN_POINT('',(5.25,12.4099999863643,-7.6583523942248));
#43623=CARTESIAN_POINT('Ctrl Pts',(5.25,12.4099999860592,-7.65835239311871));
#43624=CARTESIAN_POINT('Ctrl Pts',(5.25,12.3926880098894,-7.66312722015755));
#43625=CARTESIAN_POINT('Ctrl Pts',(5.25,12.3587824122134,-7.6725047316683));
#43626=CARTESIAN_POINT('Ctrl Pts',(5.25,12.31026017487,-7.68580697919));
#43627=CARTESIAN_POINT('Ctrl Pts',(5.25,12.26332802492,-7.698354350369));
#43628=CARTESIAN_POINT('Ctrl Pts',(5.25,12.21488327627,-7.710652709337));
#43629=CARTESIAN_POINT('Ctrl Pts',(5.25,12.1793923623,-7.718809498598));
#43630=CARTESIAN_POINT('Ctrl Pts',(5.25,12.16096980378,-7.722576187434));
#43631=CARTESIAN_POINT('',(5.25,12.40999999936,7.5));
#43632=CARTESIAN_POINT('',(5.25,12.40999999936,7.5));
#43633=CARTESIAN_POINT('',(5.25,1.41,7.5));
#43634=CARTESIAN_POINT('',(5.25,1.41,7.5));
#43635=CARTESIAN_POINT('',(5.25,0.04746907580983,7.375195555416));
#43636=CARTESIAN_POINT('Origin',(5.25,1.41,0.));
#43637=CARTESIAN_POINT('',(5.25,-0.975037109157,7.551196560962));
#43638=CARTESIAN_POINT('Origin',(5.25,-0.2250371090282,8.850234666499));
#43639=CARTESIAN_POINT('',(5.25,-5.118174593052,9.943238102513));
#43640=CARTESIAN_POINT('',(5.25,-5.118174593052,9.943238102513));
#43641=CARTESIAN_POINT('',(5.25,-8.533238102513,6.528174593052));
#43642=CARTESIAN_POINT('Origin',(5.25,-6.368174593052,7.778174593052));
#43643=CARTESIAN_POINT('',(5.25,-6.141196560822,2.385037109028));
#43644=CARTESIAN_POINT('',(5.25,-6.141196560967,2.385037109161));
#43645=CARTESIAN_POINT('',(5.25,-5.965195555416,1.36253092419));
#43646=CARTESIAN_POINT('Origin',(5.25,-7.440234666499,1.635037109028));
#43647=CARTESIAN_POINT('',(5.25,1.41,-7.5));
#43648=CARTESIAN_POINT('Origin',(5.25,1.41,0.));
#43649=CARTESIAN_POINT('',(5.250000058775,3.638347091316,-7.500000176329));
#43650=CARTESIAN_POINT('',(5.25,-6.368174593052,9.028174593052));
#43651=CARTESIAN_POINT('Origin',(5.25,-6.368174593052,7.778174593052));
#43652=CARTESIAN_POINT('Origin',(5.25,-6.368174593052,7.778174593052));
#43653=CARTESIAN_POINT('',(2.75,-6.368174593052,9.028174593052));
#43654=CARTESIAN_POINT('Origin',(2.75,-6.368174593052,7.778174593052));
#43655=CARTESIAN_POINT('',(5.25,-6.368174593052,9.028174593052));
#43656=CARTESIAN_POINT('Origin',(2.75,0.,0.));
#43657=CARTESIAN_POINT('',(2.75,-5.118174593052,9.943238102513));
#43658=CARTESIAN_POINT('',(2.75000000024287,-2.18603093399766,8.25036791856334));
#43659=CARTESIAN_POINT('',(2.75,-5.118174593052,9.943238102513));
#43660=CARTESIAN_POINT('',(2.74999999998423,-6.84036777526504,3.59603441391076));
#43661=CARTESIAN_POINT('Origin',(2.75,1.41,0.));
#43662=CARTESIAN_POINT('',(2.75,-8.533238102513,6.528174593052));
#43663=CARTESIAN_POINT('',(2.749999999978,-6.840370038804,3.596038711084));
#43664=CARTESIAN_POINT('Origin',(2.75,-6.368174593052,7.778174593052));
#43665=CARTESIAN_POINT('Origin',(3.25,-5.196644207287,9.988542555415));
#43666=CARTESIAN_POINT('',(3.25,-4.868174593052,10.37625080441));
#43667=CARTESIAN_POINT('Origin',(3.25,-5.118174593052,9.943238102513));
#43668=CARTESIAN_POINT('',(3.25,-0.7250371090282,7.984209262715));
#43669=CARTESIAN_POINT('',(3.25,-0.7250371090282,7.984209262715));
#43670=CARTESIAN_POINT('Ctrl Pts',(2.75000000080443,-2.18603081191096,8.25036913644901));
#43671=CARTESIAN_POINT('Ctrl Pts',(2.75000000143807,-2.18599696924301,8.2503657438976));
#43672=CARTESIAN_POINT('Ctrl Pts',(2.75000000265658,-2.18596312714159,8.25036235117153));
#43673=CARTESIAN_POINT('Ctrl Pts',(2.75000000445985,-2.18592928560675,8.25035895827084));
#43674=CARTESIAN_POINT('Ctrl Pts',(2.75000203206361,-2.14787778318541,8.24654397264854));
#43675=CARTESIAN_POINT('Ctrl Pts',(2.75074081561521,-2.11054605849314,8.24250971552603));
#43676=CARTESIAN_POINT('Ctrl Pts',(2.75208237772229,-2.07396390256443,8.23830837253815));
#43677=CARTESIAN_POINT('Ctrl Pts',(2.75351653681867,-2.03485678153477,8.23381704542679));
#43678=CARTESIAN_POINT('Ctrl Pts',(2.75563957979403,-1.99660590053698,8.22913468870886));
#43679=CARTESIAN_POINT('Ctrl Pts',(2.75832257441735,-1.9592033183985,8.22430523024947));
#43680=CARTESIAN_POINT('Ctrl Pts',(2.75919641252517,-1.94702148198355,8.22273229946338));
#43681=CARTESIAN_POINT('Ctrl Pts',(2.76012990642584,-1.93492932457007,8.22114362203655));
#43682=CARTESIAN_POINT('Ctrl Pts',(2.76111931513426,-1.92292575588343,8.21954032745987));
#43683=CARTESIAN_POINT('Ctrl Pts',(2.76180768008298,-1.91457446902568,8.21842486144499));
#43684=CARTESIAN_POINT('Ctrl Pts',(2.76252312304503,-1.90626632766312,8.21730248881821));
#43685=CARTESIAN_POINT('Ctrl Pts',(2.76326437045243,-1.89800218029635,8.2161738191947));
#43686=CARTESIAN_POINT('Ctrl Pts',(2.76730004426291,-1.85300856175418,8.21002885005913));
#43687=CARTESIAN_POINT('Ctrl Pts',(2.77209848480575,-1.80932259995566,8.20369889117441));
#43688=CARTESIAN_POINT('Ctrl Pts',(2.77749540077863,-1.76700707275716,8.19727271673768));
#43689=CARTESIAN_POINT('Ctrl Pts',(2.78100267390783,-1.73950764303895,8.19309656334957));
#43690=CARTESIAN_POINT('Ctrl Pts',(2.78476326022402,-1.71258601065174,8.188879337019));
#43691=CARTESIAN_POINT('Ctrl Pts',(2.78873776548973,-1.68625022687806,8.18464108598879));
#43692=CARTESIAN_POINT('Ctrl Pts',(2.79098335513103,-1.6713705477019,8.18224648037767));
#43693=CARTESIAN_POINT('Ctrl Pts',(2.79329729900393,-1.65667891831125,8.17984575545618));
#43694=CARTESIAN_POINT('Ctrl Pts',(2.79567328788736,-1.64217445308732,8.17744174943354));
#43695=CARTESIAN_POINT('Ctrl Pts',(2.80255749831722,-1.60014909199633,8.17047636190586));
#43696=CARTESIAN_POINT('Ctrl Pts',(2.80996108154947,-1.5596983374674,8.16348535455907));
#43697=CARTESIAN_POINT('Ctrl Pts',(2.81777158248429,-1.52080586459298,8.15653879339027));
#43698=CARTESIAN_POINT('Ctrl Pts',(2.82072673602345,-1.50609064596347,8.15391051704867));
#43699=CARTESIAN_POINT('Ctrl Pts',(2.82374036182381,-1.49159805648715,8.15128834736281));
#43700=CARTESIAN_POINT('Ctrl Pts',(2.8268071518979,-1.4773257415543,8.14867521058651));
#43701=CARTESIAN_POINT('Ctrl Pts',(2.83100504743873,-1.45778945580721,8.1450982865207));
#43702=CARTESIAN_POINT('Ctrl Pts',(2.83530229236517,-1.43866881913031,8.14153963541655));
#43703=CARTESIAN_POINT('Ctrl Pts',(2.83968716971298,-1.41995266321184,8.13800479351629));
#43704=CARTESIAN_POINT('Ctrl Pts',(2.84875078533761,-1.38126605244481,8.13069821553552));
#43705=CARTESIAN_POINT('Ctrl Pts',(2.85818770414255,-1.34431059448287,8.12349512669871));
#43706=CARTESIAN_POINT('Ctrl Pts',(2.86793215029481,-1.30901006276093,8.11644243981932));
#43707=CARTESIAN_POINT('Ctrl Pts',(2.8691616724745,-1.30455595772217,8.11555255497526));
#43708=CARTESIAN_POINT('Ctrl Pts',(2.87039611681958,-1.30012814775789,8.11466503148957));
#43709=CARTESIAN_POINT('Ctrl Pts',(2.87163537382243,-1.29572643767609,8.11377993626792));
#43710=CARTESIAN_POINT('Ctrl Pts',(2.87795924690619,-1.27326470790997,8.10926333492064));
#43711=CARTESIAN_POINT('Ctrl Pts',(2.884407574416,-1.25148815620034,8.10481226298927));
#43712=CARTESIAN_POINT('Ctrl Pts',(2.89096401354338,-1.2303795899674,8.1004364144946));
#43713=CARTESIAN_POINT('Ctrl Pts',(2.90080152733586,-1.1987075485709,8.09387073622263));
#43714=CARTESIAN_POINT('Ctrl Pts',(2.91088218359936,-1.16854172400716,8.08747545772209));
#43715=CARTESIAN_POINT('Ctrl Pts',(2.92117058635112,-1.13986277581381,8.08128868142044));
#43716=CARTESIAN_POINT('Ctrl Pts',(2.92974409568673,-1.1159640972722,8.07613313049));
#43717=CARTESIAN_POINT('Ctrl Pts',(2.93846080868979,-1.0931011345692,8.07112280556824));
#43718=CARTESIAN_POINT('Ctrl Pts',(2.94729604479062,-1.07126537440902,8.0662759237153));
#43719=CARTESIAN_POINT('Ctrl Pts',(2.95612955847588,-1.04943387109639,8.06142998675445));
#43720=CARTESIAN_POINT('Ctrl Pts',(2.96508155460103,-1.02862989400395,8.05674762477974));
#43721=CARTESIAN_POINT('Ctrl Pts',(2.97413022110453,-1.00887086876362,8.0522521809041));
#43722=CARTESIAN_POINT('Ctrl Pts',(2.98499562424733,-0.985144745708707,
8.04685416894336));
#43723=CARTESIAN_POINT('Ctrl Pts',(2.99599912932157,-0.962923457993005,
8.04172374290186));
#43724=CARTESIAN_POINT('Ctrl Pts',(3.0071077955465,-0.942199653336915,8.03688739802855));
#43725=CARTESIAN_POINT('Ctrl Pts',(3.0145034433413,-0.928402681036047,8.03366757824343));
#43726=CARTESIAN_POINT('Ctrl Pts',(3.02194572611609,-0.915268968712097,
8.03057785708498));
#43727=CARTESIAN_POINT('Ctrl Pts',(3.02942256884002,-0.902808977924984,
8.02762852891565));
#43728=CARTESIAN_POINT('Ctrl Pts',(3.04183447358211,-0.882124816916487,
8.02273250774167));
#43729=CARTESIAN_POINT('Ctrl Pts',(3.05434262452836,-0.863287067001056,
8.0182183319781));
#43730=CARTESIAN_POINT('Ctrl Pts',(3.06691280320266,-0.846284631151253,
8.01411257827712));
#43731=CARTESIAN_POINT('Ctrl Pts',(3.06760370501054,-0.845350116696736,
8.01388691142479));
#43732=CARTESIAN_POINT('Ctrl Pts',(3.06829479751297,-0.844421135571319,
8.01366247350665));
#43733=CARTESIAN_POINT('Ctrl Pts',(3.06898607616024,-0.843497682288813,
8.01343926730765));
#43734=CARTESIAN_POINT('Ctrl Pts',(3.07467411818084,-0.83589923975678,8.01160266170126));
#43735=CARTESIAN_POINT('Ctrl Pts',(3.0803746756442,-0.8286752304301,8.00984951854266));
#43736=CARTESIAN_POINT('Ctrl Pts',(3.08608187232844,-0.821827182093947,
8.00818252582984));
#43737=CARTESIAN_POINT('Ctrl Pts',(3.09708026754574,-0.808630240366617,
8.00497004767386));
#43738=CARTESIAN_POINT('Ctrl Pts',(3.10810885215689,-0.796817347737043,
8.00207175608596));
#43739=CARTESIAN_POINT('Ctrl Pts',(3.11909757641733,-0.786412036999781,
7.99950664885367));
#43740=CARTESIAN_POINT('Ctrl Pts',(3.12331828887664,-0.782415410673481,
7.99852140436139));
#43741=CARTESIAN_POINT('Ctrl Pts',(3.1275331906934,-0.778625917010289,7.99758515267624));
#43742=CARTESIAN_POINT('Ctrl Pts',(3.13173857046868,-0.77504297073421,7.99669838060771));
#43743=CARTESIAN_POINT('Ctrl Pts',(3.13551881815513,-0.771822233227817,
7.9959012544884));
#43744=CARTESIAN_POINT('Ctrl Pts',(3.13929136238273,-0.768768372415048,
7.99514410309805));
#43745=CARTESIAN_POINT('Ctrl Pts',(3.14305240612772,-0.765879628621723,
7.99442685358692));
#43746=CARTESIAN_POINT('Ctrl Pts',(3.15459054621756,-0.757017532663539,
7.99222647361269));
#43747=CARTESIAN_POINT('Ctrl Pts',(3.16602850201771,-0.749717434211676,
7.99040763809797));
#43748=CARTESIAN_POINT('Ctrl Pts',(3.1772685852345,-0.743883488159329,7.98894871026817));
#43749=CARTESIAN_POINT('Ctrl Pts',(3.18253941430561,-0.741147767092236,
7.98826457305409));
#43750=CARTESIAN_POINT('Ctrl Pts',(3.18776708152223,-0.73873377593749,7.98765940185426));
#43751=CARTESIAN_POINT('Ctrl Pts',(3.19294333485885,-0.736628319017608,
7.98713004868365));
#43752=CARTESIAN_POINT('Ctrl Pts',(3.1947510034279,-0.73589304428315,7.98694518619215));
#43753=CARTESIAN_POINT('Ctrl Pts',(3.19655241119166,-0.73519537838123,7.98676956462907));
#43754=CARTESIAN_POINT('Ctrl Pts',(3.19834710830016,-0.73453439781842,7.98660294139632));
#43755=CARTESIAN_POINT('Ctrl Pts',(3.20862886183901,-0.730747664553751,
7.98564836304162));
#43756=CARTESIAN_POINT('Ctrl Pts',(3.21869184518773,-0.728185401026915,
7.985002609133));
#43757=CARTESIAN_POINT('Ctrl Pts',(3.2285270849327,-0.726682175030561,7.98462380996472));
#43758=CARTESIAN_POINT('Ctrl Pts',(3.23580778908085,-0.725569386320671,
7.98434339741277));
#43759=CARTESIAN_POINT('Ctrl Pts',(3.24296430279622,-0.725037924549703,
7.98420952256945));
#43760=CARTESIAN_POINT('Ctrl Pts',(3.25,-0.725037109028451,7.98420926271457));
#43761=CARTESIAN_POINT('Ctrl Pts',(2.748031232229,-2.249001700534,8.299984818872));
#43762=CARTESIAN_POINT('Ctrl Pts',(2.748165300609,-2.234652803614,8.298726087963));
#43763=CARTESIAN_POINT('Ctrl Pts',(2.750023861624,-2.124930155855,8.288701163509));
#43764=CARTESIAN_POINT('Ctrl Pts',(2.764346989763,-1.927188444858,8.26530476129));
#43765=CARTESIAN_POINT('Ctrl Pts',(2.803313967766,-1.669542337486,8.224590429631));
#43766=CARTESIAN_POINT('Ctrl Pts',(2.852280936191,-1.44708336687,8.182172690363));
#43767=CARTESIAN_POINT('Ctrl Pts',(2.906900085727,-1.25819520666,8.141037625298));
#43768=CARTESIAN_POINT('Ctrl Pts',(2.964682486012,-1.101023410635,8.103166220994));
#43769=CARTESIAN_POINT('Ctrl Pts',(3.024021001282,-0.9744663407883,8.070107631206));
#43770=CARTESIAN_POINT('Ctrl Pts',(3.083563542553,-0.8781689679159,8.043241583061));
#43771=CARTESIAN_POINT('Ctrl Pts',(3.141847763167,-0.8121044008003,8.023815916094));
#43772=CARTESIAN_POINT('Ctrl Pts',(3.197244721767,-0.7752791571759,8.012580732793));
#43773=CARTESIAN_POINT('Ctrl Pts',(3.240232902369,-0.7659855665842,8.009696653886));
#43774=CARTESIAN_POINT('Ctrl Pts',(3.264295855207,-0.7681844468823,8.010377190337));
#43775=CARTESIAN_POINT('Ctrl Pts',(3.271420796559,-0.76950533233,8.010782594487));
#43776=CARTESIAN_POINT('Ctrl Pts',(2.792765104092,-1.991224869763,7.723406537252));
#43777=CARTESIAN_POINT('Ctrl Pts',(2.788537105428,-1.978678815405,7.721010757773));
#43778=CARTESIAN_POINT('Ctrl Pts',(2.756791097347,-1.881958605473,7.703051902518));
#43779=CARTESIAN_POINT('Ctrl Pts',(2.707875130552,-1.697202037034,7.675957994411));
#43780=CARTESIAN_POINT('Ctrl Pts',(2.667269448356,-1.433978002984,7.651213835617));
#43781=CARTESIAN_POINT('Ctrl Pts',(2.655188267488,-1.188072643789,7.63769259235));
#43782=CARTESIAN_POINT('Ctrl Pts',(2.669252075638,-0.9625884713048,7.63275022109));
#43783=CARTESIAN_POINT('Ctrl Pts',(2.708556680229,-0.7591881016237,7.63436877623));
#43784=CARTESIAN_POINT('Ctrl Pts',(2.773606268264,-0.5803351016669,7.640737884484));
#43785=CARTESIAN_POINT('Ctrl Pts',(2.865015042587,-0.4307700699685,7.649762753622));
#43786=CARTESIAN_POINT('Ctrl Pts',(2.980841699795,-0.3181327676405,7.658830046356));
#43787=CARTESIAN_POINT('Ctrl Pts',(3.112743733696,-0.2504501741924,7.6652140151));
#43788=CARTESIAN_POINT('Ctrl Pts',(3.224577167091,-0.2326920076717,7.666977451746));
#43789=CARTESIAN_POINT('Ctrl Pts',(3.287204681318,-0.2368974193595,7.666582838974));
#43790=CARTESIAN_POINT('Ctrl Pts',(3.305617539918,-0.2394455144739,7.666401482426));
#43791=CARTESIAN_POINT('Ctrl Pts',(2.354707813324,-1.817087042029,7.300711712326));
#43792=CARTESIAN_POINT('Ctrl Pts',(2.34719425366,-1.803021267319,7.302353914292));
#43793=CARTESIAN_POINT('Ctrl Pts',(2.290915031225,-1.694244596348,7.31560478624));
#43794=CARTESIAN_POINT('Ctrl Pts',(2.206032845101,-1.481950544316,7.349512634112));
#43795=CARTESIAN_POINT('Ctrl Pts',(2.139909159661,-1.170091282631,7.413473773373));
#43796=CARTESIAN_POINT('Ctrl Pts',(2.126223235302,-0.8711180476606,7.483575579401));
#43797=CARTESIAN_POINT('Ctrl Pts',(2.160037805531,-0.5901682844192,7.555449904233));
#43798=CARTESIAN_POINT('Ctrl Pts',(2.239342696343,-0.3303374624533,7.626078694443));
#43799=CARTESIAN_POINT('Ctrl Pts',(2.364778982571,-0.09589688494384,7.692513876796));
#43800=CARTESIAN_POINT('Ctrl Pts',(2.537224667366,0.105246040717,7.750964265596));
#43801=CARTESIAN_POINT('Ctrl Pts',(2.752985727524,0.2602729087259,7.79651453519));
#43802=CARTESIAN_POINT('Ctrl Pts',(2.996933379488,0.3550315871828,7.824430482657));
#43803=CARTESIAN_POINT('Ctrl Pts',(3.203127274003,0.3801014864107,7.831768774722));
#43804=CARTESIAN_POINT('Ctrl Pts',(3.318595594879,0.3741633816109,7.830072397969));
#43805=CARTESIAN_POINT('Ctrl Pts',(3.352552019354,0.3705590653944,7.82915107849));
#43806=CARTESIAN_POINT('Ctrl Pts',(1.722078738097,-1.841162035607,7.310012002466));
#43807=CARTESIAN_POINT('Ctrl Pts',(1.714517855214,-1.82325387619,7.318210429835));
#43808=CARTESIAN_POINT('Ctrl Pts',(1.658918378237,-1.685294382398,7.381280276636));
#43809=CARTESIAN_POINT('Ctrl Pts',(1.589006788219,-1.423058481785,7.500753094977));
#43810=CARTESIAN_POINT('Ctrl Pts',(1.568209302474,-1.051506193311,7.667791090927));
#43811=CARTESIAN_POINT('Ctrl Pts',(1.613417879879,-0.7047595538035,7.821222793726));
#43812=CARTESIAN_POINT('Ctrl Pts',(1.714294320514,-0.3859681540512,7.959996344744));
#43813=CARTESIAN_POINT('Ctrl Pts',(1.865759429155,-0.0966333636266,8.083750427066));
#43814=CARTESIAN_POINT('Ctrl Pts',(2.066526668314,0.1601126450525,8.191369643204));
#43815=CARTESIAN_POINT('Ctrl Pts',(2.315861782763,0.3772080734943,8.280260680351));
#43816=CARTESIAN_POINT('Ctrl Pts',(2.608197466777,0.542551163196,8.346280004011));
#43817=CARTESIAN_POINT('Ctrl Pts',(2.926010971638,0.6427899774458,8.38547381194));
#43818=CARTESIAN_POINT('Ctrl Pts',(3.189996159877,0.6692080185729,8.395646328464));
#43819=CARTESIAN_POINT('Ctrl Pts',(3.337814974144,0.6629510827252,8.393278067348));
#43820=CARTESIAN_POINT('Ctrl Pts',(3.381343738726,0.6591564736418,8.391950440612));
#43821=CARTESIAN_POINT('',(1.75000000021594,-1.78647023985835,7.3336606126813));
#43822=CARTESIAN_POINT('Origin',(1.75,-2.186029020505,8.250368190795));
#43823=CARTESIAN_POINT('',(3.25,-0.04336631913618,7.86687525911));
#43824=CARTESIAN_POINT('Origin',(3.25,-0.2250371090282,8.850234666499));
#43825=CARTESIAN_POINT('Ctrl Pts',(1.75000000048586,-1.78647023867652,7.33366060996403));
#43826=CARTESIAN_POINT('Ctrl Pts',(1.75001261091093,-1.67132937033661,7.38385324834833));
#43827=CARTESIAN_POINT('Ctrl Pts',(1.77542675361188,-1.45285226422692,7.47262865678146));
#43828=CARTESIAN_POINT('Ctrl Pts',(1.861160899812,-1.164361559054,7.576243569427));
#43829=CARTESIAN_POINT('Ctrl Pts',(1.977195804371,-0.9138167090022,7.656329079677));
#43830=CARTESIAN_POINT('Ctrl Pts',(2.112596345794,-0.6991889689988,7.717855015608));
#43831=CARTESIAN_POINT('Ctrl Pts',(2.261791685601,-0.5166888823143,7.765159563871));
#43832=CARTESIAN_POINT('Ctrl Pts',(2.421231729676,-0.3644382359967,7.801148505907));
#43833=CARTESIAN_POINT('Ctrl Pts',(2.587582423301,-0.2420433787695,7.827817542484));
#43834=CARTESIAN_POINT('Ctrl Pts',(2.757987815569,-0.1491336781293,7.84673056923));
#43835=CARTESIAN_POINT('Ctrl Pts',(2.929826816222,-0.08520576210219,7.859080936862));
#43836=CARTESIAN_POINT('Ctrl Pts',(3.096992661939,-0.04997560015663,7.865659537624));
#43837=CARTESIAN_POINT('Ctrl Pts',(3.200093400178,-0.04336596610774,7.866875225272));
#43838=CARTESIAN_POINT('Ctrl Pts',(3.25,-0.04336631913618,7.86687525911));
#43839=CARTESIAN_POINT('Origin',(1.75,1.41,0.));
#43840=CARTESIAN_POINT('',(1.75,-5.923658654762,3.196474735617));
#43841=CARTESIAN_POINT('Origin',(1.75,-6.840365986607,3.596034077569));
#43842=CARTESIAN_POINT('Origin',(1.75,1.41,0.));
#43843=CARTESIAN_POINT('Ctrl Pts',(3.271450805884,-6.600784524332,2.179511695863));
#43844=CARTESIAN_POINT('Ctrl Pts',(3.264316214845,-6.600377874579,2.178186642191));
#43845=CARTESIAN_POINT('Ctrl Pts',(3.240231918653,-6.599695561688,2.175981939566));
#43846=CARTESIAN_POINT('Ctrl Pts',(3.197202365664,-6.602584594832,2.185291506928));
#43847=CARTESIAN_POINT('Ctrl Pts',(3.141761803778,-6.613837343706,2.222175058386));
#43848=CARTESIAN_POINT('Ctrl Pts',(3.083432184706,-6.633291854611,2.288342755621));
#43849=CARTESIAN_POINT('Ctrl Pts',(3.023840460015,-6.66019722422,2.384794977911));
#43850=CARTESIAN_POINT('Ctrl Pts',(2.964463630781,-6.693298019679,2.511543641683));
#43851=CARTESIAN_POINT('Ctrl Pts',(2.906684619961,-6.731189795874,2.66885803549));
#43852=CARTESIAN_POINT('Ctrl Pts',(2.852103604317,-6.772317939251,2.857792631679));
#43853=CARTESIAN_POINT('Ctrl Pts',(2.803187857468,-6.814706270047,3.080231240091));
#43854=CARTESIAN_POINT('Ctrl Pts',(2.764302638213,-6.85538301175,3.337654190934));
#43855=CARTESIAN_POINT('Ctrl Pts',(2.750023886213,-6.878666337879,3.535090238471));
#43856=CARTESIAN_POINT('Ctrl Pts',(2.748171519073,-6.888664773212,3.644483876021));
#43857=CARTESIAN_POINT('Ctrl Pts',(2.748037895908,-6.889914238717,3.658707376734));
#43858=CARTESIAN_POINT('Ctrl Pts',(3.305695023565,-6.256408875213,1.649469417717));
#43859=CARTESIAN_POINT('Ctrl Pts',(3.287257504913,-6.256590398572,1.646913457279));
#43860=CARTESIAN_POINT('Ctrl Pts',(3.224574537333,-6.256985835413,1.642697452954));
#43861=CARTESIAN_POINT('Ctrl Pts',(3.112635733078,-6.255219576771,1.660485800177));
#43862=CARTESIAN_POINT('Ctrl Pts',(2.980650256738,-6.248826651561,1.728271881478));
#43863=CARTESIAN_POINT('Ctrl Pts',(2.864782305834,-6.239750546342,1.841066970101));
#43864=CARTESIAN_POINT('Ctrl Pts',(2.773367855811,-6.230722480542,1.990835841996));
#43865=CARTESIAN_POINT('Ctrl Pts',(2.708363725574,-6.224362431101,2.169903227412));
#43866=CARTESIAN_POINT('Ctrl Pts',(2.669158301008,-6.222767402465,2.373417325382));
#43867=CARTESIAN_POINT('Ctrl Pts',(2.655195161133,-6.22773834187,2.598889472782));
#43868=CARTESIAN_POINT('Ctrl Pts',(2.667348643033,-6.241277363413,2.844712958734));
#43869=CARTESIAN_POINT('Ctrl Pts',(2.707993195755,-6.266049883286,3.107654258154));
#43870=CARTESIAN_POINT('Ctrl Pts',(2.756810997999,-6.293038359982,3.292099408065));
#43871=CARTESIAN_POINT('Ctrl Pts',(2.788464197933,-6.310948959069,3.38854088252));
#43872=CARTESIAN_POINT('Ctrl Pts',(2.792655545842,-6.313325094994,3.400979580454));
#43873=CARTESIAN_POINT('Ctrl Pts',(3.352694515196,-6.419142450118,1.039481056806));
#43874=CARTESIAN_POINT('Ctrl Pts',(3.318692730551,-6.420065951233,1.035865662458));
#43875=CARTESIAN_POINT('Ctrl Pts',(3.203122611875,-6.421766407795,1.029912756346));
#43876=CARTESIAN_POINT('Ctrl Pts',(2.996735102831,-6.414415900882,1.055025197856));
#43877=CARTESIAN_POINT('Ctrl Pts',(2.752632908899,-6.386458010439,1.149927772965));
#43878=CARTESIAN_POINT('Ctrl Pts',(2.536792417474,-6.340846931723,1.305166068799));
#43879=CARTESIAN_POINT('Ctrl Pts',(2.36433046361,-6.282324327712,1.506570330996));
#43880=CARTESIAN_POINT('Ctrl Pts',(2.238971023845,-6.215824387893,1.741270810204));
#43881=CARTESIAN_POINT('Ctrl Pts',(2.159845582096,-6.145179984273,2.001219054871));
#43882=CARTESIAN_POINT('Ctrl Pts',(2.126218782839,-6.073339305311,2.282127143621));
#43883=CARTESIAN_POINT('Ctrl Pts',(2.14004402452,-6.003289201097,2.580974729488));
#43884=CARTESIAN_POINT('Ctrl Pts',(2.206252171837,-5.939446912097,2.892483751437));
#43885=CARTESIAN_POINT('Ctrl Pts',(2.290967627635,-5.905574269497,3.104384124248));
#43886=CARTESIAN_POINT('Ctrl Pts',(2.347082827887,-5.89237152092,3.212853022938));
#43887=CARTESIAN_POINT('Ctrl Pts',(2.354531186858,-5.890744549661,3.226799824363));
#43888=CARTESIAN_POINT('Ctrl Pts',(3.381527042583,-6.981918423624,0.7508744730096));
#43889=CARTESIAN_POINT('Ctrl Pts',(3.33793980561,-6.983249539883,0.7470681478622));
#43890=CARTESIAN_POINT('Ctrl Pts',(3.189989944912,-6.985623678342,0.7407954945952));
#43891=CARTESIAN_POINT('Ctrl Pts',(2.925754637913,-6.975433994821,0.7672586248663));
#43892=CARTESIAN_POINT('Ctrl Pts',(2.607728547645,-6.936180022559,0.8676509822134));
#43893=CARTESIAN_POINT('Ctrl Pts',(2.315255948472,-6.870066961331,1.033223765781));
#43894=CARTESIAN_POINT('Ctrl Pts',(2.065845059635,-6.781052513204,1.250609837518));
#43895=CARTESIAN_POINT('Ctrl Pts',(1.865111694256,-6.673301299875,1.507655263828));
#43896=CARTESIAN_POINT('Ctrl Pts',(1.713837092142,-6.549474404633,1.797142544492));
#43897=CARTESIAN_POINT('Ctrl Pts',(1.613202352312,-6.410704136534,2.115912157827));
#43898=CARTESIAN_POINT('Ctrl Pts',(1.568201988779,-6.257320639317,2.462537074865));
#43899=CARTESIAN_POINT('Ctrl Pts',(1.589188572213,-6.090455036669,2.833709173528));
#43900=CARTESIAN_POINT('Ctrl Pts',(1.658984742568,-5.97119718329,3.095447355188));
#43901=CARTESIAN_POINT('Ctrl Pts',(1.714424163993,-5.908325889543,3.23301009736));
#43902=CARTESIAN_POINT('Ctrl Pts',(1.721918698242,-5.900199786108,3.250765686424));
#43903=CARTESIAN_POINT('',(3.25,-6.574209262715,2.135037109028));
#43904=CARTESIAN_POINT('',(3.25,-6.45687525911,1.453366319136));
#43905=CARTESIAN_POINT('Origin',(3.25,-7.440234666499,1.635037109028));
#43906=CARTESIAN_POINT('Ctrl Pts',(3.25,-6.57420926271478,2.13503710902813));
#43907=CARTESIAN_POINT('Ctrl Pts',(3.24051328877442,-6.574209580288,2.13503810640009));
#43908=CARTESIAN_POINT('Ctrl Pts',(3.23080615598635,-6.57445243030741,2.13600227329107));
#43909=CARTESIAN_POINT('Ctrl Pts',(3.22087230023474,-6.57497097820664,2.1380598369659));
#43910=CARTESIAN_POINT('Ctrl Pts',(3.21347574283905,-6.57535707897103,2.13959185919339));
#43911=CARTESIAN_POINT('Ctrl Pts',(3.20595370673705,-6.57589625420415,2.14173100212492));
#43912=CARTESIAN_POINT('Ctrl Pts',(3.19831104571938,-6.57660635689357,2.14454781654446));
#43913=CARTESIAN_POINT('Ctrl Pts',(3.19651447281003,-6.57677328190198,2.14520996974805));
#43914=CARTESIAN_POINT('Ctrl Pts',(3.19471116015858,-6.57694922279033,2.14590888702886));
#43915=CARTESIAN_POINT('Ctrl Pts',(3.19290156425008,-6.57713442323191,2.14664549535018));
#43916=CARTESIAN_POINT('Ctrl Pts',(3.18189733676813,-6.57826063476863,2.15112484098472));
#43917=CARTESIAN_POINT('Ctrl Pts',(3.17065888397034,-6.57973024826778,2.1570014501285));
#43918=CARTESIAN_POINT('Ctrl Pts',(3.15927245949691,-6.58157034387027,2.16439079707255));
#43919=CARTESIAN_POINT('Ctrl Pts',(3.1538680298637,-6.58244372314971,2.16789806185859));
#43920=CARTESIAN_POINT('Ctrl Pts',(3.14843060788739,-6.58340039015426,2.17174550131682));
#43921=CARTESIAN_POINT('Ctrl Pts',(3.14297129559834,-6.58444227478407,2.17594186663245));
#43922=CARTESIAN_POINT('Ctrl Pts',(3.13920633189964,-6.58516080078181,2.17883585075412));
#43923=CARTESIAN_POINT('Ctrl Pts',(3.13542993069291,-6.5859193107831,2.18189527048653));
#43924=CARTESIAN_POINT('Ctrl Pts',(3.13164589470533,-6.58671786767652,2.18512186217636));
#43925=CARTESIAN_POINT('Ctrl Pts',(3.12069286106816,-6.58902932045964,2.1944613524529));
#43926=CARTESIAN_POINT('Ctrl Pts',(3.109675479807,-6.59167741438172,2.20520508063705));
#43927=CARTESIAN_POINT('Ctrl Pts',(3.09866120950954,-6.59464872736088,2.21734787551539));
#43928=CARTESIAN_POINT('Ctrl Pts',(3.09442640256284,-6.59579114864755,2.22201658172238));
#43929=CARTESIAN_POINT('Ctrl Pts',(3.09019212355419,-6.59698119320272,2.22689159758761));
#43930=CARTESIAN_POINT('Ctrl Pts',(3.08596246544424,-6.59821749385538,2.23197066469041));
#43931=CARTESIAN_POINT('Ctrl Pts',(3.08024996729594,-6.59988721869021,2.23883035894125));
#43932=CARTESIAN_POINT('Ctrl Pts',(3.07454429121136,-6.60164320384453,2.24606655891752));
#43933=CARTESIAN_POINT('Ctrl Pts',(3.06885114450466,-6.60348280832308,2.25367794990381));
#43934=CARTESIAN_POINT('Ctrl Pts',(3.05557765797147,-6.60777181869476,2.27142379433048));
#43935=CARTESIAN_POINT('Ctrl Pts',(3.04237135767047,-6.61251695827372,2.29121255884396));
#43936=CARTESIAN_POINT('Ctrl Pts',(3.02927014080688,-6.61768864373912,2.31306301272805));
#43937=CARTESIAN_POINT('Ctrl Pts',(3.02178682413499,-6.62064267163348,2.32554382787229));
#43938=CARTESIAN_POINT('Ctrl Pts',(3.01433747439815,-6.62373755466617,2.3387007727525));
#43939=CARTESIAN_POINT('Ctrl Pts',(3.00693454048262,-6.62696290842619,2.35252311012848));
#43940=CARTESIAN_POINT('Ctrl Pts',(2.99581808697545,-6.6318061902286,2.37327912018529));
#43941=CARTESIAN_POINT('Ctrl Pts',(2.98480625277407,-6.6369442289306,2.39553659560213));
#43942=CARTESIAN_POINT('Ctrl Pts',(2.97393305392326,-6.64235017239947,2.4193015558268));
#43943=CARTESIAN_POINT('Ctrl Pts',(2.96487468961802,-6.64685381535004,2.43909993074558));
#43944=CARTESIAN_POINT('Ctrl Pts',(2.95591340816756,-6.65154466262965,2.45994580479158));
#43945=CARTESIAN_POINT('Ctrl Pts',(2.94707248054145,-6.65639850762819,2.48181799973957));
#43946=CARTESIAN_POINT('Ctrl Pts',(2.93823408053821,-6.66125096491153,2.50368394142292));
#43947=CARTESIAN_POINT('Ctrl Pts',(2.92951596079112,-6.66626612348122,2.52657487624024));
#43948=CARTESIAN_POINT('Ctrl Pts',(2.92094383128304,-6.67142497211021,2.55049507921643));
#43949=CARTESIAN_POINT('Ctrl Pts',(2.91065031956988,-6.67761977688293,2.5792187340894));
#43950=CARTESIAN_POINT('Ctrl Pts',(2.90056879809431,-6.68402127602502,2.6094220654221));
#43951=CARTESIAN_POINT('Ctrl Pts',(2.8907337765054,-6.69059072399738,2.64112227472971));
#43952=CARTESIAN_POINT('Ctrl Pts',(2.88418583059476,-6.69496452120737,2.66222759249904));
#43953=CARTESIAN_POINT('Ctrl Pts',(2.87774725879252,-6.69941230199369,2.68399537478204));
#43954=CARTESIAN_POINT('Ctrl Pts',(2.87143408618968,-6.70392417886007,2.70644225837694));
#43955=CARTESIAN_POINT('Ctrl Pts',(2.86159165554342,-6.71095833394112,2.74143764166619));
#43956=CARTESIAN_POINT('Ctrl Pts',(2.85205449398499,-6.71814491868167,2.77807325337933));
#43957=CARTESIAN_POINT('Ctrl Pts',(2.84288373170243,-6.72544280974844,2.81644159973842));
#43958=CARTESIAN_POINT('Ctrl Pts',(2.84175743423344,-6.72633909252018,2.82115376761089));
#43959=CARTESIAN_POINT('Ctrl Pts',(2.84063668982235,-6.72723702172671,2.82589202074456));
#43960=CARTESIAN_POINT('Ctrl Pts',(2.83952163404616,-6.72813649253441,2.83065648517027));
#43961=CARTESIAN_POINT('Ctrl Pts',(2.83514517450144,-6.73166680705819,2.8493564338692));
#43962=CARTESIAN_POINT('Ctrl Pts',(2.83085621640419,-6.73522097501525,2.86846030126194));
#43963=CARTESIAN_POINT('Ctrl Pts',(2.82666626830219,-6.73879389815918,2.88798042967713));
#43964=CARTESIAN_POINT('Ctrl Pts',(2.81859266003575,-6.74567856143616,2.92559375239581));
#43965=CARTESIAN_POINT('Ctrl Pts',(2.81088601077042,-6.75262925430877,2.96474438901527));
#43966=CARTESIAN_POINT('Ctrl Pts',(2.80364920149339,-6.75958428980929,3.00546602378017));
#43967=CARTESIAN_POINT('Ctrl Pts',(2.80088318048451,-6.76224261250034,3.02103046564451));
#43968=CARTESIAN_POINT('Ctrl Pts',(2.79818602344303,-6.76490133183295,3.03682401832795));
#43969=CARTESIAN_POINT('Ctrl Pts',(2.79556434006813,-6.76755605070014,3.05284692811978));
#43970=CARTESIAN_POINT('Ctrl Pts',(2.79319374416818,-6.76995651817167,3.0673352697027));
#43971=CARTESIAN_POINT('Ctrl Pts',(2.79088485160737,-6.77235370295779,3.0820111151052));
#43972=CARTESIAN_POINT('Ctrl Pts',(2.78864396027109,-6.77474457481874,3.09687549807305));
#43973=CARTESIAN_POINT('Ctrl Pts',(2.78243004536069,-6.78137438058622,3.13809392284103));
#43974=CARTESIAN_POINT('Ctrl Pts',(2.77673782796066,-6.78795234727477,3.18075634451844));
#43975=CARTESIAN_POINT('Ctrl Pts',(2.77172743500744,-6.79439750337758,3.22480001727387));
#43976=CARTESIAN_POINT('Ctrl Pts',(2.76860707762661,-6.79841139821653,3.25222940268233));
#43977=CARTESIAN_POINT('Ctrl Pts',(2.76575155268839,-6.80237343980551,3.28019374186988));
#43978=CARTESIAN_POINT('Ctrl Pts',(2.76320363662809,-6.806260205241,3.30866920745312));
#43979=CARTESIAN_POINT('Ctrl Pts',(2.76246674850062,-6.80738430479368,3.31690465635168));
#43980=CARTESIAN_POINT('Ctrl Pts',(2.76175561008452,-6.80850208713546,3.32518281325778));
#43981=CARTESIAN_POINT('Ctrl Pts',(2.76107146865022,-6.80961300152605,3.33350267279286));
#43982=CARTESIAN_POINT('Ctrl Pts',(2.75804225864649,-6.81453185721365,3.3703409645109));
#43983=CARTESIAN_POINT('Ctrl Pts',(2.75553951217967,-6.81931358854474,3.40799423196495));
#43984=CARTESIAN_POINT('Ctrl Pts',(2.75367822980329,-6.82391801056441,3.44648708900259));
#43985=CARTESIAN_POINT('Ctrl Pts',(2.75194379522927,-6.82820863773932,3.48235662870593));
#43986=CARTESIAN_POINT('Ctrl Pts',(2.75076637573596,-6.83234532670531,3.5189555638735));
#43987=CARTESIAN_POINT('Ctrl Pts',(2.75026751838297,-6.83628130815854,3.55627119138643));
#43988=CARTESIAN_POINT('Ctrl Pts',(2.75009151577668,-6.83766996764193,3.56943657355102));
#43989=CARTESIAN_POINT('Ctrl Pts',(2.75000025092927,-6.83903350525114,3.58269083008542));
#43990=CARTESIAN_POINT('Ctrl Pts',(2.7500000000008,-6.84036938720128,3.59603220353762));
#43991=CARTESIAN_POINT('Ctrl Pts',(2.74999999998808,-6.84036945491068,3.59603287974736));
#43992=CARTESIAN_POINT('Ctrl Pts',(2.7499999999756,-6.84036952262001,3.59603355595731));
#43993=CARTESIAN_POINT('Ctrl Pts',(2.74999999996335,-6.84036959032926,3.59603423216749));
#43994=CARTESIAN_POINT('Ctrl Pts',(3.25,-6.45687525911025,1.45336631913605));
#43995=CARTESIAN_POINT('Ctrl Pts',(3.200061038244,-6.45687531917522,1.45336599401248));
#43996=CARTESIAN_POINT('Ctrl Pts',(3.14847540739251,-6.4562670418847,1.45667483599627));
#43997=CARTESIAN_POINT('Ctrl Pts',(3.09479707713993,-6.45486414723981,1.46421034877569));
#43998=CARTESIAN_POINT('Ctrl Pts',(3.04111874688734,-6.45346125259492,1.47174586155511));
#43999=CARTESIAN_POINT('Ctrl Pts',(2.98534771723367,-6.45126498433326,1.48350827579869));
#44000=CARTESIAN_POINT('Ctrl Pts',(2.92880284639516,-6.44810528300073,1.50006045254051));
#44001=CARTESIAN_POINT('Ctrl Pts',(2.87225797555666,-6.4449455816682,1.51661262928234));
#44002=CARTESIAN_POINT('Ctrl Pts',(2.81493926353333,-6.44082214246287,1.53795450990436));
#44003=CARTESIAN_POINT('Ctrl Pts',(2.75786489396516,-6.43560370021495,1.56412997515346));
#44004=CARTESIAN_POINT('Ctrl Pts',(2.700790524397,-6.43038525796702,1.59030544040256));
#44005=CARTESIAN_POINT('Ctrl Pts',(2.643960497284,-6.4240722818765,1.62131458592504));
#44006=CARTESIAN_POINT('Ctrl Pts',(2.58779565893966,-6.41646225785502,1.65725330784731));
#44007=CARTESIAN_POINT('Ctrl Pts',(2.53512661061407,-6.40932589398821,1.69095514582072));
#44008=CARTESIAN_POINT('Ctrl Pts',(2.48304252316936,-6.4010485467861,1.72899184972167));
#44009=CARTESIAN_POINT('Ctrl Pts',(2.43194867115751,-6.39141658065603,1.77141167859568));
#44010=CARTESIAN_POINT('Ctrl Pts',(2.42855743126309,-6.39077728049533,1.77422719964817));
#44011=CARTESIAN_POINT('Ctrl Pts',(2.42517055369546,-6.39013199469215,1.77706202360263));
#44012=CARTESIAN_POINT('Ctrl Pts',(2.42178815695477,-6.38948065302519,1.77991616181372));
#44013=CARTESIAN_POINT('Ctrl Pts',(2.37166766403781,-6.37982904562717,1.82220889828441));
#44014=CARTESIAN_POINT('Ctrl Pts',(2.3225310457101,-6.36885175503254,1.86874387943997));
#44015=CARTESIAN_POINT('Ctrl Pts',(2.27483701918363,-6.35629580130176,1.91954409344578));
#44016=CARTESIAN_POINT('Ctrl Pts',(2.27081892151714,-6.35523799486225,1.92382387932716));
#44017=CARTESIAN_POINT('Ctrl Pts',(2.2668110628251,-6.35416895545652,1.92813392605475));
#44018=CARTESIAN_POINT('Ctrl Pts',(2.26281371740039,-6.353088516178,1.93247424044547));
#44019=CARTESIAN_POINT('Ctrl Pts',(2.2201788328164,-6.34156476752845,1.97876716323444));
#44020=CARTESIAN_POINT('Ctrl Pts',(2.1787399299299,-6.32874810757987,2.02850464921655));
#44021=CARTESIAN_POINT('Ctrl Pts',(2.13882776655781,-6.31436833841078,2.08185824987127));
#44022=CARTESIAN_POINT('Ctrl Pts',(2.13058023305217,-6.31139687262177,2.0928833502885));
#44023=CARTESIAN_POINT('Ctrl Pts',(2.12239789278961,-6.30835849921372,2.10406278968684));
#44024=CARTESIAN_POINT('Ctrl Pts',(2.11428366431634,-6.3052505765884,2.11539796266622));
#44025=CARTESIAN_POINT('Ctrl Pts',(2.07988507840782,-6.29207518427888,2.16345107366793));
#44026=CARTESIAN_POINT('Ctrl Pts',(2.04671057025077,-6.27765365439441,2.21430410098874));
#44027=CARTESIAN_POINT('Ctrl Pts',(2.01509997230188,-6.26171202128629,2.26822279823904));
#44028=CARTESIAN_POINT('Ctrl Pts',(2.0031695090356,-6.25569533446156,2.28857277826633));
#44029=CARTESIAN_POINT('Ctrl Pts',(1.99146181797665,-6.24946164733413,2.30935923610152));
#44030=CARTESIAN_POINT('Ctrl Pts',(1.97999516912917,-6.24299445217726,2.33059561377431));
#44031=CARTESIAN_POINT('Ctrl Pts',(1.94999818237139,-6.22607613802455,2.38615040997562));
#44032=CARTESIAN_POINT('Ctrl Pts',(1.92165078304898,-6.20756304660474,2.4447853243894));
#44033=CARTESIAN_POINT('Ctrl Pts',(1.89563069728732,-6.18715556759926,2.50663664732157));
#44034=CARTESIAN_POINT('Ctrl Pts',(1.88535055886863,-6.17909288437544,2.53107316021189));
#44035=CARTESIAN_POINT('Ctrl Pts',(1.87543369533783,-6.17073402192865,2.55601144677107));
#44036=CARTESIAN_POINT('Ctrl Pts',(1.865921901754,-6.1620585630372,2.58145871900657));
#44037=CARTESIAN_POINT('Ctrl Pts',(1.84188066661732,-6.14013117938556,2.64577717272496));
#44038=CARTESIAN_POINT('Ctrl Pts',(1.82042716017291,-6.11618429015519,2.71334849296128));
#44039=CARTESIAN_POINT('Ctrl Pts',(1.80262601149376,-6.08988601050222,2.78418925891778));
#44040=CARTESIAN_POINT('Ctrl Pts',(1.79555783429077,-6.07944393712419,2.81231750479677));
#44041=CARTESIAN_POINT('Ctrl Pts',(1.78906548420749,-6.06863070306812,2.84096085726446));
#44042=CARTESIAN_POINT('Ctrl Pts',(1.78321560761792,-6.05742376295122,2.87011887288863));
#44043=CARTESIAN_POINT('Ctrl Pts',(1.76727058462547,-6.02687697874084,2.94959494771222));
#44044=CARTESIAN_POINT('Ctrl Pts',(1.75609878882583,-5.99340723684766,3.03289665525687));
#44045=CARTESIAN_POINT('Ctrl Pts',(1.75187206416855,-5.95661567846224,3.11977137717403));
#44046=CARTESIAN_POINT('Ctrl Pts',(1.75064269165845,-5.94591459567352,3.14503949932704));
#44047=CARTESIAN_POINT('Ctrl Pts',(1.75000085690326,-5.93493232465646,3.17060960179539));
#44048=CARTESIAN_POINT('Ctrl Pts',(1.75,-5.92365865476181,3.19647473561692));
#44049=CARTESIAN_POINT('Origin',(-41.76566382177,-7.440234666499,1.635037109028));
#44050=CARTESIAN_POINT('',(4.75,-6.45687525911,1.453366319136));
#44051=CARTESIAN_POINT('',(4.75,-6.574209262715,2.135037109028));
#44052=CARTESIAN_POINT('Origin',(4.75,-7.440234666499,1.635037109028));
#44053=CARTESIAN_POINT('',(4.75,-6.574209262851,2.135037109265));
#44054=CARTESIAN_POINT('',(3.25,-6.45687525911,1.453366319136));
#44055=CARTESIAN_POINT('Origin',(4.75,-7.440234666499,1.635037109028));
#44056=CARTESIAN_POINT('Origin',(4.75,-5.965195555416,1.36253092419));
#44057=CARTESIAN_POINT('Origin',(4.75,-6.141196560822,2.385037109028));
#44058=CARTESIAN_POINT('Origin',(4.75,-6.110531496591,2.331923659762));
#44059=CARTESIAN_POINT('',(4.75,-8.966250804401,6.278174593044));
#44060=CARTESIAN_POINT('',(4.75,-6.574209262851,2.135037109265));
#44061=CARTESIAN_POINT('Origin',(4.75,-8.533238102513,6.528174593052));
#44062=CARTESIAN_POINT('Origin',(5.25,-8.966250804405,6.278174593052));
#44063=CARTESIAN_POINT('',(3.25,-8.966250804405,6.278174593052));
#44064=CARTESIAN_POINT('',(4.75,-8.966250804401,6.278174593044));
#44065=CARTESIAN_POINT('',(3.25,-8.966250804398,6.278174593039));
#44066=CARTESIAN_POINT('Origin',(3.25,-6.461881837768,2.940480301938));
#44067=CARTESIAN_POINT('Origin',(3.25,-8.533238102513,6.528174593052));
#44068=CARTESIAN_POINT('Origin',(3.25,-6.368174593052,7.778174593052));
#44069=CARTESIAN_POINT('Origin',(3.25,-6.368174593052,7.778174593052));
#44070=CARTESIAN_POINT('Origin',(5.25,-6.368174593052,7.778174593052));
#44071=CARTESIAN_POINT('',(4.75,-4.868174593052,10.37625080441));
#44072=CARTESIAN_POINT('Origin',(4.75,-6.368174593052,7.778174593052));
#44073=CARTESIAN_POINT('',(4.75,-4.868174593043,10.3762508044));
#44074=CARTESIAN_POINT('Origin',(4.75,-6.368174593052,7.778174593052));
#44075=CARTESIAN_POINT('Origin',(4.75,-5.118174593052,9.943238102513));
#44076=CARTESIAN_POINT('Origin',(4.75,-5.171288042318,9.973903166745));
#44077=CARTESIAN_POINT('',(4.75,-0.7250371092557,7.984209262846));
#44078=CARTESIAN_POINT('',(4.75,-4.868174593043,10.3762508044));
#44079=CARTESIAN_POINT('Origin',(4.75,-0.9750371090282,7.551196560822));
#44080=CARTESIAN_POINT('Origin',(5.25,-0.3950637418857,7.793699050369));
#44081=CARTESIAN_POINT('',(3.25,-0.7250371090282,7.984209262715));
#44082=CARTESIAN_POINT('Origin',(33.40462042024,-0.2250371090282,8.850234666499));
#44083=CARTESIAN_POINT('',(4.75,-0.04336631913618,7.86687525911));
#44084=CARTESIAN_POINT('Origin',(4.75,-0.2250371090282,8.850234666499));
#44085=CARTESIAN_POINT('',(4.75,-0.04336631887412,7.866875259159));
#44086=CARTESIAN_POINT('Origin',(4.75,-0.2250371090282,8.850234666499));
#44087=CARTESIAN_POINT('Origin',(4.75,0.04746907580983,7.375195555416));
#44088=CARTESIAN_POINT('Origin',(4.75,1.41,0.));
#44089=CARTESIAN_POINT('',(4.75,1.41,8.));
#44090=CARTESIAN_POINT('Origin',(4.75,1.41,0.));
#44091=CARTESIAN_POINT('Origin',(4.75,1.41,7.5));
#44092=CARTESIAN_POINT('Origin',(-4.6,1.41,0.));
#44093=CARTESIAN_POINT('',(4.75,1.410000000002,-8.));
#44094=CARTESIAN_POINT('Origin',(4.75,1.41,0.));
#44095=CARTESIAN_POINT('',(-4.1,1.410000000002,8.));
#44096=CARTESIAN_POINT('',(-4.1,1.410000000002,8.));
#44097=CARTESIAN_POINT('',(-4.1,1.41,-8.));
#44098=CARTESIAN_POINT('Origin',(-4.1,1.41,0.));
#44099=CARTESIAN_POINT('',(-4.1,1.410000000002,-8.));
#44100=CARTESIAN_POINT('Origin',(4.75,1.41,0.));
#44101=CARTESIAN_POINT('Origin',(4.75,1.41,-7.5));
#44102=CARTESIAN_POINT('Origin',(4.75,4.213822859968,-7.5));
#44103=CARTESIAN_POINT('',(4.75000019975999,3.6383472114225,-8.00000004058105));
#44104=CARTESIAN_POINT('',(4.75000019976,3.638347231863,-8.000000176328));
#44105=CARTESIAN_POINT('Origin',(4.75,3.638347150101,-7.5));
#44106=CARTESIAN_POINT('Origin',(-4.6,1.41,-8.));
#44107=CARTESIAN_POINT('',(-4.09999992634177,3.59647863879817,-8.00000011306536));
#44108=CARTESIAN_POINT('',(-4.1,1.410000000002,-8.));
#44109=CARTESIAN_POINT('',(-1.576219094765,2.688757347123,-8.));
#44110=CARTESIAN_POINT('Ctrl Pts',(-4.099999915327,3.596478469713,-8.));
#44111=CARTESIAN_POINT('Ctrl Pts',(-4.018359390359,3.529042992373,-8.));
#44112=CARTESIAN_POINT('Ctrl Pts',(-3.93452530619,3.465279502913,-8.));
#44113=CARTESIAN_POINT('Ctrl Pts',(-3.84862157962933,3.40513255040783,-8.));
#44114=CARTESIAN_POINT('Ctrl Pts',(-3.76271785306867,3.34498559790267,-8.));
#44115=CARTESIAN_POINT('Ctrl Pts',(-3.67474448411633,3.28845518235233,-8.));
#44116=CARTESIAN_POINT('Ctrl Pts',(-3.58456988763017,3.23541665283533,-8.));
#44117=CARTESIAN_POINT('Ctrl Pts',(-3.494395291144,3.18237812331833,-8.));
#44118=CARTESIAN_POINT('Ctrl Pts',(-3.402019467124,3.13283147983467,-8.));
#44119=CARTESIAN_POINT('Ctrl Pts',(-3.307166927403,3.08676170221583,-8.));
#44120=CARTESIAN_POINT('Ctrl Pts',(-3.212314387682,3.040691924597,-8.));
#44121=CARTESIAN_POINT('Ctrl Pts',(-3.11498513226,2.998099012843,-8.));
#44122=CARTESIAN_POINT('Ctrl Pts',(-3.0152306510545,2.95919441423967,-8.));
#44123=CARTESIAN_POINT('Ctrl Pts',(-2.915476169849,2.92028981563633,-8.));
#44124=CARTESIAN_POINT('Ctrl Pts',(-2.81329646286,2.88507353018367,-8.));
#44125=CARTESIAN_POINT('Ctrl Pts',(-2.706913955166,2.8534050156445,-8.));
#44126=CARTESIAN_POINT('Ctrl Pts',(-2.600531447472,2.82173650110533,-8.));
#44127=CARTESIAN_POINT('Ctrl Pts',(-2.489946139073,2.79361575747967,-8.));
#44128=CARTESIAN_POINT('Ctrl Pts',(-2.37284548982433,2.76958445078183,-8.));
#44129=CARTESIAN_POINT('Ctrl Pts',(-2.25574484057567,2.745553144084,-8.));
#44130=CARTESIAN_POINT('Ctrl Pts',(-2.13212885047733,2.725611274314,-8.));
#44131=CARTESIAN_POINT('Ctrl Pts',(-1.99962443142992,2.711412599665,-8.));
#44132=CARTESIAN_POINT('Ctrl Pts',(-1.8671200123825,2.697213925016,-8.));
#44133=CARTESIAN_POINT('Ctrl Pts',(-1.725727164386,2.688758445488,-8.));
#44134=CARTESIAN_POINT('Ctrl Pts',(-1.576219094765,2.688757347123,-8.));
#44135=CARTESIAN_POINT('',(2.16937313768,2.688757347123,-8.));
#44136=CARTESIAN_POINT('',(-1.576219094765,2.688757347123,-8.));
#44137=CARTESIAN_POINT('Ctrl Pts',(2.16937313768,2.688757347123,-8.));
#44138=CARTESIAN_POINT('Ctrl Pts',(2.284499469128,2.688757798533,-8.));
#44139=CARTESIAN_POINT('Ctrl Pts',(2.3964607117535,2.6937462920655,-8.));
#44140=CARTESIAN_POINT('Ctrl Pts',(2.50432998544575,2.70274264988892,-8.));
#44141=CARTESIAN_POINT('Ctrl Pts',(2.612199259138,2.71173900771233,-8.));
#44142=CARTESIAN_POINT('Ctrl Pts',(2.715976563897,2.72474322982667,-8.));
#44143=CARTESIAN_POINT('Ctrl Pts',(2.81844949985083,2.7415977468805,-8.));
#44144=CARTESIAN_POINT('Ctrl Pts',(2.92092243580467,2.75845226393433,-8.));
#44145=CARTESIAN_POINT('Ctrl Pts',(3.02209100295334,2.77915707592767,-8.));
#44146=CARTESIAN_POINT('Ctrl Pts',(3.12132923442132,2.80345374875183,-8.));
#44147=CARTESIAN_POINT('Ctrl Pts',(3.22056746588931,2.82775042157599,-8.));
#44148=CARTESIAN_POINT('Ctrl Pts',(3.31787536167661,2.85563895523098,-8.));
#44149=CARTESIAN_POINT('Ctrl Pts',(3.41368272796592,2.88706205193797,-8.));
#44150=CARTESIAN_POINT('Ctrl Pts',(3.50949009425531,2.91848514864499,-8.));
#44151=CARTESIAN_POINT('Ctrl Pts',(3.6037969310467,2.95344280840401,-8.));
#44152=CARTESIAN_POINT('Ctrl Pts',(3.69671207446142,2.99197095919337,-8.));
#44153=CARTESIAN_POINT('Ctrl Pts',(3.78962721787606,3.03049910998269,-8.));
#44154=CARTESIAN_POINT('Ctrl Pts',(3.88115066791403,3.07259775180235,-8.));
#44155=CARTESIAN_POINT('Ctrl Pts',(3.97141476700251,3.11841262290817,-8.));
#44156=CARTESIAN_POINT('Ctrl Pts',(4.061678866091,3.164227494014,-8.));
#44157=CARTESIAN_POINT('Ctrl Pts',(4.15068361423,3.213758594406,-8.));
#44158=CARTESIAN_POINT('Ctrl Pts',(4.2384834233655,3.26725712317767,-8.));
#44159=CARTESIAN_POINT('Ctrl Pts',(4.326283232501,3.32075565194933,-8.));
#44160=CARTESIAN_POINT('Ctrl Pts',(4.412878102633,3.37822160910067,-8.));
#44161=CARTESIAN_POINT('Ctrl Pts',(4.49819320382275,3.43997159218608,-8.));
#44162=CARTESIAN_POINT('Ctrl Pts',(4.58350830152976,3.50172157275074,-8.));
#44163=CARTESIAN_POINT('Ctrl Pts',(4.66754363039901,3.56775557889971,-8.));
#44164=CARTESIAN_POINT('Ctrl Pts',(4.75000018966185,3.63834722321791,-8.));
#44165=CARTESIAN_POINT('Ctrl Pts',(2.116278824535,3.685575955387,-8.914669819439));
#44166=CARTESIAN_POINT('Ctrl Pts',(2.133974364313,3.685202511829,-8.913936796476));
#44167=CARTESIAN_POINT('Ctrl Pts',(2.239909103176,3.683895874728,-8.90958933508));
#44168=CARTESIAN_POINT('Ctrl Pts',(2.429044891448,3.691486482049,-8.902264402712));
#44169=CARTESIAN_POINT('Ctrl Pts',(2.679654460364,3.723106835226,-8.893510969338));
#44170=CARTESIAN_POINT('Ctrl Pts',(2.918517115661,3.77349021367,-8.886064087219));
#44171=CARTESIAN_POINT('Ctrl Pts',(3.148793502593,3.841976725606,-8.879768421771));
#44172=CARTESIAN_POINT('Ctrl Pts',(3.371320421461,3.928221561954,-8.874576435951));
#44173=CARTESIAN_POINT('Ctrl Pts',(3.586961347311,4.032566912426,-8.870469771728));
#44174=CARTESIAN_POINT('Ctrl Pts',(3.796243341077,4.155927546394,-8.867468981321));
#44175=CARTESIAN_POINT('Ctrl Pts',(3.999311125999,4.299791587489,-8.865635475613));
#44176=CARTESIAN_POINT('Ctrl Pts',(4.196870836309,4.467121255863,-8.865073355886));
#44177=CARTESIAN_POINT('Ctrl Pts',(4.390781885124,4.664118803414,-8.865984111162));
#44178=CARTESIAN_POINT('Ctrl Pts',(4.58185832671,4.900643864149,-8.868774418082));
#44179=CARTESIAN_POINT('Ctrl Pts',(4.766586072556,5.188641909635,-8.874118740203));
#44180=CARTESIAN_POINT('Ctrl Pts',(4.935004609316,5.539877033665,-8.882942615775));
#44181=CARTESIAN_POINT('Ctrl Pts',(5.06881085959,5.961167749208,-8.896284405282));
#44182=CARTESIAN_POINT('Ctrl Pts',(5.142480202847,6.444827636589,-8.914820452271));
#44183=CARTESIAN_POINT('Ctrl Pts',(5.134565454299,6.910226196755,-8.935812671574));
#44184=CARTESIAN_POINT('Ctrl Pts',(5.086154708016,7.20557677316,-8.950861426659));
#44185=CARTESIAN_POINT('Ctrl Pts',(5.059038787903,7.325804132106,-8.957281445266));
#44186=CARTESIAN_POINT('Ctrl Pts',(2.1154288364,3.637085259508,-8.348384030449));
#44187=CARTESIAN_POINT('Ctrl Pts',(2.133400208805,3.636290273659,-8.347686475024));
#44188=CARTESIAN_POINT('Ctrl Pts',(2.241031179989,3.632497380359,-8.343553235046));
#44189=CARTESIAN_POINT('Ctrl Pts',(2.433665358953,3.636061516638,-8.33661798874));
#44190=CARTESIAN_POINT('Ctrl Pts',(2.689779275819,3.66336607149,-8.328377510496));
#44191=CARTESIAN_POINT('Ctrl Pts',(2.934551817168,3.710677008797,-8.321401663127));
#44192=CARTESIAN_POINT('Ctrl Pts',(3.171022006258,3.777280474976,-8.315529203019));
#44193=CARTESIAN_POINT('Ctrl Pts',(3.399874678972,3.862820491692,-8.310703523916));
#44194=CARTESIAN_POINT('Ctrl Pts',(3.621834783565,3.96763839521,-8.306897709465));
#44195=CARTESIAN_POINT('Ctrl Pts',(3.837283647501,4.092660683915,-8.304122996033));
#44196=CARTESIAN_POINT('Ctrl Pts',(4.046201161548,4.239396089147,-8.302430243022));
#44197=CARTESIAN_POINT('Ctrl Pts',(4.249124654791,4.410851402467,-8.30191168612));
#44198=CARTESIAN_POINT('Ctrl Pts',(4.447727052512,4.613350620516,-8.302751920613));
#44199=CARTESIAN_POINT('Ctrl Pts',(4.642490961035,4.856958632612,-8.305328882577));
#44200=CARTESIAN_POINT('Ctrl Pts',(4.829272674408,5.153781459785,-8.310276411291));
#44201=CARTESIAN_POINT('Ctrl Pts',(4.997130608976,5.515463539827,-8.318479830472));
#44202=CARTESIAN_POINT('Ctrl Pts',(5.126539475247,5.948065657011,-8.330966280555));
#44203=CARTESIAN_POINT('Ctrl Pts',(5.191058871723,6.442132504575,-8.348484454665));
#44204=CARTESIAN_POINT('Ctrl Pts',(5.170988750385,6.91385957546,-8.368577870152));
#44205=CARTESIAN_POINT('Ctrl Pts',(5.113623097214,7.210715672424,-8.383180326519));
#44206=CARTESIAN_POINT('Ctrl Pts',(5.082734909316,7.331093861617,-8.389443006712));
#44207=CARTESIAN_POINT('Ctrl Pts',(2.107932622538,3.209437931445,-7.974093609674));
#44208=CARTESIAN_POINT('Ctrl Pts',(2.128396203266,3.20832377114,-7.973710572124));
#44209=CARTESIAN_POINT('Ctrl Pts',(2.250984002149,3.202768031486,-7.97144548218));
#44210=CARTESIAN_POINT('Ctrl Pts',(2.470711253402,3.204775266025,-7.967678546612));
#44211=CARTESIAN_POINT('Ctrl Pts',(2.763453159674,3.233567093421,-7.963258313335));
#44212=CARTESIAN_POINT('Ctrl Pts',(3.043704631512,3.285693179689,-7.959557451335));
#44213=CARTESIAN_POINT('Ctrl Pts',(3.314817166296,3.360322787411,-7.956471695572));
#44214=CARTESIAN_POINT('Ctrl Pts',(3.577466067767,3.457049507122,-7.953956646518));
#44215=CARTESIAN_POINT('Ctrl Pts',(3.832382497416,3.5762604501,-7.951986459763));
#44216=CARTESIAN_POINT('Ctrl Pts',(4.079906764865,3.719010073588,-7.950557558931));
#44217=CARTESIAN_POINT('Ctrl Pts',(4.319915478746,3.887014376219,-7.949688993494));
#44218=CARTESIAN_POINT('Ctrl Pts',(4.552916354557,4.083696712316,-7.949423413387));
#44219=CARTESIAN_POINT('Ctrl Pts',(4.780697367817,4.316276202614,-7.949853814381));
#44220=CARTESIAN_POINT('Ctrl Pts',(5.003620995656,4.596243417174,-7.951177111079));
#44221=CARTESIAN_POINT('Ctrl Pts',(5.216642853094,4.937350941106,-7.953731995165));
#44222=CARTESIAN_POINT('Ctrl Pts',(5.406819439974,5.352632881146,-7.958009960562));
#44223=CARTESIAN_POINT('Ctrl Pts',(5.551348297991,5.848391301807,-7.964620728133));
#44224=CARTESIAN_POINT('Ctrl Pts',(5.619772718639,6.412753788441,-7.974098483983));
#44225=CARTESIAN_POINT('Ctrl Pts',(5.590729149136,6.949067622384,-7.985268994065));
#44226=CARTESIAN_POINT('Ctrl Pts',(5.521121943126,7.28486103587,-7.993617512756));
#44227=CARTESIAN_POINT('Ctrl Pts',(5.484197631687,7.420713649103,-7.997235986271));
#44228=CARTESIAN_POINT('Ctrl Pts',(2.097982686268,2.641809757266,-8.001132743794));
#44229=CARTESIAN_POINT('Ctrl Pts',(2.121761001818,2.640657299117,-8.001167370025));
#44230=CARTESIAN_POINT('Ctrl Pts',(2.26420112762,2.63504805256,-8.001379534588));
#44231=CARTESIAN_POINT('Ctrl Pts',(2.519463443997,2.638838702993,-8.001787552801));
#44232=CARTESIAN_POINT('Ctrl Pts',(2.859471577427,2.674089067881,-8.002358257106));
#44233=CARTESIAN_POINT('Ctrl Pts',(3.18492826935,2.736224863315,-8.002904688175));
#44234=CARTESIAN_POINT('Ctrl Pts',(3.499756825995,2.824300917133,-8.003410580015));
#44235=CARTESIAN_POINT('Ctrl Pts',(3.804770782395,2.937849332127,-8.003858188745));
#44236=CARTESIAN_POINT('Ctrl Pts',(4.10084877835,3.077324021872,-8.004231772651));
#44237=CARTESIAN_POINT('Ctrl Pts',(4.388417761842,3.24395206713,-8.004515730234));
#44238=CARTESIAN_POINT('Ctrl Pts',(4.667370373622,3.439727472378,-8.00469383333));
#44239=CARTESIAN_POINT('Ctrl Pts',(4.938340469526,3.668629169678,-8.004749158421));
#44240=CARTESIAN_POINT('Ctrl Pts',(5.203468267774,3.93904415572,-8.004659626021));
#44241=CARTESIAN_POINT('Ctrl Pts',(5.463274621234,4.26431174805,-8.004390090535));
#44242=CARTESIAN_POINT('Ctrl Pts',(5.712047138579,4.660396215544,-8.003894643709));
#44243=CARTESIAN_POINT('Ctrl Pts',(5.934939194387,5.142453440912,-8.003137596628));
#44244=CARTESIAN_POINT('Ctrl Pts',(6.1056490689,5.717890833968,-8.002138506643));
#44245=CARTESIAN_POINT('Ctrl Pts',(6.1888494719,6.37312249819,-8.001050166323));
#44246=CARTESIAN_POINT('Ctrl Pts',(6.159033073884,6.9961590832,-8.000264096742));
#44247=CARTESIAN_POINT('Ctrl Pts',(6.080744158775,7.386544638581,-8.000048758441));
#44248=CARTESIAN_POINT('Ctrl Pts',(6.038895767987,7.544540690767,-8.000015016273));
#44249=CARTESIAN_POINT('',(5.18295248725182,7.29695751098408,-8.53243621599188));
#44250=CARTESIAN_POINT('Ctrl Pts',(5.1829522985385,7.29695750739212,-8.53243627219658));
#44251=CARTESIAN_POINT('Ctrl Pts',(5.18723923406474,7.24664967889388,-8.54361501736799));
#44252=CARTESIAN_POINT('Ctrl Pts',(5.19130154250867,7.19348202716866,-8.55459110489445));
#44253=CARTESIAN_POINT('Ctrl Pts',(5.19490205157409,7.13800448322447,-8.56468063816348));
#44254=CARTESIAN_POINT('Ctrl Pts',(5.19528501692091,7.13210365740475,-8.56575380352356));
#44255=CARTESIAN_POINT('Ctrl Pts',(5.19566273688535,7.12617665834645,-8.56681692760366));
#44256=CARTESIAN_POINT('Ctrl Pts',(5.19603491554704,7.12022412060748,-8.56786918139442));
#44257=CARTESIAN_POINT('Ctrl Pts',(5.19789902987704,7.09040991565347,-8.57313955708245));
#44258=CARTESIAN_POINT('Ctrl Pts',(5.19962419820451,7.05995761975205,-8.57814494571069));
#44259=CARTESIAN_POINT('Ctrl Pts',(5.20121350787315,7.02852136024741,-8.5827781149027));
#44260=CARTESIAN_POINT('Ctrl Pts',(5.20218206777201,7.00936341958488,-8.585601669036));
#44261=CARTESIAN_POINT('Ctrl Pts',(5.20309921267649,6.98983994056404,-8.58828700549728));
#44262=CARTESIAN_POINT('Ctrl Pts',(5.20395612249813,6.96987196846932,-8.59081022277285));
#44263=CARTESIAN_POINT('Ctrl Pts',(5.20461321692097,6.95456015529194,-8.59274507280901));
#44264=CARTESIAN_POINT('Ctrl Pts',(5.20523474535529,6.93898696204747,-8.59458460040998));
#44265=CARTESIAN_POINT('Ctrl Pts',(5.20581397145749,6.92311679382367,-8.59631817378764));
#44266=CARTESIAN_POINT('Ctrl Pts',(5.2077358588334,6.8704591600474,-8.60207021565373));
#44267=CARTESIAN_POINT('Ctrl Pts',(5.20919999246733,6.81452954470778,-8.60664116434144));
#44268=CARTESIAN_POINT('Ctrl Pts',(5.20999840830055,6.75545526215373,-8.60910833131169));
#44269=CARTESIAN_POINT('Ctrl Pts',(5.21026934367702,6.73540892499787,-8.6099455426796));
#44270=CARTESIAN_POINT('Ctrl Pts',(5.21046332268927,6.71500010887712,-8.61054064166149));
#44271=CARTESIAN_POINT('Ctrl Pts',(5.21057211880332,6.69423259999795,-8.61085815377749));
#44272=CARTESIAN_POINT('Ctrl Pts',(5.21076175376346,6.65803419573641,-8.61141158712377));
#44273=CARTESIAN_POINT('Ctrl Pts',(5.21069210583572,6.62074565536196,-8.61111312886292));
#44274=CARTESIAN_POINT('Ctrl Pts',(5.21029733445679,6.58264849326771,-8.60988509567174));
#44275=CARTESIAN_POINT('Ctrl Pts',(5.20991968294653,6.54620347326579,-8.60871031803069));
#44276=CARTESIAN_POINT('Ctrl Pts',(5.2092443421083,6.50901873038902,-8.60668481503895));
#44277=CARTESIAN_POINT('Ctrl Pts',(5.20826147406231,6.47133598480579,-8.60374314939847));
#44278=CARTESIAN_POINT('Ctrl Pts',(5.20794528621798,6.45921347645598,-8.60279681797445));
#44279=CARTESIAN_POINT('Ctrl Pts',(5.20759766387723,6.44703937354788,-8.60175569533908));
#44280=CARTESIAN_POINT('Ctrl Pts',(5.20721943055202,6.43482153224083,-8.60061767598738));
#44281=CARTESIAN_POINT('Ctrl Pts',(5.20717293371244,6.43331957308106,-8.60047777741232));
#44282=CARTESIAN_POINT('Ctrl Pts',(5.20712597375788,6.43181695506658,-8.60033641779852));
#44283=CARTESIAN_POINT('Ctrl Pts',(5.20707854776624,6.43031369019317,-8.60019360443901));
#44284=CARTESIAN_POINT('Ctrl Pts',(5.20577851568142,6.38910648503552,-8.5962788323262));
#44285=CARTESIAN_POINT('Ctrl Pts',(5.20412386978512,6.34741327362881,-8.59127149360352));
#44286=CARTESIAN_POINT('Ctrl Pts',(5.20208863155282,6.30548216541678,-8.58532297130938));
#44287=CARTESIAN_POINT('Ctrl Pts',(5.19996000458014,6.26162701051749,-8.57910149570916));
#44288=CARTESIAN_POINT('Ctrl Pts',(5.19741530186008,6.21751183338102,-8.5718504727011));
#44289=CARTESIAN_POINT('Ctrl Pts',(5.19448099156681,6.17341777707288,-8.56374594101904));
#44290=CARTESIAN_POINT('Ctrl Pts',(5.1941972595391,6.1691541189196,-8.56296227638308));
#44291=CARTESIAN_POINT('Ctrl Pts',(5.19390992441439,6.16489065499327,-8.56217063370893));
#44292=CARTESIAN_POINT('Ctrl Pts',(5.19361903494277,6.16062763730049,-8.56137117349791));
#44293=CARTESIAN_POINT('Ctrl Pts',(5.1889645568448,6.09241574096818,-8.54857913251516));
#44294=CARTESIAN_POINT('Ctrl Pts',(5.18339170218387,6.02431529261517,-8.53380517569397));
#44295=CARTESIAN_POINT('Ctrl Pts',(5.17695209220329,5.95634040206383,-8.51767149052187));
#44296=CARTESIAN_POINT('Ctrl Pts',(5.17573675136541,5.94351157226104,-8.51462659704009));
#44297=CARTESIAN_POINT('Ctrl Pts',(5.17449040621829,5.93068722455044,-8.51153334083738));
#44298=CARTESIAN_POINT('Ctrl Pts',(5.17321317578403,5.91786749114468,-8.50839599056089));
#44299=CARTESIAN_POINT('Ctrl Pts',(5.17212619654791,5.90695733456609,-8.50572596758343));
#44300=CARTESIAN_POINT('Ctrl Pts',(5.17101684657982,5.89605052010649,-8.50302400883112));
#44301=CARTESIAN_POINT('Ctrl Pts',(5.16988525053059,5.88514714324858,-8.50029275191432));
#44302=CARTESIAN_POINT('Ctrl Pts',(5.16230316750045,5.8120907653105,-8.48199239046117));
#44303=CARTESIAN_POINT('Ctrl Pts',(5.15372750951834,5.73919017115096,-8.46237195280239));
#44304=CARTESIAN_POINT('Ctrl Pts',(5.14431889499684,5.66677187873498,-8.44211748739085));
#44305=CARTESIAN_POINT('Ctrl Pts',(5.14193079042821,5.64839059054679,-8.43697647738624));
#44306=CARTESIAN_POINT('Ctrl Pts',(5.13948886442781,5.63004056205971,-8.43179463827499));
#44307=CARTESIAN_POINT('Ctrl Pts',(5.13699536057964,5.61172763420576,-8.42658313372846));
#44308=CARTESIAN_POINT('Ctrl Pts',(5.12949546600836,5.55664649675454,-8.41090810892934));
#44309=CARTESIAN_POINT('Ctrl Pts',(5.12153284902103,5.50190222651919,-8.39496012661076));
#44310=CARTESIAN_POINT('Ctrl Pts',(5.11322560411293,5.44781430353963,-8.37903587164113));
#44311=CARTESIAN_POINT('Ctrl Pts',(5.10788953745503,5.41307152592815,-8.36880710302587));
#44312=CARTESIAN_POINT('Ctrl Pts',(5.10241161165168,5.37860001522318,-8.35858787364834));
#44313=CARTESIAN_POINT('Ctrl Pts',(5.09683002250716,5.34449059744963,-8.34845164351308));
#44314=CARTESIAN_POINT('Ctrl Pts',(5.08797042045967,5.29034905106899,-8.33236250421331));
#44315=CARTESIAN_POINT('Ctrl Pts',(5.07884119105764,5.23711372307129,-8.31649212545848));
#44316=CARTESIAN_POINT('Ctrl Pts',(5.069511669899,5.18459806022679,-8.30092096452761));
#44317=CARTESIAN_POINT('Ctrl Pts',(5.06381317828989,5.152521380301,-8.29141006590805));
#44318=CARTESIAN_POINT('Ctrl Pts',(5.05803892964553,5.12071336580347,-8.28201092988208));
#44319=CARTESIAN_POINT('Ctrl Pts',(5.05219551521658,5.08913373399478,-8.27274283293787));
#44320=CARTESIAN_POINT('Ctrl Pts',(5.04772070181313,5.06495044844973,-8.2656454406624));
#44321=CARTESIAN_POINT('Ctrl Pts',(5.04320144113992,5.04089952986362,-8.25862713571524));
#44322=CARTESIAN_POINT('Ctrl Pts',(5.03863450812376,5.01690204575399,-8.2516724774818));
#44323=CARTESIAN_POINT('Ctrl Pts',(5.03131471129866,4.97843931652748,-8.24052567828929));
#44324=CARTESIAN_POINT('Ctrl Pts',(5.02387456159545,4.94011435349542,-8.22954086069226));
#44325=CARTESIAN_POINT('Ctrl Pts',(5.01627292819204,4.90159183136664,-8.21867609358834));
#44326=CARTESIAN_POINT('Ctrl Pts',(5.01228433768763,4.88137899580684,-8.21297533105433));
#44327=CARTESIAN_POINT('Ctrl Pts',(5.00825063655086,4.86111159023468,-8.20730808233553));
#44328=CARTESIAN_POINT('Ctrl Pts',(5.00416124115483,4.84074012217289,-8.20167162155164));
#44329=CARTESIAN_POINT('Ctrl Pts',(4.99669364977443,4.80354005111777,-8.19137895432589));
#44330=CARTESIAN_POINT('Ctrl Pts',(4.98903930399197,4.76599468914279,-8.18118853798181));
#44331=CARTESIAN_POINT('Ctrl Pts',(4.98117932932182,4.7278550640792,-8.17108846758484));
#44332=CARTESIAN_POINT('Ctrl Pts',(4.97331935465168,4.6897154390156,-8.16098839718786));
#44333=CARTESIAN_POINT('Ctrl Pts',(4.9652543657701,4.65098125419039,-8.15097822975307));
#44334=CARTESIAN_POINT('Ctrl Pts',(4.95693176799035,4.61139297708926,-8.14108593475121));
#44335=CARTESIAN_POINT('Ctrl Pts',(4.95491385635422,4.6017943340777,-8.13868743157702));
#44336=CARTESIAN_POINT('Ctrl Pts',(4.95288061937741,4.5921454452916,-8.13629605936647));
#44337=CARTESIAN_POINT('Ctrl Pts',(4.95083097602889,4.58244253309453,-8.13391261591468));
#44338=CARTESIAN_POINT('Ctrl Pts',(4.94184067356442,4.53988287728865,-8.12345817389968));
#44339=CARTESIAN_POINT('Ctrl Pts',(4.93254499040935,4.49629030101477,-8.11315052694005));
#44340=CARTESIAN_POINT('Ctrl Pts',(4.92297544431639,4.45162169242285,-8.10312070556636));
#44341=CARTESIAN_POINT('Ctrl Pts',(4.91373348375058,4.40848218349251,-8.09343422590291));
#44342=CARTESIAN_POINT('Ctrl Pts',(4.90423648988793,4.36433828423002,-8.08400699033239));
#44343=CARTESIAN_POINT('Ctrl Pts',(4.8944929279702,4.3191572751814,-8.07500141838257));
#44344=CARTESIAN_POINT('Ctrl Pts',(4.89305231704439,4.31247714569442,-8.07366992118948));
#44345=CARTESIAN_POINT('Ctrl Pts',(4.89160627326198,4.30577436841791,-8.07234772096928));
#44346=CARTESIAN_POINT('Ctrl Pts',(4.89015477736819,4.29904886650588,-8.07103542504457));
#44347=CARTESIAN_POINT('Ctrl Pts',(4.88444745348448,4.27260399824501,-8.06587543946994));
#44348=CARTESIAN_POINT('Ctrl Pts',(4.87865286577492,4.24581034509846,-8.0608695711381));
#44349=CARTESIAN_POINT('Ctrl Pts',(4.87278236715416,4.21865081450186,-8.05605112229944));
#44350=CARTESIAN_POINT('Ctrl Pts',(4.86417516312855,4.17883007078203,-8.04898641197064));
#44351=CARTESIAN_POINT('Ctrl Pts',(4.85540597405651,4.13822187706632,-8.04232278026814));
#44352=CARTESIAN_POINT('Ctrl Pts',(4.84649415516862,4.09678027383868,-8.03619910573178));
#44353=CARTESIAN_POINT('Ctrl Pts',(4.83865735079759,4.06033768659553,-8.03081411755181));
#44354=CARTESIAN_POINT('Ctrl Pts',(4.83071011442131,4.02325035891697,-8.0258473682564));
#44355=CARTESIAN_POINT('Ctrl Pts',(4.82264849588103,3.98550100986324,-8.02141843089699));
#44356=CARTESIAN_POINT('Ctrl Pts',(4.81465734732444,3.94808164367814,-8.01702820873377));
#44357=CARTESIAN_POINT('Ctrl Pts',(4.80654432476385,3.91002527144511,-8.01316842437477));
#44358=CARTESIAN_POINT('Ctrl Pts',(4.79835549762466,3.87129242944051,-8.00996662431293));
#44359=CARTESIAN_POINT('Ctrl Pts',(4.79482934650976,3.85461386831123,-8.00858791272628));
#44360=CARTESIAN_POINT('Ctrl Pts',(4.79128883489312,3.83781012371503,-8.00733171078698));
#44361=CARTESIAN_POINT('Ctrl Pts',(4.78773614681455,3.82087945116332,-8.00621041663226));
#44362=CARTESIAN_POINT('Ctrl Pts',(4.77983289626817,3.78321575985821,-8.00371600438864));
#44363=CARTESIAN_POINT('Ctrl Pts',(4.77187114760531,3.74492163519567,-8.0018874550049));
#44364=CARTESIAN_POINT('Ctrl Pts',(4.76385756247949,3.705998673479,-8.0008822568962));
#44365=CARTESIAN_POINT('Ctrl Pts',(4.75925693393927,3.68365285874913,-8.00030516898425));
#44366=CARTESIAN_POINT('Ctrl Pts',(4.75463874402007,3.66110036062685,-7.99999998526946));
#44367=CARTESIAN_POINT('Ctrl Pts',(4.75000019976002,3.63834723186299,-7.99999998599622));
#44368=CARTESIAN_POINT('',(2.169373137679,3.679332757285,-8.863031548225));
#44369=CARTESIAN_POINT('Origin',(2.169373138313,2.688757347123,-9.));
#44370=CARTESIAN_POINT('',(5.13980281059253,6.65770465916531,-8.87505252673587));
#44371=CARTESIAN_POINT('Origin',(2.10038301328526,6.72679850008447,-8.99999817412645));
#44372=CARTESIAN_POINT('Ctrl Pts',(5.18295251264825,7.29695736715025,-8.53243592896757));
#44373=CARTESIAN_POINT('Ctrl Pts',(5.17654833497352,7.1943406645062,-8.58329263403164));
#44374=CARTESIAN_POINT('Ctrl Pts',(5.1699516725902,7.09359920983857,-8.63567789420594));
#44375=CARTESIAN_POINT('Ctrl Pts',(5.157494193214,6.90937313701787,-8.73460493631109));
#44376=CARTESIAN_POINT('Ctrl Pts',(5.15310666387399,6.84592850506508,-8.76944708099986));
#44377=CARTESIAN_POINT('Ctrl Pts',(5.14396640620889,6.71587927969526,-8.84203148010505));
#44378=CARTESIAN_POINT('Ctrl Pts',(5.14187631370327,6.68681172236822,-8.85857429491814));
#44379=CARTESIAN_POINT('Ctrl Pts',(5.13980325342901,6.65769808278058,-8.87503678322028));
#44380=CARTESIAN_POINT('Ctrl Pts',(5.031171575324,8.155237335624,-8.328092758217));
#44381=CARTESIAN_POINT('Ctrl Pts',(5.038708713357,8.115239371898,-8.340486420358));
#44382=CARTESIAN_POINT('Ctrl Pts',(5.055903779581,8.021823545362,-8.369528270796));
#44383=CARTESIAN_POINT('Ctrl Pts',(5.081440156798,7.873580856051,-8.415449976165));
#44384=CARTESIAN_POINT('Ctrl Pts',(5.107114572603,7.709609696431,-8.465029851269));
#44385=CARTESIAN_POINT('Ctrl Pts',(5.130275638286,7.542561037424,-8.513074805866));
#44386=CARTESIAN_POINT('Ctrl Pts',(5.150590806214,7.370633393346,-8.558423192441));
#44387=CARTESIAN_POINT('Ctrl Pts',(5.167866499439,7.188862495842,-8.599955644047));
#44388=CARTESIAN_POINT('Ctrl Pts',(5.181671783386,6.98691179701,-8.635615603358));
#44389=CARTESIAN_POINT('Ctrl Pts',(5.190015050755,6.752775192089,-8.658681825984));
#44390=CARTESIAN_POINT('Ctrl Pts',(5.188780785953,6.485018200615,-8.655143868828));
#44391=CARTESIAN_POINT('Ctrl Pts',(5.174650084459,6.201354130137,-8.616792553242));
#44392=CARTESIAN_POINT('Ctrl Pts',(5.148239374427,5.917872628893,-8.55261185355));
#44393=CARTESIAN_POINT('Ctrl Pts',(5.111611019512,5.639452557662,-8.474210057388));
#44394=CARTESIAN_POINT('Ctrl Pts',(5.067315842323,5.369156561314,-8.390508586803));
#44395=CARTESIAN_POINT('Ctrl Pts',(5.017976873343,5.108292633657,-8.307637532437));
#44396=CARTESIAN_POINT('Ctrl Pts',(4.964741308491,4.85146302315,-8.227986869471));
#44397=CARTESIAN_POINT('Ctrl Pts',(4.906610173435,4.585932850899,-8.151357345673));
#44398=CARTESIAN_POINT('Ctrl Pts',(4.842079312509,4.298108371584,-8.07947238098));
#44399=CARTESIAN_POINT('Ctrl Pts',(4.771105566726,3.978310550728,-8.019756056663));
#44400=CARTESIAN_POINT('Ctrl Pts',(4.721281427315,3.742419916668,-7.998750565229));
#44401=CARTESIAN_POINT('Ctrl Pts',(4.695191509856,3.613080798913,-7.997107751107));
#44402=CARTESIAN_POINT('Ctrl Pts',(4.692661092446,3.600476016323,-7.997045622421));
#44403=CARTESIAN_POINT('Ctrl Pts',(5.313497515126,8.076389263026,-8.153031867848));
#44404=CARTESIAN_POINT('Ctrl Pts',(5.317534510854,8.033660503279,-8.161010743624));
#44405=CARTESIAN_POINT('Ctrl Pts',(5.326265824451,7.934136921648,-8.179935247545));
#44406=CARTESIAN_POINT('Ctrl Pts',(5.337462630015,7.777617310787,-8.210478293268));
#44407=CARTESIAN_POINT('Ctrl Pts',(5.346478990087,7.607149574909,-8.243740345299));
#44408=CARTESIAN_POINT('Ctrl Pts',(5.352349552748,7.437371290181,-8.275637786151));
#44409=CARTESIAN_POINT('Ctrl Pts',(5.355278570525,7.268196900007,-8.304695219039));
#44410=CARTESIAN_POINT('Ctrl Pts',(5.355687020392,7.097302977515,-8.329452046748));
#44411=CARTESIAN_POINT('Ctrl Pts',(5.354195232211,6.91945862717,-8.347946571836));
#44412=CARTESIAN_POINT('Ctrl Pts',(5.352174075495,6.730414811562,-8.357264936963));
#44413=CARTESIAN_POINT('Ctrl Pts',(5.352554332008,6.524883545689,-8.356085858452));
#44414=CARTESIAN_POINT('Ctrl Pts',(5.355545391982,6.28889745216,-8.339458569343));
#44415=CARTESIAN_POINT('Ctrl Pts',(5.355743304285,6.024221707419,-8.302176740217));
#44416=CARTESIAN_POINT('Ctrl Pts',(5.348567768536,5.745007024714,-8.25096946318));
#44417=CARTESIAN_POINT('Ctrl Pts',(5.332271520057,5.462498551095,-8.194966634583));
#44418=CARTESIAN_POINT('Ctrl Pts',(5.307199470508,5.183786132192,-8.140920516122));
#44419=CARTESIAN_POINT('Ctrl Pts',(5.273996300018,4.906787526201,-8.092132289014));
#44420=CARTESIAN_POINT('Ctrl Pts',(5.231834820217,4.620390772582,-8.05003102277));
#44421=CARTESIAN_POINT('Ctrl Pts',(5.178762545894,4.312871161624,-8.018232907273));
#44422=CARTESIAN_POINT('Ctrl Pts',(5.113457189332,3.978364205831,-8.00511529044));
#44423=CARTESIAN_POINT('Ctrl Pts',(5.062572556357,3.740423131644,-8.01837619026));
#44424=CARTESIAN_POINT('Ctrl Pts',(5.034564290784,3.613522785182,-8.03453190803));
#44425=CARTESIAN_POINT('Ctrl Pts',(5.031834968443,3.601189986531,-8.036192956447));
#44426=CARTESIAN_POINT('Ctrl Pts',(5.343715148193,7.936726246008,-7.842947387839));
#44427=CARTESIAN_POINT('Ctrl Pts',(5.341552423568,7.892678299717,-7.8509163253));
#44428=CARTESIAN_POINT('Ctrl Pts',(5.335836718102,7.790705225447,-7.86998804917));
#44429=CARTESIAN_POINT('Ctrl Pts',(5.324457252268,7.632826661304,-7.901227441035));
#44430=CARTESIAN_POINT('Ctrl Pts',(5.309356049496,7.464506176445,-7.935456809141));
#44431=CARTESIAN_POINT('Ctrl Pts',(5.29203668893,7.301307301607,-7.968041021536));
#44432=CARTESIAN_POINT('Ctrl Pts',(5.273219125013,7.14428292257,-7.996958180074));
#44433=CARTESIAN_POINT('Ctrl Pts',(5.253815840562,6.993090308133,-8.020196513283));
#44434=CARTESIAN_POINT('Ctrl Pts',(5.235340681084,6.846770386955,-8.035318131012));
#44435=CARTESIAN_POINT('Ctrl Pts',(5.222346509965,6.707286169975,-8.040470406053));
#44436=CARTESIAN_POINT('Ctrl Pts',(5.224401525058,6.56633478398,-8.040118999002));
#44437=CARTESIAN_POINT('Ctrl Pts',(5.245703537717,6.385473319824,-8.029564849193));
#44438=CARTESIAN_POINT('Ctrl Pts',(5.27671001174,6.153667134501,-7.995362006865));
#44439=CARTESIAN_POINT('Ctrl Pts',(5.307543849893,5.889969376952,-7.943666866687));
#44440=CARTESIAN_POINT('Ctrl Pts',(5.33238773401,5.610077285361,-7.886145647549));
#44441=CARTESIAN_POINT('Ctrl Pts',(5.348757652582,5.324444421342,-7.831644909872));
#44442=CARTESIAN_POINT('Ctrl Pts',(5.356373795317,5.03314145169,-7.7847870628));
#44443=CARTESIAN_POINT('Ctrl Pts',(5.35504567828,4.725491437746,-7.748168605561));
#44444=CARTESIAN_POINT('Ctrl Pts',(5.343331751932,4.389196488746,-7.727282197562));
#44445=CARTESIAN_POINT('Ctrl Pts',(5.319122436767,4.018254298991,-7.733197090829));
#44446=CARTESIAN_POINT('Ctrl Pts',(5.293895775961,3.752329054664,-7.766551305318));
#44447=CARTESIAN_POINT('Ctrl Pts',(5.278459817194,3.610625652574,-7.79561095396));
#44448=CARTESIAN_POINT('Ctrl Pts',(5.276941725209,3.596855779951,-7.798547106358));
#44449=CARTESIAN_POINT('Ctrl Pts',(5.099664136616,7.838671252106,-7.625242200552));
#44450=CARTESIAN_POINT('Ctrl Pts',(5.093148727071,7.795683164535,-7.637613336092));
#44451=CARTESIAN_POINT('Ctrl Pts',(5.077597570703,7.696715214695,-7.666988881474));
#44452=CARTESIAN_POINT('Ctrl Pts',(5.051961619203,7.545392264572,-7.71448895437));
#44453=CARTESIAN_POINT('Ctrl Pts',(5.022970150104,7.386288154655,-7.766261388878));
#44454=CARTESIAN_POINT('Ctrl Pts',(4.993567957957,7.234152663538,-7.815863008815));
#44455=CARTESIAN_POINT('Ctrl Pts',(4.964591406833,7.08976474703,-7.860893443632));
#44456=CARTESIAN_POINT('Ctrl Pts',(4.936960987655,6.952649665104,-7.898984011573));
#44457=CARTESIAN_POINT('Ctrl Pts',(4.912271046082,6.822153566707,-7.926998796839));
#44458=CARTESIAN_POINT('Ctrl Pts',(4.895742416311,6.700350837807,-7.940621984007));
#44459=CARTESIAN_POINT('Ctrl Pts',(4.898304229926,6.578973325192,-7.938960061882));
#44460=CARTESIAN_POINT('Ctrl Pts',(4.925677905901,6.420257064082,-7.914374379919));
#44461=CARTESIAN_POINT('Ctrl Pts',(4.969099180964,6.211279092219,-7.857172641533));
#44462=CARTESIAN_POINT('Ctrl Pts',(5.018624475667,5.968030337843,-7.777665034204));
#44463=CARTESIAN_POINT('Ctrl Pts',(5.067579257769,5.703664743327,-7.690521915594));
#44464=CARTESIAN_POINT('Ctrl Pts',(5.112174401207,5.427114642955,-7.606620402143));
#44465=CARTESIAN_POINT('Ctrl Pts',(5.151461612933,5.137862158608,-7.531345219964));
#44466=CARTESIAN_POINT('Ctrl Pts',(5.185885099729,4.824158450321,-7.467143262251));
#44467=CARTESIAN_POINT('Ctrl Pts',(5.215098814274,4.471110576435,-7.419991233884));
#44468=CARTESIAN_POINT('Ctrl Pts',(5.23727508881,4.068727117922,-7.4034147995));
#44469=CARTESIAN_POINT('Ctrl Pts',(5.245608391033,3.76940638382,-7.427953662365));
#44470=CARTESIAN_POINT('Ctrl Pts',(5.248015394314,3.606514035979,-7.455559442076));
#44471=CARTESIAN_POINT('Ctrl Pts',(5.248230402702,3.590651920927,-7.458387517839));
#44472=CARTESIAN_POINT('',(5.246082198634,7.96024107558274,-8.031111952023));
#44473=CARTESIAN_POINT('Ctrl Pts',(5.246082198634,7.960241075785,-8.031111952023));
#44474=CARTESIAN_POINT('Ctrl Pts',(5.24531416124,7.961564936488,-8.037211072505));
#44475=CARTESIAN_POINT('Ctrl Pts',(5.243746788157,7.960077213467,-8.049657858755));
#44476=CARTESIAN_POINT('Ctrl Pts',(5.241420859859,7.951438324206,-8.068128465827));
#44477=CARTESIAN_POINT('Ctrl Pts',(5.239201509839,7.939491726482,-8.085752715982));
#44478=CARTESIAN_POINT('Ctrl Pts',(5.236885850808,7.924335625739,-8.104141772995));
#44479=CARTESIAN_POINT('Ctrl Pts',(5.234470453135,7.906262887624,-8.123322872162));
#44480=CARTESIAN_POINT('Ctrl Pts',(5.232015563957,7.886079705568,-8.142817580344));
#44481=CARTESIAN_POINT('Ctrl Pts',(5.229553400312,7.864393101416,-8.16237005635));
#44482=CARTESIAN_POINT('Ctrl Pts',(5.226947781756,7.84014329634,-8.183061733116));
#44483=CARTESIAN_POINT('Ctrl Pts',(5.224222732637,7.813560756387,-8.20470182906));
#44484=CARTESIAN_POINT('Ctrl Pts',(5.221362028258,7.784508545691,-8.22741918737));
#44485=CARTESIAN_POINT('Ctrl Pts',(5.218362980801,7.752937676919,-8.251235152442));
#44486=CARTESIAN_POINT('Ctrl Pts',(5.215224251798,7.718786278869,-8.276160353447));
#44487=CARTESIAN_POINT('Ctrl Pts',(5.211941467388,7.681930867577,-8.302229523409));
#44488=CARTESIAN_POINT('Ctrl Pts',(5.208473403288,7.641774422659,-8.329770033749));
#44489=CARTESIAN_POINT('Ctrl Pts',(5.204791140956,7.5977585816,-8.35901152383));
#44490=CARTESIAN_POINT('Ctrl Pts',(5.200873339775,7.549273843232,-8.390123492704));
#44491=CARTESIAN_POINT('Ctrl Pts',(5.196708849019,7.495676152098,-8.423194380345));
#44492=CARTESIAN_POINT('Ctrl Pts',(5.192299032893,7.436264363619,-8.45821376354));
#44493=CARTESIAN_POINT('Ctrl Pts',(5.187673532847,7.370324268216,-8.494944723498));
#44494=CARTESIAN_POINT('Ctrl Pts',(5.184525962137,7.322165181379,-8.51994250699));
#44495=CARTESIAN_POINT('Ctrl Pts',(5.182952650723,7.296957647765,-8.532436450571));
#44496=CARTESIAN_POINT('Origin',(4.69181087540435,7.94978071640467,-7.96462206846104));
#44497=CARTESIAN_POINT('Origin',(4.75,10.48573680623,-7.968642341825));
#44498=CARTESIAN_POINT('',(5.246082198634,10.41979065289,-8.031111952022));
#44499=CARTESIAN_POINT('',(5.246082198634,7.960241075785,-8.031111952023));
#44500=CARTESIAN_POINT('Origin',(4.75,10.41979065293,-7.968642341825));
#44501=CARTESIAN_POINT('Ctrl Pts',(5.24583498938,10.46559780792,-8.030265711223));
#44502=CARTESIAN_POINT('Ctrl Pts',(5.24583498938,10.46530050489,-8.030301692655));
#44503=CARTESIAN_POINT('Ctrl Pts',(5.245834989379,10.46004562112,-8.030931668211));
#44504=CARTESIAN_POINT('Ctrl Pts',(5.245834989331,10.4498027854,-8.03195283292));
#44505=CARTESIAN_POINT('Ctrl Pts',(5.245834989351,10.43481488829,-8.032844402977));
#44506=CARTESIAN_POINT('Ctrl Pts',(5.245834989345,10.42449916127,-8.033050835857));
#44507=CARTESIAN_POINT('Ctrl Pts',(5.245834989346,10.41918940524,-8.033044320572));
#44508=CARTESIAN_POINT('Ctrl Pts',(5.245834989346,10.41888877729,-8.033043589861));
#44509=CARTESIAN_POINT('Ctrl Pts',(5.248664215617,10.46298074913,-8.008641229529));
#44510=CARTESIAN_POINT('Ctrl Pts',(5.248664215617,10.46270014925,-8.008675189523));
#44511=CARTESIAN_POINT('Ctrl Pts',(5.248664215617,10.45774061605,-8.009269768448));
#44512=CARTESIAN_POINT('Ctrl Pts',(5.248664215601,10.44807755293,-8.01023338741));
#44513=CARTESIAN_POINT('Ctrl Pts',(5.248664215608,10.43394801199,-8.011073679399));
#44514=CARTESIAN_POINT('Ctrl Pts',(5.248664215606,10.42422714206,-8.011268221533));
#44515=CARTESIAN_POINT('Ctrl Pts',(5.248664215606,10.41922413839,-8.011262073099));
#44516=CARTESIAN_POINT('Ctrl Pts',(5.248664215606,10.41894087986,-8.011261383974));
#44517=CARTESIAN_POINT('Ctrl Pts',(5.250054025977,10.46034699506,-7.986878796461));
#44518=CARTESIAN_POINT('Ctrl Pts',(5.250054025977,10.46008320489,-7.986910722122));
#44519=CARTESIAN_POINT('Ctrl Pts',(5.250054025977,10.45542090641,-7.987469678606));
#44520=CARTESIAN_POINT('Ctrl Pts',(5.250054025978,10.44634131451,-7.988375384713));
#44521=CARTESIAN_POINT('Ctrl Pts',(5.250054025978,10.43307560553,-7.989164071509));
#44522=CARTESIAN_POINT('Ctrl Pts',(5.250054025978,10.42395338754,-7.989346647043));
#44523=CARTESIAN_POINT('Ctrl Pts',(5.250054025978,10.41925909312,-7.9893408678));
#44524=CARTESIAN_POINT('Ctrl Pts',(5.250054025978,10.41899331481,-7.989340220527));
#44525=CARTESIAN_POINT('Ctrl Pts',(5.249998396461,10.45770796146,-7.965072739197));
#44526=CARTESIAN_POINT('Ctrl Pts',(5.249998396461,10.45746101469,-7.965102626446));
#44527=CARTESIAN_POINT('Ctrl Pts',(5.249998396461,10.45309654676,-7.965625889082));
#44528=CARTESIAN_POINT('Ctrl Pts',(5.249998396461,10.44460159568,-7.966473566244));
#44529=CARTESIAN_POINT('Ctrl Pts',(5.249998396461,10.43220145028,-7.967210544403));
#44530=CARTESIAN_POINT('Ctrl Pts',(5.249998396461,10.42367908425,-7.967381129347));
#44531=CARTESIAN_POINT('Ctrl Pts',(5.249998396461,10.41929411792,-7.967375720036));
#44532=CARTESIAN_POINT('Ctrl Pts',(5.249998396461,10.41904585488,-7.967375114698));
#44533=CARTESIAN_POINT('',(5.24599641608878,10.4645576409889,-8.02912516883275));
#44534=CARTESIAN_POINT('Ctrl Pts',(5.245996542241,10.46455752845,-8.029125198361));
#44535=CARTESIAN_POINT('Ctrl Pts',(5.2460120432,10.4595955694,-8.029591626281));
#44536=CARTESIAN_POINT('Ctrl Pts',(5.246039094108,10.44966467169,-8.030367134869));
#44537=CARTESIAN_POINT('Ctrl Pts',(5.246067839312,10.43474154707,-8.031026583047));
#44538=CARTESIAN_POINT('Ctrl Pts',(5.246078758439,10.424776975,-8.031139333386));
#44539=CARTESIAN_POINT('Ctrl Pts',(5.246082198634,10.41979065289,-8.031111952022));
#44540=CARTESIAN_POINT('Origin',(4.750000004037,10.4571165168,-7.96641902307));
#44541=CARTESIAN_POINT('Origin',(8.197306954564,11.98889246271,39.41676));
#44542=CARTESIAN_POINT('',(4.23,10.15082771808,-16.1));
#44543=CARTESIAN_POINT('',(5.246082198634,10.41979065289,-8.031111952022));
#44544=CARTESIAN_POINT('',(1.218893149689,13.14,-16.1));
#44545=CARTESIAN_POINT('Origin',(1.2063075471585,10.1383337960431,-16.1));
#44546=CARTESIAN_POINT('',(2.23784458253126,13.4097224533938,-8.00832639825692));
#44547=CARTESIAN_POINT('',(2.237844640648,13.40972245349,-8.008326395313));
#44548=CARTESIAN_POINT('',(2.25070091824063,13.4097088030271,-8.00792916996587));
#44549=CARTESIAN_POINT('Ctrl Pts',(2.237844640648,13.4097224534935,-8.00832639531314));
#44550=CARTESIAN_POINT('Ctrl Pts',(2.23927596418,13.4097214685921,-8.00835594235443));
#44551=CARTESIAN_POINT('Ctrl Pts',(2.24070638414192,13.409720288815,-8.00836088798532));
#44552=CARTESIAN_POINT('Ctrl Pts',(2.242134536513,13.4097189970496,-8.00833938734947));
#44553=CARTESIAN_POINT('Ctrl Pts',(2.24356268888409,13.4097177052841,-8.00831788671363));
#44554=CARTESIAN_POINT('Ctrl Pts',(2.24498857359248,13.4097163045634,-8.0082699399031));
#44555=CARTESIAN_POINT('Ctrl Pts',(2.24641625272802,13.4097145733304,-8.00820227825647));
#44556=CARTESIAN_POINT('Ctrl Pts',(2.24784393186355,13.4097128420974,-8.00813461660984));
#44557=CARTESIAN_POINT('Ctrl Pts',(2.24927340557576,13.4097107742197,-8.00804723994156));
#44558=CARTESIAN_POINT('Ctrl Pts',(2.25069783394685,13.4097088006893,-8.00792869483126));
#44559=CARTESIAN_POINT('',(3.726652166637,12.93059538988,-8.835890668796));
#44560=CARTESIAN_POINT('Ctrl Pts',(3.72665216664103,12.9305953898865,-8.83589066879675));
#44561=CARTESIAN_POINT('Ctrl Pts',(3.67915834207035,12.9615640469669,-8.82131895211287));
#44562=CARTESIAN_POINT('Ctrl Pts',(3.62945060498817,12.9922562972525,-8.80384623652916));
#44563=CARTESIAN_POINT('Ctrl Pts',(3.57741786220796,13.0223335068074,-8.78336557823536));
#44564=CARTESIAN_POINT('Ctrl Pts',(3.54859552520211,13.0389940828921,-8.7720207902441));
#44565=CARTESIAN_POINT('Ctrl Pts',(3.51906017611917,13.0554651496962,-8.75975308160159));
#44566=CARTESIAN_POINT('Ctrl Pts',(3.48879640079114,13.0716831311055,-8.74654451168046));
#44567=CARTESIAN_POINT('Ctrl Pts',(3.43564340987221,13.1001671589318,-8.72334598507696));
#44568=CARTESIAN_POINT('Ctrl Pts',(3.38024111998694,13.1278688643674,-8.69724485914804));
#44569=CARTESIAN_POINT('Ctrl Pts',(3.32267013814449,13.1543499903996,-8.6683223432563));
#44570=CARTESIAN_POINT('Ctrl Pts',(3.2882857383413,13.1701659031319,-8.65104830487951));
#44571=CARTESIAN_POINT('Ctrl Pts',(3.2531286892389,13.1855463882986,-8.63276796561064));
#44572=CARTESIAN_POINT('Ctrl Pts',(3.21722500639134,13.2003987422202,-8.61349976246249));
#44573=CARTESIAN_POINT('Ctrl Pts',(3.1662961337491,13.2214665988108,-8.58616808542137));
#44574=CARTESIAN_POINT('Ctrl Pts',(3.1138624144285,13.2414693868998,-8.55684832417649));
#44575=CARTESIAN_POINT('Ctrl Pts',(3.0601161068077,13.260114095891,-8.5257623363328));
#44576=CARTESIAN_POINT('Ctrl Pts',(3.01253212736738,13.276621080065,-8.49824053861466));
#44577=CARTESIAN_POINT('Ctrl Pts',(2.96391993758325,13.2920637610469,-8.46933439956908));
#44578=CARTESIAN_POINT('Ctrl Pts',(2.9144358224046,13.3062639442575,-8.43920159758119));
#44579=CARTESIAN_POINT('Ctrl Pts',(2.86519697669492,13.3203937438433,-8.40921814971057));
#44580=CARTESIAN_POINT('Ctrl Pts',(2.815090644569,13.3332926101047,-8.3780196179234));
#44581=CARTESIAN_POINT('Ctrl Pts',(2.76435866544655,13.3447958777846,-8.34589203270953));
#44582=CARTESIAN_POINT('Ctrl Pts',(2.7140258684057,13.3562086325687,-8.31401724181916));
#44583=CARTESIAN_POINT('Ctrl Pts',(2.66307764286107,13.3662474711529,-8.28122800576709));
#44584=CARTESIAN_POINT('Ctrl Pts',(2.61176745742015,13.3747999263361,-8.24780744521448));
#44585=CARTESIAN_POINT('Ctrl Pts',(2.60411434570424,13.3760755579558,-8.24282263993031));
#44586=CARTESIAN_POINT('Ctrl Pts',(2.59645320634571,13.377318213237,-8.23782379581316));
#44587=CARTESIAN_POINT('Ctrl Pts',(2.5887849046406,13.3785276155587,-8.23281185858658));
#44588=CARTESIAN_POINT('Ctrl Pts',(2.53100835148655,13.3876398153921,-8.19504959143641));
#44589=CARTESIAN_POINT('Ctrl Pts',(2.47282352961947,13.3948688395409,-8.15654399260822));
#44590=CARTESIAN_POINT('Ctrl Pts',(2.41410614342739,13.4001530742437,-8.11740588425265));
#44591=CARTESIAN_POINT('Ctrl Pts',(2.36011830391961,13.4050116763301,-8.08142025802558));
#44592=CARTESIAN_POINT('Ctrl Pts',(2.30567988186774,13.4082256836511,-8.04489985185588));
#44593=CARTESIAN_POINT('Ctrl Pts',(2.25070017668898,13.4097087374959,-8.00793027014345));
#44594=CARTESIAN_POINT('',(4.7344035079452,11.9058908155723,-8.81635043036525));
#44595=CARTESIAN_POINT('Ctrl Pts',(4.73440331546188,11.9058911216399,-8.81635051243198));
#44596=CARTESIAN_POINT('Ctrl Pts',(4.72046359241685,11.9278363177059,-8.82320870877306));
#44597=CARTESIAN_POINT('Ctrl Pts',(4.7062389061123,11.9498000076889,-8.82931631968062));
#44598=CARTESIAN_POINT('Ctrl Pts',(4.69171471142633,11.9717443529647,-8.83473627246239));
#44599=CARTESIAN_POINT('Ctrl Pts',(4.67828510618429,11.99203490268,-8.83974776038744));
#44600=CARTESIAN_POINT('Ctrl Pts',(4.66459968347873,12.0123086348396,-8.84417132437756));
#44601=CARTESIAN_POINT('Ctrl Pts',(4.65066152519305,12.0325405172014,-8.84810350783152));
#44602=CARTESIAN_POINT('Ctrl Pts',(4.64952548577476,12.034189531038,-8.84842400321635));
#44603=CARTESIAN_POINT('Ctrl Pts',(4.64838777480505,12.0358382710313,-8.84874126192524));
#44604=CARTESIAN_POINT('Ctrl Pts',(4.64724839785379,12.0374867260297,-8.8490553512748));
#44605=CARTESIAN_POINT('Ctrl Pts',(4.63345522748258,12.0574427384952,-8.85285768193062));
#44606=CARTESIAN_POINT('Ctrl Pts',(4.61941151381701,12.0773644259773,-8.85619092406822));
#44607=CARTESIAN_POINT('Ctrl Pts',(4.60512837445064,12.0971888001718,-8.85911085637126));
#44608=CARTESIAN_POINT('Ctrl Pts',(4.59086993131378,12.1169788970774,-8.86202573997202));
#44609=CARTESIAN_POINT('Ctrl Pts',(4.57637312672951,12.1366716679523,-8.86452897702727));
#44610=CARTESIAN_POINT('Ctrl Pts',(4.56164792893267,12.1562358343136,-8.86671785975084));
#44611=CARTESIAN_POINT('Ctrl Pts',(4.55878778915275,12.1600358681904,-8.86714301604671));
#44612=CARTESIAN_POINT('Ctrl Pts',(4.5559190227764,12.163831153263,-8.86755643208473));
#44613=CARTESIAN_POINT('Ctrl Pts',(4.55304168486563,12.1676216115795,-8.86795898918841));
#44614=CARTESIAN_POINT('Ctrl Pts',(4.53769059338692,12.1878443571057,-8.87010670041163));
#44615=CARTESIAN_POINT('Ctrl Pts',(4.52209512389882,12.2079306785399,-8.87193658943113));
#44616=CARTESIAN_POINT('Ctrl Pts',(4.50625622100327,12.2278491180283,-8.87351233966313));
#44617=CARTESIAN_POINT('Ctrl Pts',(4.49028964446776,12.2479281153336,-8.87510079164405));
#44618=CARTESIAN_POINT('Ctrl Pts',(4.47407608664396,12.2678366101076,-8.87643124991651));
#44619=CARTESIAN_POINT('Ctrl Pts',(4.45759282280626,12.2875811900474,-8.87759645773072));
#44620=CARTESIAN_POINT('Ctrl Pts',(4.45577719067703,12.2897560562675,-8.87772480541511));
#44621=CARTESIAN_POINT('Ctrl Pts',(4.45395825915881,12.291928970625,-8.87785117276641));
#44622=CARTESIAN_POINT('Ctrl Pts',(4.4521359772108,12.2940999687377,-8.87797570142284));
#44623=CARTESIAN_POINT('Ctrl Pts',(4.43445589041851,12.3151633585722,-8.87918389944961));
#44624=CARTESIAN_POINT('Ctrl Pts',(4.4164667575051,12.3360422242232,-8.8802047942972));
#44625=CARTESIAN_POINT('Ctrl Pts',(4.39819560771196,12.3566931431443,-8.88110001445564));
#44626=CARTESIAN_POINT('Ctrl Pts',(4.3805268560358,12.3766632031807,-8.88196571928834));
#44627=CARTESIAN_POINT('Ctrl Pts',(4.36259376952211,12.3964215516007,-8.8827145160085));
#44628=CARTESIAN_POINT('Ctrl Pts',(4.34438633829058,12.4159560389645,-8.88338663468743));
#44629=CARTESIAN_POINT('Ctrl Pts',(4.32470005956646,12.4370771602303,-8.88411334431939));
#44630=CARTESIAN_POINT('Ctrl Pts',(4.30470347925626,12.4579273790388,-8.88474555950459));
#44631=CARTESIAN_POINT('Ctrl Pts',(4.28442669500039,12.4784916687152,-8.88529467544084));
#44632=CARTESIAN_POINT('Ctrl Pts',(4.26655693998259,12.4966147997795,-8.88577860657772));
#44633=CARTESIAN_POINT('Ctrl Pts',(4.24846816043806,12.5145167582446,-8.88619719033868));
#44634=CARTESIAN_POINT('Ctrl Pts',(4.23017503613097,12.5321747993092,-8.8865275870937));
#44635=CARTESIAN_POINT('Ctrl Pts',(4.21022196148984,12.5514351621353,-8.88688796463247));
#44636=CARTESIAN_POINT('Ctrl Pts',(4.19003223173258,12.5703973128709,-8.88715309162067));
#44637=CARTESIAN_POINT('Ctrl Pts',(4.16959551499735,12.5890931961295,-8.88725343204916));
#44638=CARTESIAN_POINT('Ctrl Pts',(4.15003538727033,12.6069871596876,-8.88734946859078));
#44639=CARTESIAN_POINT('Ctrl Pts',(4.13024816422848,12.6246370788773,-8.88729400526859));
#44640=CARTESIAN_POINT('Ctrl Pts',(4.11025201335401,12.64203511309,-8.88702649602809));
#44641=CARTESIAN_POINT('Ctrl Pts',(4.08980779776577,12.6598229945922,-8.8867529925614));
#44642=CARTESIAN_POINT('Ctrl Pts',(4.06914411961136,12.6773454967263,-8.88626497991193));
#44643=CARTESIAN_POINT('Ctrl Pts',(4.04826969194302,12.694604597329,-8.88544282470021));
#44644=CARTESIAN_POINT('Ctrl Pts',(4.02845058586471,12.7109911517819,-8.88466223413203));
#44645=CARTESIAN_POINT('Ctrl Pts',(4.00844178534803,12.7271396854217,-8.88358014043497));
#44646=CARTESIAN_POINT('Ctrl Pts',(3.9882911131021,12.7430341197216,-8.88212228680299));
#44647=CARTESIAN_POINT('Ctrl Pts',(3.98721813638,12.7438804616107,-8.88204465946668));
#44648=CARTESIAN_POINT('Ctrl Pts',(3.98614476663789,12.744726079807,-8.88196597418561));
#44649=CARTESIAN_POINT('Ctrl Pts',(3.98507101418444,12.7455709708424,-8.88188622231604));
#44650=CARTESIAN_POINT('Ctrl Pts',(3.96573616424763,12.76078475809,-8.88045014603486));
#44651=CARTESIAN_POINT('Ctrl Pts',(3.94626957299195,12.7757655486749,-8.87867191548715));
#44652=CARTESIAN_POINT('Ctrl Pts',(3.92671322249069,12.7904833419625,-8.87644838982425));
#44653=CARTESIAN_POINT('Ctrl Pts',(3.90724135054377,12.8051375580557,-8.87423446923738));
#44654=CARTESIAN_POINT('Ctrl Pts',(3.88768089863728,12.8195308037399,-8.87157880919055));
#44655=CARTESIAN_POINT('Ctrl Pts',(3.86810143765954,12.8336381217342,-8.86842314569923));
#44656=CARTESIAN_POINT('Ctrl Pts',(3.86414329506343,12.8364900274294,-8.86778520341378));
#44657=CARTESIAN_POINT('Ctrl Pts',(3.86018445518521,12.8393302693263,-8.86712697652388));
#44658=CARTESIAN_POINT('Ctrl Pts',(3.8562256065573,12.8421586760638,-8.8664482126833));
#44659=CARTESIAN_POINT('Ctrl Pts',(3.83591435037889,12.8566700906745,-8.86296574908175));
#44660=CARTESIAN_POINT('Ctrl Pts',(3.81559298551218,12.8708755481986,-8.85893634747914));
#44661=CARTESIAN_POINT('Ctrl Pts',(3.79528162573602,12.8847698834918,-8.85425917623451));
#44662=CARTESIAN_POINT('Ctrl Pts',(3.77365563981166,12.8995635114316,-8.84927928120942));
#44663=CARTESIAN_POINT('Ctrl Pts',(3.75204127377548,12.9140042816332,-8.84356550746721));
#44664=CARTESIAN_POINT('Ctrl Pts',(3.73046143290345,12.9281088821324,-8.83704931856408));
#44665=CARTESIAN_POINT('Ctrl Pts',(3.72919155762041,12.9289388735886,-8.83666587054531));
#44666=CARTESIAN_POINT('Ctrl Pts',(3.7279218007954,12.9297677075523,-8.83627965703763));
#44667=CARTESIAN_POINT('Ctrl Pts',(3.72665216663739,12.9305953898806,-8.83589066879607));
#44668=CARTESIAN_POINT('Ctrl Pts',(5.24599603643705,10.464557593822,-8.02912518352156));
#44669=CARTESIAN_POINT('Ctrl Pts',(5.23960886297041,10.5293098253969,-8.0719644400836));
#44670=CARTESIAN_POINT('Ctrl Pts',(5.23114313036524,10.59324216141,-8.11397625912077));
#44671=CARTESIAN_POINT('Ctrl Pts',(5.22071935566554,10.6565502380626,-8.15506706152508));
#44672=CARTESIAN_POINT('Ctrl Pts',(5.2149946266579,10.6913189848239,-8.17763409844285));
#44673=CARTESIAN_POINT('Ctrl Pts',(5.20867842486534,10.7258993816846,-8.19992372898681));
#44674=CARTESIAN_POINT('Ctrl Pts',(5.20178440999674,10.7603234534577,-8.22192239442965));
#44675=CARTESIAN_POINT('Ctrl Pts',(5.19952708631644,10.7715950091284,-8.22912546976175));
#44676=CARTESIAN_POINT('Ctrl Pts',(5.19720777914531,10.782849802605,-8.23629735666203));
#44677=CARTESIAN_POINT('Ctrl Pts',(5.19482671544939,10.7940886657919,-8.24343732543202));
#44678=CARTESIAN_POINT('Ctrl Pts',(5.18426817063287,10.8439260728501,-8.27509867089527));
#44679=CARTESIAN_POINT('Ctrl Pts',(5.17248884820929,10.8934529095174,-8.30614206762962));
#44680=CARTESIAN_POINT('Ctrl Pts',(5.15960538071716,10.9423981591268,-8.33629953697301));
#44681=CARTESIAN_POINT('Ctrl Pts',(5.14750737623479,10.988359376441,-8.36461840373122));
#44682=CARTESIAN_POINT('Ctrl Pts',(5.13443630744655,11.0338077140869,-8.39215581953822));
#44683=CARTESIAN_POINT('Ctrl Pts',(5.12052994224784,11.0785214063487,-8.41872107326711));
#44684=CARTESIAN_POINT('Ctrl Pts',(5.1196270714083,11.0814244430728,-8.4204458225164));
#44685=CARTESIAN_POINT('Ctrl Pts',(5.11872069317206,11.0843243841839,-8.4221664860781));
#44686=CARTESIAN_POINT('Ctrl Pts',(5.11781085086665,11.087221169466,-8.42388301697232));
#44687=CARTESIAN_POINT('Ctrl Pts',(5.11529940807314,11.0952171820476,-8.42862116677971));
#44688=CARTESIAN_POINT('Ctrl Pts',(5.11276156857949,11.1031891491766,-8.43332782524898));
#44689=CARTESIAN_POINT('Ctrl Pts',(5.11019821719763,11.1111358016278,-8.4380018702359));
#44690=CARTESIAN_POINT('Ctrl Pts',(5.09292366871355,11.164688675427,-8.4695004846338));
#44691=CARTESIAN_POINT('Ctrl Pts',(5.07448826746994,11.2170967576868,-8.49951672097186));
#44692=CARTESIAN_POINT('Ctrl Pts',(5.05506589859061,11.268305622478,-8.52793313715213));
#44693=CARTESIAN_POINT('Ctrl Pts',(5.03928099584317,11.3099239727193,-8.55102766123532));
#44694=CARTESIAN_POINT('Ctrl Pts',(5.02284437489363,11.3507503323974,-8.57306654332118));
#44695=CARTESIAN_POINT('Ctrl Pts',(5.00585320087564,11.3907578171497,-8.59401165357297));
#44696=CARTESIAN_POINT('Ctrl Pts',(5.00377937125237,11.3956408644861,-8.59656807433924));
#44697=CARTESIAN_POINT('Ctrl Pts',(5.00169728428527,11.4005117154219,-8.59910822742005));
#44698=CARTESIAN_POINT('Ctrl Pts',(4.99960711231283,11.4053703106247,-8.60163199358955));
#44699=CARTESIAN_POINT('Ctrl Pts',(4.98127182930402,11.4479905922306,-8.62377082598037));
#44700=CARTESIAN_POINT('Ctrl Pts',(4.96231162670814,11.4896666639454,-8.64465675792625));
#44701=CARTESIAN_POINT('Ctrl Pts',(4.94287797767578,11.5302992819331,-8.6642046388798));
#44702=CARTESIAN_POINT('Ctrl Pts',(4.92335358393126,11.5711216324418,-8.68384379794728));
#44703=CARTESIAN_POINT('Ctrl Pts',(4.9033514176432,11.6108907593272,-8.70213236529609));
#44704=CARTESIAN_POINT('Ctrl Pts',(4.88304043862665,11.6495118066644,-8.71903408269427));
#44705=CARTESIAN_POINT('Ctrl Pts',(4.88030099105452,11.6547208285571,-8.72131370538767));
#44706=CARTESIAN_POINT('Ctrl Pts',(4.87755594704801,11.6599089739279,-8.72356817353367));
#44707=CARTESIAN_POINT('Ctrl Pts',(4.87480574064037,11.6650760180154,-8.72579746713904));
#44708=CARTESIAN_POINT('Ctrl Pts',(4.87364799763581,11.6672511671715,-8.72673592363798));
#44709=CARTESIAN_POINT('Ctrl Pts',(4.87248933984689,11.6694225769385,-8.72766991907993));
#44710=CARTESIAN_POINT('Ctrl Pts',(4.8713298016431,11.6715902270508,-8.72859944240856));
#44711=CARTESIAN_POINT('Ctrl Pts',(4.84830268699342,11.7146373017335,-8.7470587223081));
#44712=CARTESIAN_POINT('Ctrl Pts',(4.82492692307448,11.756209583914,-8.76374501041384));
#44713=CARTESIAN_POINT('Ctrl Pts',(4.80134248448596,11.796368798876,-8.77870090903335));
#44714=CARTESIAN_POINT('Ctrl Pts',(4.77918216802678,11.8341030408412,-8.7927537110577));
#44715=CARTESIAN_POINT('Ctrl Pts',(4.75683730732651,11.8705900200991,-8.80528012543115));
#44716=CARTESIAN_POINT('Ctrl Pts',(4.73440350757872,11.9058908193334,-8.81635041762902));
#44717=CARTESIAN_POINT('Ctrl Pts',(5.24405860277,10.41841896918,-8.057679818181));
#44718=CARTESIAN_POINT('Ctrl Pts',(5.235172178155,10.52502830086,-8.128371564553));
#44719=CARTESIAN_POINT('Ctrl Pts',(5.20530028371,10.74104647072,-8.270140627685));
#44720=CARTESIAN_POINT('Ctrl Pts',(5.125913608767,11.05967157546,-8.468059100874));
#44721=CARTESIAN_POINT('Ctrl Pts',(5.016041643698,11.36413136551,-8.639703681194));
#44722=CARTESIAN_POINT('Ctrl Pts',(4.886112276442,11.64063777194,-8.773600837921));
#44723=CARTESIAN_POINT('Ctrl Pts',(4.781666447384,11.8219539015,-8.842625516305));
#44724=CARTESIAN_POINT('Ctrl Pts',(4.725327585499,11.91061577933,-8.869706635872));
#44725=CARTESIAN_POINT('Ctrl Pts',(4.720441050621,11.91824346637,-8.871985319865));
#44726=CARTESIAN_POINT('Ctrl Pts',(5.263405483213,10.56633525831,-7.765984057053));
#44727=CARTESIAN_POINT('Ctrl Pts',(5.24953910387,10.67241634538,-7.836077214095));
#44728=CARTESIAN_POINT('Ctrl Pts',(5.209789346079,10.88490733115,-7.975664007802));
#44729=CARTESIAN_POINT('Ctrl Pts',(5.11802262976,11.19199783826,-8.168244427088));
#44730=CARTESIAN_POINT('Ctrl Pts',(5.000199183344,11.47897625117,-8.333016823614));
#44731=CARTESIAN_POINT('Ctrl Pts',(4.868420870299,11.73341300754,-8.459550995621));
#44732=CARTESIAN_POINT('Ctrl Pts',(4.767730415513,11.89590862948,-8.523574335264));
#44733=CARTESIAN_POINT('Ctrl Pts',(4.715113959745,11.97405300316,-8.548439569164));
#44734=CARTESIAN_POINT('Ctrl Pts',(4.710562374606,11.98076613924,-8.550529537085));
#44735=CARTESIAN_POINT('Ctrl Pts',(5.429303416511,10.70239560335,-7.51838478119));
#44736=CARTESIAN_POINT('Ctrl Pts',(5.410831311191,10.81341375347,-7.588104635239));
#44737=CARTESIAN_POINT('Ctrl Pts',(5.361353134582,11.0336467798,-7.725975081631));
#44738=CARTESIAN_POINT('Ctrl Pts',(5.255448994482,11.34631646014,-7.913862147991));
#44739=CARTESIAN_POINT('Ctrl Pts',(5.12590846242,11.63265782121,-8.072310052117));
#44740=CARTESIAN_POINT('Ctrl Pts',(4.986818578048,11.88078489552,-8.191875405979));
#44741=CARTESIAN_POINT('Ctrl Pts',(4.884846125337,12.03511321985,-8.251040159787));
#44742=CARTESIAN_POINT('Ctrl Pts',(4.833039527478,12.10804408545,-8.273702750527));
#44743=CARTESIAN_POINT('Ctrl Pts',(4.828568893935,12.11429967682,-8.275604699134));
#44744=CARTESIAN_POINT('Ctrl Pts',(5.705336011203,10.79673328632,-7.369232710796));
#44745=CARTESIAN_POINT('Ctrl Pts',(5.683643415344,10.91707006838,-7.438886492236));
#44746=CARTESIAN_POINT('Ctrl Pts',(5.626721757645,11.15461489827,-7.575883270228));
#44747=CARTESIAN_POINT('Ctrl Pts',(5.508026128852,11.48875283381,-7.760751926392));
#44748=CARTESIAN_POINT('Ctrl Pts',(5.365574933928,11.79144130809,-7.914811324028));
#44749=CARTESIAN_POINT('Ctrl Pts',(5.215315821712,12.05040371183,-8.029331757309));
#44750=CARTESIAN_POINT('Ctrl Pts',(5.107305411296,12.20901075874,-8.084847190353));
#44751=CARTESIAN_POINT('Ctrl Pts',(5.053218350566,12.28317653379,-8.105803884447));
#44752=CARTESIAN_POINT('Ctrl Pts',(5.048556900723,12.28953202271,-8.10755978277));
#44753=CARTESIAN_POINT('',(5.0296756656025,12.2439817558929,-8.12864334680508));
#44754=CARTESIAN_POINT('Ctrl Pts',(5.02967626811991,12.2439818882291,-8.1286429048552));
#44755=CARTESIAN_POINT('Ctrl Pts',(5.02967648738242,12.2439809951838,-8.12864293636837));
#44756=CARTESIAN_POINT('Ctrl Pts',(5.02967670664473,12.2439801021382,-8.12864296788131));
#44757=CARTESIAN_POINT('Ctrl Pts',(5.02967692590687,12.2439792090923,-8.128642999394));
#44758=CARTESIAN_POINT('Ctrl Pts',(5.04084945619076,12.1984739392401,-8.13024873303066));
#44759=CARTESIAN_POINT('Ctrl Pts',(5.05153116834038,12.1521715925343,-8.13123707595096));
#44760=CARTESIAN_POINT('Ctrl Pts',(5.06169688000618,12.1054561046381,-8.13168208977979));
#44761=CARTESIAN_POINT('Ctrl Pts',(5.07037995894368,12.0655539037551,-8.13206219993155));
#44762=CARTESIAN_POINT('Ctrl Pts',(5.07868691827156,12.0253495868224,-8.13204747369092));
#44763=CARTESIAN_POINT('Ctrl Pts',(5.08661210601055,11.9850816455577,-8.1317058711365));
#44764=CARTESIAN_POINT('Ctrl Pts',(5.08661217722911,11.9850812836957,-8.13170586806674));
#44765=CARTESIAN_POINT('Ctrl Pts',(5.08661224844763,11.9850809218336,-8.13170586499695));
#44766=CARTESIAN_POINT('Ctrl Pts',(5.08661231966612,11.9850805599716,-8.13170586192714));
#44767=CARTESIAN_POINT('Ctrl Pts',(5.09521421993041,11.9413741985835,-8.13133508399009));
#44768=CARTESIAN_POINT('Ctrl Pts',(5.10337425549314,11.8975974876453,-8.13057930125357));
#44769=CARTESIAN_POINT('Ctrl Pts',(5.11120333789497,11.8532839497436,-8.12948489008677));
#44770=CARTESIAN_POINT('Ctrl Pts',(5.11903242029681,11.8089704118418,-8.12839047891998));
#44771=CARTESIAN_POINT('Ctrl Pts',(5.12653112604953,11.7641199980392,-8.12695640896504));
#44772=CARTESIAN_POINT('Ctrl Pts',(5.13378775745265,11.7182705694087,-8.12518126233682));
#44773=CARTESIAN_POINT('Ctrl Pts',(5.14486231968076,11.6482983850321,-8.12247215797336));
#44774=CARTESIAN_POINT('Ctrl Pts',(5.15535472479294,11.5759944016464,-8.11897642123504));
#44775=CARTESIAN_POINT('Ctrl Pts',(5.16519525578843,11.5013255754757,-8.11473197728622));
#44776=CARTESIAN_POINT('Ctrl Pts',(5.16825083759386,11.4781401694458,-8.11341403563144));
#44777=CARTESIAN_POINT('Ctrl Pts',(5.17124340411837,11.454726808459,-8.11202422654111));
#44778=CARTESIAN_POINT('Ctrl Pts',(5.17417040688738,11.43108476995,-8.11056461713076));
#44779=CARTESIAN_POINT('Ctrl Pts',(5.18231808703616,11.3652741838185,-8.10650161085566));
#44780=CARTESIAN_POINT('Ctrl Pts',(5.18995660706929,11.2976897736154,-8.1018934020723));
#44781=CARTESIAN_POINT('Ctrl Pts',(5.19698873514388,11.2287393237199,-8.09680289807924));
#44782=CARTESIAN_POINT('Ctrl Pts',(5.20061866017442,11.1931476847043,-8.09417522297627));
#44783=CARTESIAN_POINT('Ctrl Pts',(5.20408727345096,11.1571920463045,-8.09141990128149));
#44784=CARTESIAN_POINT('Ctrl Pts',(5.20738320932935,11.1209287096605,-8.08855055885703));
#44785=CARTESIAN_POINT('Ctrl Pts',(5.21389434195574,11.0492903638078,-8.08288216306126));
#44786=CARTESIAN_POINT('Ctrl Pts',(5.21973050537357,10.9764512949221,-8.07676267753496));
#44787=CARTESIAN_POINT('Ctrl Pts',(5.22481639026868,10.9030631605354,-8.07031469790219));
#44788=CARTESIAN_POINT('Ctrl Pts',(5.2272924227007,10.8673345892811,-8.06717553785022));
#44789=CARTESIAN_POINT('Ctrl Pts',(5.2295912026956,10.8314759452762,-8.0639591438049));
#44790=CARTESIAN_POINT('Ctrl Pts',(5.23170748242673,10.7955629743409,-8.06068231933708));
#44791=CARTESIAN_POINT('Ctrl Pts',(5.23678672400019,10.709368955508,-8.05281767704946));
#44792=CARTESIAN_POINT('Ctrl Pts',(5.24081943893851,10.6228631481432,-8.04460206063475));
#44793=CARTESIAN_POINT('Ctrl Pts',(5.24379785372006,10.5358259237703,-8.03611817822594));
#44794=CARTESIAN_POINT('Ctrl Pts',(5.24460940073787,10.5121103552351,-8.03380652253884));
#44795=CARTESIAN_POINT('Ctrl Pts',(5.24534248481075,10.4883555620476,-8.03147495313888));
#44796=CARTESIAN_POINT('Ctrl Pts',(5.24599653617109,10.4645576403199,-8.02912520903265));
#44797=CARTESIAN_POINT('Origin',(5.589034133447,12.40999918796,-8.940774072981));
#44798=CARTESIAN_POINT('Ctrl Pts',(4.987098562407,12.27585194406,-8.14835087597));
#44799=CARTESIAN_POINT('Ctrl Pts',(4.987098562407,12.26694242033,-8.150208671023));
#44800=CARTESIAN_POINT('Ctrl Pts',(4.987098562412,12.17370434769,-8.169454091409));
#44801=CARTESIAN_POINT('Ctrl Pts',(4.987098562457,11.99360631362,-8.202795817883));
#44802=CARTESIAN_POINT('Ctrl Pts',(4.987098562454,11.72908230884,-8.245409589304));
#44803=CARTESIAN_POINT('Ctrl Pts',(4.987098562392,11.44720983869,-8.286072928672));
#44804=CARTESIAN_POINT('Ctrl Pts',(4.987098562673,11.14595693493,-8.325928645102));
#44805=CARTESIAN_POINT('Ctrl Pts',(4.987098561544,10.8306092651,-8.365103658667));
#44806=CARTESIAN_POINT('Ctrl Pts',(4.987098564536,10.60836950429,-8.39178141968));
#44807=CARTESIAN_POINT('Ctrl Pts',(4.987098564583,10.49206836173,-8.405568226311));
#44808=CARTESIAN_POINT('Ctrl Pts',(4.987098564577,10.48360845566,-8.406570214801));
#44809=CARTESIAN_POINT('Ctrl Pts',(5.170465299867,12.25567265706,-8.051672134066));
#44810=CARTESIAN_POINT('Ctrl Pts',(5.170465299867,12.24689977024,-8.05350152513));
#44811=CARTESIAN_POINT('Ctrl Pts',(5.170465299868,12.15505390585,-8.072460052785));
#44812=CARTESIAN_POINT('Ctrl Pts',(5.170465299882,11.97691816161,-8.105445604263));
#44813=CARTESIAN_POINT('Ctrl Pts',(5.170465299881,11.71430579976,-8.147754747855));
#44814=CARTESIAN_POINT('Ctrl Pts',(5.170465299862,11.43376848665,-8.188227714547));
#44815=CARTESIAN_POINT('Ctrl Pts',(5.170465299947,11.13345274852,-8.227960364163));
#44816=CARTESIAN_POINT('Ctrl Pts',(5.170465299605,10.81868443806,-8.267063873485));
#44817=CARTESIAN_POINT('Ctrl Pts',(5.170465300511,10.59665069964,-8.293717021343));
#44818=CARTESIAN_POINT('Ctrl Pts',(5.170465300525,10.48044461194,-8.307492560892));
#44819=CARTESIAN_POINT('Ctrl Pts',(5.170465300523,10.47199157144,-8.308493735951));
#44820=CARTESIAN_POINT('Ctrl Pts',(5.268224992253,12.21809716683,-7.871648373944));
#44821=CARTESIAN_POINT('Ctrl Pts',(5.268224992253,12.20957870917,-7.873424874444));
#44822=CARTESIAN_POINT('Ctrl Pts',(5.268224992253,12.1203252509,-7.891849184266));
#44823=CARTESIAN_POINT('Ctrl Pts',(5.26822499225,11.94584345154,-7.92417150864));
#44824=CARTESIAN_POINT('Ctrl Pts',(5.26822499225,11.6867907259,-7.965913410188));
#44825=CARTESIAN_POINT('Ctrl Pts',(5.268224992254,11.40873958487,-8.006031887316));
#44826=CARTESIAN_POINT('Ctrl Pts',(5.268224992235,11.11016892614,-8.045535376416));
#44827=CARTESIAN_POINT('Ctrl Pts',(5.268224992313,10.79647943042,-8.08450573896));
#44828=CARTESIAN_POINT('Ctrl Pts',(5.268224992105,10.5748293226,-8.111113055102));
#44829=CARTESIAN_POINT('Ctrl Pts',(5.268224992102,10.45880023486,-8.12486761442));
#44830=CARTESIAN_POINT('Ctrl Pts',(5.268224992103,10.45035997864,-8.125867274802));
#44831=CARTESIAN_POINT('Ctrl Pts',(5.2475241072,12.17575325026,-7.668779135705));
#44832=CARTESIAN_POINT('Ctrl Pts',(5.2475241072,12.16752150946,-7.670496033694));
#44833=CARTESIAN_POINT('Ctrl Pts',(5.2475241072,12.08118944034,-7.688318332065));
#44834=CARTESIAN_POINT('Ctrl Pts',(5.2475241072,11.91082528085,-7.71989326411));
#44835=CARTESIAN_POINT('Ctrl Pts',(5.2475241072,11.65578391841,-7.76099593914));
#44836=CARTESIAN_POINT('Ctrl Pts',(5.2475241072,11.38053445109,-7.800714941067));
#44837=CARTESIAN_POINT('Ctrl Pts',(5.247524107202,11.08393032682,-7.839960188592));
#44838=CARTESIAN_POINT('Ctrl Pts',(5.247524107192,10.77145655021,-7.87878050769));
#44839=CARTESIAN_POINT('Ctrl Pts',(5.24752410722,10.55023875671,-7.905336175952));
#44840=CARTESIAN_POINT('Ctrl Pts',(5.24752410722,10.43440913067,-7.919067092593));
#44841=CARTESIAN_POINT('Ctrl Pts',(5.24752410722,10.42598328108,-7.920065046084));
#44842=CARTESIAN_POINT('Origin',(4.749999999929,12.16096907947,-7.722576335477));
#44843=CARTESIAN_POINT('Ctrl Pts',(4.898897183639,12.56298745161,-8.111309650193));
#44844=CARTESIAN_POINT('Ctrl Pts',(4.89889718364,12.554339838,-8.11368287565));
#44845=CARTESIAN_POINT('Ctrl Pts',(4.898897183641,12.52891246354,-8.12068549036));
#44846=CARTESIAN_POINT('Ctrl Pts',(4.89889718364,12.48660188763,-8.132388056127));
#44847=CARTESIAN_POINT('Ctrl Pts',(4.898897183642,12.43566213767,-8.146358919788));
#44848=CARTESIAN_POINT('Ctrl Pts',(4.898897183636,12.3827628083,-8.160506999916));
#44849=CARTESIAN_POINT('Ctrl Pts',(4.89889718366,12.32404545876,-8.175382572088));
#44850=CARTESIAN_POINT('Ctrl Pts',(4.898897183575,12.26901024473,-8.187959846287));
#44851=CARTESIAN_POINT('Ctrl Pts',(4.898897183596,12.23121289109,-8.195258127902));
#44852=CARTESIAN_POINT('Ctrl Pts',(4.898897183619,12.21791966919,-8.197644398133));
#44853=CARTESIAN_POINT('Ctrl Pts',(5.135442534893,12.54345730779,-8.040151306101));
#44854=CARTESIAN_POINT('Ctrl Pts',(5.135442534894,12.53476840202,-8.042535951411));
#44855=CARTESIAN_POINT('Ctrl Pts',(5.135442534894,12.50925370929,-8.04956268475));
#44856=CARTESIAN_POINT('Ctrl Pts',(5.135442534893,12.46696460986,-8.061259268755));
#44857=CARTESIAN_POINT('Ctrl Pts',(5.135442534894,12.41631345353,-8.075150729294));
#44858=CARTESIAN_POINT('Ctrl Pts',(5.135442534892,12.36408597898,-8.089117876537));
#44859=CARTESIAN_POINT('Ctrl Pts',(5.1354425349,12.30667505225,-8.103660339634));
#44860=CARTESIAN_POINT('Ctrl Pts',(5.135442534872,12.2535255264,-8.115798090918));
#44861=CARTESIAN_POINT('Ctrl Pts',(5.135442534879,12.21766329577,-8.122718057467));
#44862=CARTESIAN_POINT('Ctrl Pts',(5.135442534887,12.20513665072,-8.124962380836));
#44863=CARTESIAN_POINT('Ctrl Pts',(5.272152548789,12.48875957496,-7.840859374117));
#44864=CARTESIAN_POINT('Ctrl Pts',(5.272152548789,12.47995502296,-7.843276002811));
#44865=CARTESIAN_POINT('Ctrl Pts',(5.272152548789,12.45419577947,-7.850370284774));
#44866=CARTESIAN_POINT('Ctrl Pts',(5.272152548789,12.41196682884,-7.862050115762));
#44867=CARTESIAN_POINT('Ctrl Pts',(5.272152548789,12.36212393169,-7.875719193362));
#44868=CARTESIAN_POINT('Ctrl Pts',(5.272152548789,12.31177810915,-7.889179605035));
#44869=CARTESIAN_POINT('Ctrl Pts',(5.272152548788,12.25802605798,-7.902789135359));
#44870=CARTESIAN_POINT('Ctrl Pts',(5.272152548793,12.21015774612,-7.91369592249));
#44871=CARTESIAN_POINT('Ctrl Pts',(5.272152548792,12.17971518072,-7.919556348637));
#44872=CARTESIAN_POINT('Ctrl Pts',(5.27215254879,12.16933547408,-7.92140312391));
#44873=CARTESIAN_POINT('Ctrl Pts',(5.24752410724,12.42350167598,-7.603091333436));
#44874=CARTESIAN_POINT('Ctrl Pts',(5.24752410724,12.41455915062,-7.605546120356));
#44875=CARTESIAN_POINT('Ctrl Pts',(5.24752410724,12.38850814241,-7.612720992154));
#44876=CARTESIAN_POINT('Ctrl Pts',(5.24752410724,12.34635095316,-7.624380835719));
#44877=CARTESIAN_POINT('Ctrl Pts',(5.24752410724,12.29747236096,-7.637784596229));
#44878=CARTESIAN_POINT('Ctrl Pts',(5.24752410724,12.24937146982,-7.650640439906));
#44879=CARTESIAN_POINT('Ctrl Pts',(5.24752410724,12.19998469156,-7.663136921674));
#44880=CARTESIAN_POINT('Ctrl Pts',(5.24752410724,12.15841720627,-7.672575089719));
#44881=CARTESIAN_POINT('Ctrl Pts',(5.24752410724,12.13444064867,-7.677171416297));
#44882=CARTESIAN_POINT('Ctrl Pts',(5.24752410724,12.12662237706,-7.678543891224));
#44883=CARTESIAN_POINT('',(4.94560181045734,12.5323463870464,-8.10194138985371));
#44884=CARTESIAN_POINT('Ctrl Pts',(4.94560184643657,12.5323464095504,-8.10194147144728));
#44885=CARTESIAN_POINT('Ctrl Pts',(4.95021211447075,12.5147636855834,-8.10475801671934));
#44886=CARTESIAN_POINT('Ctrl Pts',(4.95491126399553,12.4971660349781,-8.10746710439704));
#44887=CARTESIAN_POINT('Ctrl Pts',(4.95963939106893,12.479691369481,-8.11001463335363));
#44888=CARTESIAN_POINT('Ctrl Pts',(4.96436751814233,12.4622167039839,-8.11256216231023));
#44889=CARTESIAN_POINT('Ctrl Pts',(4.96912560118877,12.4448656279846,-8.11495030211727));
#44890=CARTESIAN_POINT('Ctrl Pts',(4.97403921096105,12.4273482120725,-8.11714242005925));
#44891=CARTESIAN_POINT('Ctrl Pts',(4.97895282073333,12.4098307961603,-8.11933453800122));
#44892=CARTESIAN_POINT('Ctrl Pts',(4.98402319765244,12.3921474782198,-8.1213325009636));
#44893=CARTESIAN_POINT('Ctrl Pts',(4.98939982954737,12.373733426845,-8.12309825180934));
#44894=CARTESIAN_POINT('Ctrl Pts',(4.98939999823955,12.3737328491029,-8.12309830720989));
#44895=CARTESIAN_POINT('Ctrl Pts',(4.98940016693203,12.3737322713602,-8.1230983626102));
#44896=CARTESIAN_POINT('Ctrl Pts',(4.98940033562481,12.3737316936166,-8.12309841801029));
#44897=CARTESIAN_POINT('Ctrl Pts',(4.99267300103294,12.3625233823873,-8.12417318794445));
#44898=CARTESIAN_POINT('Ctrl Pts',(4.99606140290895,12.351040972025,-8.12516300805067));
#44899=CARTESIAN_POINT('Ctrl Pts',(4.99971722500461,12.3389118378633,-8.1260244993316));
#44900=CARTESIAN_POINT('Ctrl Pts',(5.00206681182121,12.331116476662,-8.12657817741093));
#44901=CARTESIAN_POINT('Ctrl Pts',(5.00452676102123,12.3230533869738,-8.12707838512241));
#44902=CARTESIAN_POINT('Ctrl Pts',(5.00713555182364,12.3146157102113,-8.12750524934951));
#44903=CARTESIAN_POINT('Ctrl Pts',(5.00713615243389,12.3146137676427,-8.12750534762456));
#44904=CARTESIAN_POINT('Ctrl Pts',(5.00713675305202,12.3146118250542,-8.12750544589568));
#44905=CARTESIAN_POINT('Ctrl Pts',(5.00713735367803,12.3146098824458,-8.12750554416287));
#44906=CARTESIAN_POINT('Ctrl Pts',(5.01088701655042,12.3024823248453,-8.12811901883954));
#44907=CARTESIAN_POINT('Ctrl Pts',(5.01493909774003,12.2895935841365,-8.12857880355176));
#44908=CARTESIAN_POINT('Ctrl Pts',(5.01923367534567,12.2761717227083,-8.12876405602454));
#44909=CARTESIAN_POINT('Ctrl Pts',(5.022576808797,12.2657234136918,-8.12890826665376));
#44910=CARTESIAN_POINT('Ctrl Pts',(5.02606683982151,12.2549517050472,-8.1288857258758));
#44911=CARTESIAN_POINT('Ctrl Pts',(5.02967477611916,12.2439868176467,-8.12864292461177));
#44912=CARTESIAN_POINT('Ctrl Pts',(5.02967514605934,12.2439856933606,-8.12864289971612));
#44913=CARTESIAN_POINT('Ctrl Pts',(5.02967551600076,12.2439845690726,-8.12864287481815));
#44914=CARTESIAN_POINT('Ctrl Pts',(5.02967588594343,12.2439834447825,-8.12864284991788));
#44915=CARTESIAN_POINT('Origin',(4.75,12.40999995988,-7.658352400433));
#44916=CARTESIAN_POINT('Ctrl Pts',(4.788362511431,11.83313520712,-9.106545692781));
#44917=CARTESIAN_POINT('Ctrl Pts',(4.781336029248,11.84312717048,-9.104679624838));
#44918=CARTESIAN_POINT('Ctrl Pts',(4.734941170835,11.90883089472,-9.091371892558));
#44919=CARTESIAN_POINT('Ctrl Pts',(4.6532235905,12.02218862506,-9.056946451773));
#44920=CARTESIAN_POINT('Ctrl Pts',(4.549498077196,12.16165915061,-9.003256917041));
#44921=CARTESIAN_POINT('Ctrl Pts',(4.447593846191,12.29168835275,-8.957496121759));
#44922=CARTESIAN_POINT('Ctrl Pts',(4.341839766253,12.414305274,-8.932669224563));
#44923=CARTESIAN_POINT('Ctrl Pts',(4.228724956104,12.52955087474,-8.936334256315));
#44924=CARTESIAN_POINT('Ctrl Pts',(4.107910016511,12.63834393914,-8.967414470431));
#44925=CARTESIAN_POINT('Ctrl Pts',(3.979407961331,12.74469289949,-9.016725402368));
#44926=CARTESIAN_POINT('Ctrl Pts',(3.841297009246,12.85384478495,-9.070431947384));
#44927=CARTESIAN_POINT('Ctrl Pts',(3.729267056962,12.9393797692,-9.102292739764));
#44928=CARTESIAN_POINT('Ctrl Pts',(3.664730289745,12.98734865969,-9.113614610693));
#44929=CARTESIAN_POINT('Ctrl Pts',(3.654902747863,12.99461778491,-9.115173463341));
#44930=CARTESIAN_POINT('Ctrl Pts',(4.680427221163,11.86641353654,-8.700123170612));
#44931=CARTESIAN_POINT('Ctrl Pts',(4.676272585031,11.87520161857,-8.697396084167));
#44932=CARTESIAN_POINT('Ctrl Pts',(4.648832174484,11.93327375709,-8.678686998039));
#44933=CARTESIAN_POINT('Ctrl Pts',(4.600262965426,12.03705267819,-8.638017975965));
#44934=CARTESIAN_POINT('Ctrl Pts',(4.533070467253,12.17352591546,-8.581549342235));
#44935=CARTESIAN_POINT('Ctrl Pts',(4.455773084827,12.30711579047,-8.535907121682));
#44936=CARTESIAN_POINT('Ctrl Pts',(4.361227371916,12.43386093394,-8.511743794177));
#44937=CARTESIAN_POINT('Ctrl Pts',(4.248215637988,12.54667493896,-8.515289415159));
#44938=CARTESIAN_POINT('Ctrl Pts',(4.122219669974,12.64113543641,-8.5456642095));
#44939=CARTESIAN_POINT('Ctrl Pts',(3.990318356226,12.71964485498,-8.595335621598));
#44940=CARTESIAN_POINT('Ctrl Pts',(3.856141420295,12.78951953089,-8.653002372258));
#44941=CARTESIAN_POINT('Ctrl Pts',(3.754500915548,12.84053766811,-8.692483554684));
#44942=CARTESIAN_POINT('Ctrl Pts',(3.697931827769,12.86909429444,-8.710053949906));
#44943=CARTESIAN_POINT('Ctrl Pts',(3.689358918034,12.87342214564,-8.712605773735));
#44944=CARTESIAN_POINT('Ctrl Pts',(4.784902130706,12.02281152679,-8.322549113858));
#44945=CARTESIAN_POINT('Ctrl Pts',(4.783249396625,12.0307502655,-8.320163567466));
#44946=CARTESIAN_POINT('Ctrl Pts',(4.772172682196,12.08365258323,-8.304031208104));
#44947=CARTESIAN_POINT('Ctrl Pts',(4.750277919023,12.18357420515,-8.271503273055));
#44948=CARTESIAN_POINT('Ctrl Pts',(4.708455753188,12.32563533914,-8.229059679281));
#44949=CARTESIAN_POINT('Ctrl Pts',(4.64410750416,12.47120052511,-8.195846114845));
#44950=CARTESIAN_POINT('Ctrl Pts',(4.550310030587,12.61049200715,-8.178540175844));
#44951=CARTESIAN_POINT('Ctrl Pts',(4.428613845404,12.73035393126,-8.181069390516));
#44952=CARTESIAN_POINT('Ctrl Pts',(4.289450200103,12.8216762436,-8.202883496443));
#44953=CARTESIAN_POINT('Ctrl Pts',(4.145901869533,12.88451933817,-8.239255237444));
#44954=CARTESIAN_POINT('Ctrl Pts',(4.007076074327,12.92646200883,-8.283117800936));
#44955=CARTESIAN_POINT('Ctrl Pts',(3.909998388249,12.94939041283,-8.315416010061));
#44956=CARTESIAN_POINT('Ctrl Pts',(3.858816430071,12.96108040816,-8.33110977569));
#44957=CARTESIAN_POINT('Ctrl Pts',(3.851123107886,12.96283050514,-8.333428536116));
#44958=CARTESIAN_POINT('Ctrl Pts',(5.065907741302,12.24861789423,-8.103492626421));
#44959=CARTESIAN_POINT('Ctrl Pts',(5.065527744701,12.25635351501,-8.10253388458));
#44960=CARTESIAN_POINT('Ctrl Pts',(5.062604240513,12.30832323267,-8.096071415204));
#44961=CARTESIAN_POINT('Ctrl Pts',(5.051749274438,12.41143376592,-8.083273366865));
#44962=CARTESIAN_POINT('Ctrl Pts',(5.015421902483,12.56574894735,-8.06684237541));
#44963=CARTESIAN_POINT('Ctrl Pts',(4.947917990377,12.72759143794,-8.054099213111));
#44964=CARTESIAN_POINT('Ctrl Pts',(4.844151662906,12.88353862421,-8.047489469458));
#44965=CARTESIAN_POINT('Ctrl Pts',(4.707965973537,13.0175075369,-8.048454343592));
#44966=CARTESIAN_POINT('Ctrl Pts',(4.55217013723,13.11796378328,-8.056792463515));
#44967=CARTESIAN_POINT('Ctrl Pts',(4.392726930966,13.18269400941,-8.070771847542));
#44968=CARTESIAN_POINT('Ctrl Pts',(4.242265944582,13.21764248226,-8.087806560847));
#44969=CARTESIAN_POINT('Ctrl Pts',(4.142357453441,13.22855503805,-8.100585259883));
#44970=CARTESIAN_POINT('Ctrl Pts',(4.092131989576,13.23171649105,-8.106921727197));
#44971=CARTESIAN_POINT('Ctrl Pts',(4.084641136283,13.23213762389,-8.107861429889));
#44972=CARTESIAN_POINT('',(4.07998030874528,13.1991631723816,-8.13213865329994));
#44973=CARTESIAN_POINT('Origin',(4.250000000204,13.7774991556,-8.930023854874));
#44974=CARTESIAN_POINT('',(4.37884053358692,13.1060646994139,-8.10486259615161));
#44975=CARTESIAN_POINT('Ctrl Pts',(4.07998006873709,13.199162565666,-8.13213914414405));
#44976=CARTESIAN_POINT('Ctrl Pts',(4.09485186734027,13.193838138298,-8.1328296702141));
#44977=CARTESIAN_POINT('Ctrl Pts',(4.10974150168657,13.1886223428026,-8.13304462029991));
#44978=CARTESIAN_POINT('Ctrl Pts',(4.12429557597898,13.1836267075159,-8.13289104638594));
#44979=CARTESIAN_POINT('Ctrl Pts',(4.12918128878347,13.1819497036202,-8.13283949257201));
#44980=CARTESIAN_POINT('Ctrl Pts',(4.13402937140421,13.180297908932,-8.13274643888225));
#44981=CARTESIAN_POINT('Ctrl Pts',(4.13882700960573,13.1786767289353,-8.13261589628058));
#44982=CARTESIAN_POINT('Ctrl Pts',(4.14982115159217,13.1749616753359,-8.13231674827529));
#44983=CARTESIAN_POINT('Ctrl Pts',(4.1605547904494,13.1714012335344,-8.13182659094922));
#44984=CARTESIAN_POINT('Ctrl Pts',(4.17127413559097,13.167913595797,-8.13117410839025));
#44985=CARTESIAN_POINT('Ctrl Pts',(4.17916746539731,13.1653454281951,-8.13069364433551));
#44986=CARTESIAN_POINT('Ctrl Pts',(4.18705381055708,13.1628158836012,-8.13012481013473));
#44987=CARTESIAN_POINT('Ctrl Pts',(4.19504044070577,13.1602770806608,-8.1294759888259));
#44988=CARTESIAN_POINT('Ctrl Pts',(4.19541353866471,13.1601584796767,-8.1294456789328));
#44989=CARTESIAN_POINT('Ctrl Pts',(4.1957868479523,13.1600398659674,-8.12941519061416));
#44990=CARTESIAN_POINT('Ctrl Pts',(4.19616036801421,13.1599212399424,-8.12938452432067));
#44991=CARTESIAN_POINT('Ctrl Pts',(4.2146408337908,13.1540520392814,-8.12786726341492));
#44992=CARTESIAN_POINT('Ctrl Pts',(4.23363533465402,13.1481515382724,-8.12591324528158));
#44993=CARTESIAN_POINT('Ctrl Pts',(4.25304057514006,13.1422859855327,-8.12357336709919));
#44994=CARTESIAN_POINT('Ctrl Pts',(4.26970170652261,13.1372498848516,-8.12156437278427));
#44995=CARTESIAN_POINT('Ctrl Pts',(4.28666681876166,13.1322389726019,-8.11927345682789));
#44996=CARTESIAN_POINT('Ctrl Pts',(4.30410507510598,13.1271836418196,-8.11672864605214));
#44997=CARTESIAN_POINT('Ctrl Pts',(4.30738768281662,13.1262320175586,-8.11624960644464));
#44998=CARTESIAN_POINT('Ctrl Pts',(4.31068710664069,13.1252786827765,-8.11576159716865));
#44999=CARTESIAN_POINT('Ctrl Pts',(4.31400453763256,13.1243229759357,-8.11526484703306));
#45000=CARTESIAN_POINT('Ctrl Pts',(4.32243271701589,13.1218949318522,-8.11400281648542));
#45001=CARTESIAN_POINT('Ctrl Pts',(4.3309757891944,13.1194539364639,-8.11268351689281));
#45002=CARTESIAN_POINT('Ctrl Pts',(4.33962681908085,13.1170044688423,-8.11131131639514));
#45003=CARTESIAN_POINT('Ctrl Pts',(4.35247016390373,13.113367981891,-8.10927414343549));
#45004=CARTESIAN_POINT('Ctrl Pts',(4.36555134351534,13.1097126394271,-8.10712032501676));
#45005=CARTESIAN_POINT('Ctrl Pts',(4.37884065455455,13.1060648835415,-8.10486301077009));
#45006=CARTESIAN_POINT('Ctrl Pts',(4.37884065455455,13.1060648835415,-8.10486301077009));
#45007=CARTESIAN_POINT('Ctrl Pts',(4.40088041631503,13.0999932368117,-8.10112911915094));
#45008=CARTESIAN_POINT('Ctrl Pts',(4.42265612898972,13.0929706812728,-8.09778340187562));
#45009=CARTESIAN_POINT('Ctrl Pts',(4.44398948902647,13.0850867284134,-8.09478417341399));
#45010=CARTESIAN_POINT('Ctrl Pts',(4.46147906082444,13.0786232852731,-8.09232533798311));
#45011=CARTESIAN_POINT('Ctrl Pts',(4.4786711993718,13.0715818552625,-8.09009958193691));
#45012=CARTESIAN_POINT('Ctrl Pts',(4.49547706814209,13.0640361851508,-8.08808524355259));
#45013=CARTESIAN_POINT('Ctrl Pts',(4.4979403304374,13.0629302045595,-8.08778999884612));
#45014=CARTESIAN_POINT('Ctrl Pts',(4.50039519708596,13.061813096606,-8.08749945327738));
#45015=CARTESIAN_POINT('Ctrl Pts',(4.50284193021159,13.0606847513753,-8.0872135239302));
#45016=CARTESIAN_POINT('Ctrl Pts',(4.52169287715546,13.0519913733136,-8.08501057057294));
#45017=CARTESIAN_POINT('Ctrl Pts',(4.5400613236599,13.0426349823631,-8.08308024202485));
#45018=CARTESIAN_POINT('Ctrl Pts',(4.55805604718657,13.0325834246664,-8.08138572021557));
#45019=CARTESIAN_POINT('Ctrl Pts',(4.57309759700418,13.0241814614123,-8.07996929199574));
#45020=CARTESIAN_POINT('Ctrl Pts',(4.587878377846,13.0152928662986,-8.0787179159458));
#45021=CARTESIAN_POINT('Ctrl Pts',(4.60245530568187,13.0058732724124,-8.0776191783943));
#45022=CARTESIAN_POINT('Ctrl Pts',(4.62156620056932,12.9935238342681,-8.07617869257368));
#45023=CARTESIAN_POINT('Ctrl Pts',(4.64033533417057,12.9802899205033,-8.07498840147022));
#45024=CARTESIAN_POINT('Ctrl Pts',(4.658580103847,12.9661945309864,-8.07407068066976));
#45025=CARTESIAN_POINT('Ctrl Pts',(4.67306102697751,12.9550069821323,-8.07334228318367));
#45026=CARTESIAN_POINT('Ctrl Pts',(4.68721151853636,12.9432770722533,-8.07278554246642));
#45027=CARTESIAN_POINT('Ctrl Pts',(4.70095515912211,12.9310535381473,-8.0724046213927));
#45028=CARTESIAN_POINT('Ctrl Pts',(4.71548774639111,12.9181283182958,-8.07200183373888));
#45029=CARTESIAN_POINT('Ctrl Pts',(4.72957256114547,12.9046467480563,-8.07179427222516));
#45030=CARTESIAN_POINT('Ctrl Pts',(4.74303440840472,12.8908181191709,-8.07177340722922));
#45031=CARTESIAN_POINT('Ctrl Pts',(4.75646072516754,12.8770259888462,-8.07175259730325));
#45032=CARTESIAN_POINT('Ctrl Pts',(4.76926682763735,12.8628893785513,-8.07191751001232));
#45033=CARTESIAN_POINT('Ctrl Pts',(4.78132056089648,12.8486445744751,-8.0722488014773));
#45034=CARTESIAN_POINT('Ctrl Pts',(4.78301098153662,12.8466468771388,-8.07229526193219));
#45035=CARTESIAN_POINT('Ctrl Pts',(4.7846866790031,12.844647087327,-8.07234497703885));
#45036=CARTESIAN_POINT('Ctrl Pts',(4.78634736250329,12.8426458887586,-8.07239787626646));
#45037=CARTESIAN_POINT('Ctrl Pts',(4.78831507021373,12.8402747121602,-8.07246055540914));
#45038=CARTESIAN_POINT('Ctrl Pts',(4.7902610940703,12.8379010652391,-8.07252802476904));
#45039=CARTESIAN_POINT('Ctrl Pts',(4.79218599750568,12.8355248500579,-8.07260019582179));
#45040=CARTESIAN_POINT('Ctrl Pts',(4.80452002164109,12.8202989977593,-8.07306263954241));
#45041=CARTESIAN_POINT('Ctrl Pts',(4.8159898093593,12.8049711843504,-8.07371690328845));
#45042=CARTESIAN_POINT('Ctrl Pts',(4.82675788022687,12.7895092955398,-8.07454053334698));
#45043=CARTESIAN_POINT('Ctrl Pts',(4.83598106412313,12.7762657122055,-8.07524599782486));
#45044=CARTESIAN_POINT('Ctrl Pts',(4.84468889125999,12.7629226466895,-8.07607603852168));
#45045=CARTESIAN_POINT('Ctrl Pts',(4.8529624584254,12.7494397032225,-8.0770243456723));
#45046=CARTESIAN_POINT('Ctrl Pts',(4.86112597842197,12.7361360971231,-8.07796003933771));
#45047=CARTESIAN_POINT('Ctrl Pts',(4.86885749410308,12.7226987514876,-8.07901338713688));
#45048=CARTESIAN_POINT('Ctrl Pts',(4.87624950212912,12.7089270234116,-8.08021320923806));
#45049=CARTESIAN_POINT('Ctrl Pts',(4.88127004455736,12.6995734695637,-8.08102811064835));
#45050=CARTESIAN_POINT('Ctrl Pts',(4.88613305397369,12.6900652213929,-8.08191086999274));
#45051=CARTESIAN_POINT('Ctrl Pts',(4.89085471528834,12.6803362971401,-8.08287436954563));
#45052=CARTESIAN_POINT('Ctrl Pts',(4.89573634274051,12.6702777646559,-8.0838705116986));
#45053=CARTESIAN_POINT('Ctrl Pts',(4.90046688079482,12.6599832461541,-8.08495295057575));
#45054=CARTESIAN_POINT('Ctrl Pts',(4.90505964902812,12.6493781808306,-8.08613810577501));
#45055=CARTESIAN_POINT('Ctrl Pts',(4.91245225821607,12.6323080611628,-8.08804575466347));
#45056=CARTESIAN_POINT('Ctrl Pts',(4.9195153698735,12.6144440009625,-8.09020459190755));
#45057=CARTESIAN_POINT('Ctrl Pts',(4.92605059631757,12.595935442534,-8.09265778829463));
#45058=CARTESIAN_POINT('Ctrl Pts',(4.93258977518952,12.5774156903477,-8.09511246834594));
#45059=CARTESIAN_POINT('Ctrl Pts',(4.9386000478383,12.558251267161,-8.09786168643568));
#45060=CARTESIAN_POINT('Ctrl Pts',(4.94392696676981,12.5386194520126,-8.10094653022285));
#45061=CARTESIAN_POINT('Ctrl Pts',(4.94449294521136,12.5365335963266,-8.10127429099817));
#45062=CARTESIAN_POINT('Ctrl Pts',(4.94505125356847,12.5344424843935,-8.10160584008563));
#45063=CARTESIAN_POINT('Ctrl Pts',(4.94560173849934,12.5323463420389,-8.10194122666757));
#45064=CARTESIAN_POINT('Ctrl Pts',(4.362160434186,13.06588598318,-8.125550161894));
#45065=CARTESIAN_POINT('Ctrl Pts',(4.369323430001,13.06383284013,-8.124118373749));
#45066=CARTESIAN_POINT('Ctrl Pts',(4.411515161595,13.05105630538,-8.115946316457));
#45067=CARTESIAN_POINT('Ctrl Pts',(4.487401204605,13.02082765928,-8.103918878687));
#45068=CARTESIAN_POINT('Ctrl Pts',(4.584800540606,12.96515873103,-8.093255079523));
#45069=CARTESIAN_POINT('Ctrl Pts',(4.673083800226,12.89664807489,-8.088013558801));
#45070=CARTESIAN_POINT('Ctrl Pts',(4.749096288908,12.81794410941,-8.088006774574));
#45071=CARTESIAN_POINT('Ctrl Pts',(4.811637239583,12.7322492577,-8.092781506338));
#45072=CARTESIAN_POINT('Ctrl Pts',(4.862806047777,12.63865887931,-8.102320087941));
#45073=CARTESIAN_POINT('Ctrl Pts',(4.890937846641,12.56489261123,-8.113320933997));
#45074=CARTESIAN_POINT('Ctrl Pts',(4.903190205307,12.52241499748,-8.121099998878));
#45075=CARTESIAN_POINT('Ctrl Pts',(4.905166983626,12.51516790621,-8.122470492991));
#45076=CARTESIAN_POINT('Ctrl Pts',(4.32819169137,13.30401108901,-8.053821312685));
#45077=CARTESIAN_POINT('Ctrl Pts',(4.339664949579,13.30254401372,-8.052284708458));
#45078=CARTESIAN_POINT('Ctrl Pts',(4.407297404261,13.29255218229,-8.043617185725));
#45079=CARTESIAN_POINT('Ctrl Pts',(4.529416968505,13.26023103414,-8.031694840149));
#45080=CARTESIAN_POINT('Ctrl Pts',(4.685790994072,13.18630244384,-8.021667416542));
#45081=CARTESIAN_POINT('Ctrl Pts',(4.825614762497,13.0860945265,-8.016876941016));
#45082=CARTESIAN_POINT('Ctrl Pts',(4.942633266184,12.96494921969,-8.016866232753));
#45083=CARTESIAN_POINT('Ctrl Pts',(5.034025620724,12.82959125095,-8.02124418716));
#45084=CARTESIAN_POINT('Ctrl Pts',(5.10212953111,12.68003156756,-8.030166647604));
#45085=CARTESIAN_POINT('Ctrl Pts',(5.132448218904,12.5616988631,-8.04102142987));
#45086=CARTESIAN_POINT('Ctrl Pts',(5.142003665006,12.49388627405,-8.049150073241));
#45087=CARTESIAN_POINT('Ctrl Pts',(5.143405454875,12.48232839475,-8.050596112836));
#45088=CARTESIAN_POINT('Ctrl Pts',(4.258497095234,13.43734788581,-7.852905774059));
#45089=CARTESIAN_POINT('Ctrl Pts',(4.273532865299,13.43711178824,-7.850948149822));
#45090=CARTESIAN_POINT('Ctrl Pts',(4.362214226134,13.43371377916,-7.839982893492));
#45091=CARTESIAN_POINT('Ctrl Pts',(4.522777339243,13.40629043844,-7.825554672333));
#45092=CARTESIAN_POINT('Ctrl Pts',(4.728216508237,13.32352445065,-7.813942645311));
#45093=CARTESIAN_POINT('Ctrl Pts',(4.91025077699,13.20090894489,-7.808542095672));
#45094=CARTESIAN_POINT('Ctrl Pts',(5.059442211679,13.04647229783,-7.808526441464));
#45095=CARTESIAN_POINT('Ctrl Pts',(5.17118679781,12.87059606495,-7.813472689643));
#45096=CARTESIAN_POINT('Ctrl Pts',(5.247606559789,12.67474389681,-7.823762479838));
#45097=CARTESIAN_POINT('Ctrl Pts',(5.273659508659,12.51948199623,-7.836833373193));
#45098=CARTESIAN_POINT('Ctrl Pts',(5.276855433658,12.43082409665,-7.847020998172));
#45099=CARTESIAN_POINT('Ctrl Pts',(5.277058326871,12.4157247669,-7.84884462381));
#45100=CARTESIAN_POINT('Ctrl Pts',(4.185096455794,13.40463740749,-7.615110234522));
#45101=CARTESIAN_POINT('Ctrl Pts',(4.201310261247,13.40571164913,-7.612608815703));
#45102=CARTESIAN_POINT('Ctrl Pts',(4.296978205788,13.40968717958,-7.598599206084));
#45103=CARTESIAN_POINT('Ctrl Pts',(4.470532763759,13.39190175455,-7.580205416763));
#45104=CARTESIAN_POINT('Ctrl Pts',(4.692585515909,13.31378080213,-7.565515822195));
#45105=CARTESIAN_POINT('Ctrl Pts',(4.8881074932,13.18834210605,-7.558724365674));
#45106=CARTESIAN_POINT('Ctrl Pts',(5.045857555171,13.02505917063,-7.558705015931));
#45107=CARTESIAN_POINT('Ctrl Pts',(5.160104768517,12.83642484523,-7.564923537623));
#45108=CARTESIAN_POINT('Ctrl Pts',(5.232400577203,12.6252251833,-7.577935915749));
#45109=CARTESIAN_POINT('Ctrl Pts',(5.249694969059,12.45763771892,-7.594566946463));
#45110=CARTESIAN_POINT('Ctrl Pts',(5.245790521177,12.36220114111,-7.607576997605));
#45111=CARTESIAN_POINT('Ctrl Pts',(5.244721418994,12.34595674815,-7.609906775374));
#45112=CARTESIAN_POINT('',(4.25000024490979,13.4099999999935,-7.66332090715394));
#45113=CARTESIAN_POINT('Origin',(4.250000381636,12.90999999997,-7.66332088393));
#45114=CARTESIAN_POINT('Ctrl Pts',(4.25000025238628,13.41,-7.6633209585883));
#45115=CARTESIAN_POINT('Ctrl Pts',(4.28415493337604,13.4099999913798,-7.65835623525745));
#45116=CARTESIAN_POINT('Ctrl Pts',(4.31814697540359,13.4082459767664,-7.65381476712852));
#45117=CARTESIAN_POINT('Ctrl Pts',(4.35172158509816,13.4048129065936,-7.64966299552958));
#45118=CARTESIAN_POINT('Ctrl Pts',(4.38544423063766,13.4013646994631,-7.64549291810304));
#45119=CARTESIAN_POINT('Ctrl Pts',(4.41874511751802,13.3962228787199,-7.6417159812516));
#45120=CARTESIAN_POINT('Ctrl Pts',(4.45138625796055,13.389511906566,-7.63829818044653));
#45121=CARTESIAN_POINT('Ctrl Pts',(4.46161634966191,13.3874086142298,-7.6372270041586));
#45122=CARTESIAN_POINT('Ctrl Pts',(4.47178182289008,13.3851515282507,-7.63619110452606));
#45123=CARTESIAN_POINT('Ctrl Pts',(4.4818759025286,13.3827453756387,-7.63518943471117));
#45124=CARTESIAN_POINT('Ctrl Pts',(4.51075697499333,13.3758609175766,-7.63232346777357));
#45125=CARTESIAN_POINT('Ctrl Pts',(4.53904771285317,13.3677623319655,-7.62973771995563));
#45126=CARTESIAN_POINT('Ctrl Pts',(4.56681852051631,13.3584861754701,-7.6274026746863));
#45127=CARTESIAN_POINT('Ctrl Pts',(4.59478006125459,13.3491463092736,-7.62505159205967));
#45128=CARTESIAN_POINT('Ctrl Pts',(4.62221532564241,13.3386123996553,-7.62295466751495));
#45129=CARTESIAN_POINT('Ctrl Pts',(4.6491849939952,13.3268704055476,-7.621081772125));
#45130=CARTESIAN_POINT('Ctrl Pts',(4.66440127267806,13.3202455760429,-7.62002508511557));
#45131=CARTESIAN_POINT('Ctrl Pts',(4.67946907126468,13.3132352797687,-7.61903971135721));
#45132=CARTESIAN_POINT('Ctrl Pts',(4.69439624426327,13.3058303288484,-7.61812023979166));
#45133=CARTESIAN_POINT('Ctrl Pts',(4.72551027391046,13.2903955333589,-7.61620370371663));
#45134=CARTESIAN_POINT('Ctrl Pts',(4.75599854582717,13.2732465032488,-7.61457349131395));
#45135=CARTESIAN_POINT('Ctrl Pts',(4.78560383747331,13.2544693773512,-7.61323779027849));
#45136=CARTESIAN_POINT('Ctrl Pts',(4.8151597086785,13.2357235963176,-7.61190431894354));
#45137=CARTESIAN_POINT('Ctrl Pts',(4.84383490385939,13.2153554159023,-7.61086437653432));
#45138=CARTESIAN_POINT('Ctrl Pts',(4.87139399083305,13.1934982502575,-7.61012610981066));
#45139=CARTESIAN_POINT('Ctrl Pts',(4.87626049766555,13.1896386141944,-7.60999574337079));
#45140=CARTESIAN_POINT('Ctrl Pts',(4.88109226752965,13.1857326622559,-7.60987478380504));
#45141=CARTESIAN_POINT('Ctrl Pts',(4.88588809340355,13.1817812725556,-7.60976327597167));
#45142=CARTESIAN_POINT('Ctrl Pts',(4.90576650621335,13.1654029974264,-7.60930108263906));
#45143=CARTESIAN_POINT('Ctrl Pts',(4.92503580965707,13.1482315816514,-7.60900127509333));
#45144=CARTESIAN_POINT('Ctrl Pts',(4.9435328183971,13.1304250341334,-7.60885617900091));
#45145=CARTESIAN_POINT('Ctrl Pts',(4.96217990656388,13.1124740093932,-7.60870990564038));
#45146=CARTESIAN_POINT('Ctrl Pts',(4.98004168199111,13.0938779739926,-7.60872086448693));
#45147=CARTESIAN_POINT('Ctrl Pts',(4.99699092323015,13.074834235439,-7.60888119288522));
#45148=CARTESIAN_POINT('Ctrl Pts',(5.01326443784369,13.0565497262225,-7.60903512936508));
#45149=CARTESIAN_POINT('Ctrl Pts',(5.02869681276836,13.0378531896953,-7.6093267627795));
#45150=CARTESIAN_POINT('Ctrl Pts',(5.04321411733002,13.0189428249584,-7.609749133877));
#45151=CARTESIAN_POINT('Ctrl Pts',(5.06060603931925,12.9962879590434,-7.61025514001244));
#45152=CARTESIAN_POINT('Ctrl Pts',(5.07669654126715,12.9733258348404,-7.61094878551759));
#45153=CARTESIAN_POINT('Ctrl Pts',(5.09161639757621,12.9500757718421,-7.61181896630913));
#45154=CARTESIAN_POINT('Ctrl Pts',(5.10693797017169,12.9261997022139,-7.61271257666923));
#45155=CARTESIAN_POINT('Ctrl Pts',(5.12102551994337,12.902019406217,-7.61379235670061));
#45156=CARTESIAN_POINT('Ctrl Pts',(5.13398627545505,12.8775128498845,-7.61504628102299));
#45157=CARTESIAN_POINT('Ctrl Pts',(5.14079582648039,12.8646371617619,-7.61570508996722));
#45158=CARTESIAN_POINT('Ctrl Pts',(5.14729371912646,12.8516707591378,-7.61641197017769));
#45159=CARTESIAN_POINT('Ctrl Pts',(5.15349116847712,12.8386067060649,-7.61716517758683));
#45160=CARTESIAN_POINT('Ctrl Pts',(5.16284753929381,12.8188837332737,-7.61830230472141));
#45161=CARTESIAN_POINT('Ctrl Pts',(5.1715142138442,12.7989569858579,-7.61954502237368));
#45162=CARTESIAN_POINT('Ctrl Pts',(5.17955764954905,12.7786767909224,-7.62092269173428));
#45163=CARTESIAN_POINT('Ctrl Pts',(5.18754921097392,12.758527388418,-7.62229147613468));
#45164=CARTESIAN_POINT('Ctrl Pts',(5.19492576677389,12.7380285473847,-7.62379347717676));
#45165=CARTESIAN_POINT('Ctrl Pts',(5.20170404880516,12.7170169433238,-7.62545749163233));
#45166=CARTESIAN_POINT('Ctrl Pts',(5.20833992004127,12.6964467902424,-7.62708654536765));
#45167=CARTESIAN_POINT('Ctrl Pts',(5.21440256391927,12.6753846636706,-7.6288708762714));
#45168=CARTESIAN_POINT('Ctrl Pts',(5.21985838876017,12.6536692548344,-7.63083750393334));
#45169=CARTESIAN_POINT('Ctrl Pts',(5.22089342463171,12.6495495794844,-7.6312105969551));
#45170=CARTESIAN_POINT('Ctrl Pts',(5.22190647058077,12.6454063817389,-7.63159025095984));
#45171=CARTESIAN_POINT('Ctrl Pts',(5.22289708207348,12.641238551485,-7.63197665043367));
#45172=CARTESIAN_POINT('Ctrl Pts',(5.22930372598955,12.6142836811497,-7.63447563601622));
#45173=CARTESIAN_POINT('Ctrl Pts',(5.23476590910481,12.5863081834297,-7.63725676286129));
#45174=CARTESIAN_POINT('Ctrl Pts',(5.23906231640469,12.5574982517462,-7.64035714954161));
#45175=CARTESIAN_POINT('Ctrl Pts',(5.24327909769855,12.5292222591504,-7.643400076258));
#45176=CARTESIAN_POINT('Ctrl Pts',(5.24637240858335,12.5001429148305,-7.64675053868086));
#45177=CARTESIAN_POINT('Ctrl Pts',(5.24817002368789,12.4704698586976,-7.65044362962145));
#45178=CARTESIAN_POINT('Ctrl Pts',(5.24937639154043,12.4505564629351,-7.65292203902956));
#45179=CARTESIAN_POINT('Ctrl Pts',(5.25000000001406,12.4303763800539,-7.65555475684944));
#45180=CARTESIAN_POINT('Ctrl Pts',(5.25,12.40999999931,-7.658352389464));
#45181=CARTESIAN_POINT('Origin',(4.25,12.41,8.));
#45182=CARTESIAN_POINT('',(4.25,13.41,7.5));
#45183=CARTESIAN_POINT('Origin',(4.25,12.41,7.5));
#45184=CARTESIAN_POINT('',(4.249999999336,13.41,7.5));
#45185=CARTESIAN_POINT('Ctrl Pts',(4.24999999999483,12.91,7.99999999999811));
#45186=CARTESIAN_POINT('Ctrl Pts',(4.75000000031615,12.9099999999981,8.00000000000139));
#45187=CARTESIAN_POINT('Ctrl Pts',(4.74999999999708,12.4099999996768,7.9999999999991));
#45188=CARTESIAN_POINT('Ctrl Pts',(4.24999999999672,13.4100000000044,8.00000000000096));
#45189=CARTESIAN_POINT('Ctrl Pts',(5.25000000063966,13.4100000000007,8.00000000000752));
#45190=CARTESIAN_POINT('Ctrl Pts',(5.25000000000152,12.4099999993577,8.00000000000294));
#45191=CARTESIAN_POINT('Ctrl Pts',(4.25,13.4100000000016,7.49999999999652));
#45192=CARTESIAN_POINT('Ctrl Pts',(5.25000000063778,13.4099999999978,7.50000000000308));
#45193=CARTESIAN_POINT('Ctrl Pts',(5.24999999999965,12.40999999936,7.4999999999985));
#45194=CARTESIAN_POINT('',(4.75,12.41,8.));
#45195=CARTESIAN_POINT('',(4.25,12.91,8.));
#45196=CARTESIAN_POINT('Origin',(4.25,12.41,8.));
#45197=CARTESIAN_POINT('Origin',(4.75,12.41,7.5));
#45198=CARTESIAN_POINT('Origin',(4.25,12.91,7.5));
#45199=CARTESIAN_POINT('Origin',(-4.6,13.41,8.));
#45200=CARTESIAN_POINT('',(4.75,1.410000000002,8.));
#45201=CARTESIAN_POINT('',(-1.6,12.91,8.));
#45202=CARTESIAN_POINT('',(4.25,12.91,8.));
#45203=CARTESIAN_POINT('',(-4.1,10.41,8.));
#45204=CARTESIAN_POINT('Origin',(-1.6,10.41,8.));
#45205=CARTESIAN_POINT('',(-4.1,10.41,8.));
#45206=CARTESIAN_POINT('',(-4.40872847693047E-16,12.51,8.));
#45207=CARTESIAN_POINT('Origin',(0.,8.91,8.));
#45208=CARTESIAN_POINT('Origin',(0.,8.91,8.));
#45209=CARTESIAN_POINT('',(-4.40872847693047E-16,12.51,7.));
#45210=CARTESIAN_POINT('Origin',(0.,8.91,7.));
#45211=CARTESIAN_POINT('',(-4.40872847693047E-16,12.51,8.));
#45212=CARTESIAN_POINT('Origin',(-4.6,0.,7.));
#45213=CARTESIAN_POINT('',(0.,5.68,7.));
#45214=CARTESIAN_POINT('Origin',(0.,8.91,7.));
#45215=CARTESIAN_POINT('Origin',(0.,8.91,8.));
#45216=CARTESIAN_POINT('',(0.,5.68,-16.1));
#45217=CARTESIAN_POINT('Origin',(0.,8.91,-16.1));
#45218=CARTESIAN_POINT('',(3.95560916124595E-16,5.68,8.));
#45219=CARTESIAN_POINT('',(3.95560916124595E-16,5.68,8.));
#45220=CARTESIAN_POINT('Origin',(-4.6,0.,-16.1));
#45221=CARTESIAN_POINT('',(1.258051184494,4.68,-16.1));
#45222=CARTESIAN_POINT('',(4.23,7.656716133874,-16.1));
#45223=CARTESIAN_POINT('Origin',(1.2063075471551,7.70854277345064,-16.1));
#45224=CARTESIAN_POINT('',(-1.245641523513,4.68,-16.1));
#45225=CARTESIAN_POINT('',(1.258051184494,4.68,-16.1));
#45226=CARTESIAN_POINT('',(-4.23,7.689614180046,-16.1));
#45227=CARTESIAN_POINT('Origin',(-1.22687177271412,7.70854277344467,-16.1));
#45228=CARTESIAN_POINT('',(-4.23,10.14289693909,-16.1));
#45229=CARTESIAN_POINT('',(-4.23,10.14289693909,-16.1));
#45230=CARTESIAN_POINT('',(-1.231437138339,13.14,-16.1));
#45231=CARTESIAN_POINT('Origin',(-1.22687177271438,10.1383337960394,-16.1));
#45232=CARTESIAN_POINT('',(1.218893149689,13.14,-16.1));
#45233=CARTESIAN_POINT('',(4.23,10.15082771808,-16.1));
#45234=CARTESIAN_POINT('Origin',(-2.749877045436,12.05258860061,-47.51676));
#45235=CARTESIAN_POINT('',(1.258051184494,4.68,-16.1));
#45236=CARTESIAN_POINT('',(4.23,7.656716133874,-16.1));
#45237=CARTESIAN_POINT('Origin',(4.23,0.,-16.1));
#45238=CARTESIAN_POINT('Origin',(-4.6,3.56,-8.));
#45239=CARTESIAN_POINT('',(-1.576219094763,3.679332757285,-8.863031548225));
#45240=CARTESIAN_POINT('',(-1.576219094763,3.679332757285,-8.863031548225));
#45241=CARTESIAN_POINT('',(-1.576219094763,3.679332757285,-8.863031548225));
#45242=CARTESIAN_POINT('Origin',(-1.673987770644,2.688757347123,-9.));
#45243=CARTESIAN_POINT('Origin',(-1.576219094767,2.688757347123,-9.));
#45244=CARTESIAN_POINT('Ctrl Pts',(-4.555013514898,6.748954102442,-9.006265058719));
#45245=CARTESIAN_POINT('Ctrl Pts',(-4.556447823076,6.654112126016,-9.001984393795));
#45246=CARTESIAN_POINT('Ctrl Pts',(-4.549028255214,6.413451891621,-8.991281013082));
#45247=CARTESIAN_POINT('Ctrl Pts',(-4.494420707384,6.046862385281,-8.975598452435));
#45248=CARTESIAN_POINT('Ctrl Pts',(-4.385548769305,5.671570029758,-8.960309855565));
#45249=CARTESIAN_POINT('Ctrl Pts',(-4.249041101692,5.351127072694,-8.947889723381));
#45250=CARTESIAN_POINT('Ctrl Pts',(-4.095807849191,5.077797340177,-8.937834704605));
#45251=CARTESIAN_POINT('Ctrl Pts',(-3.93137473704,4.842250471115,-8.929646446674));
#45252=CARTESIAN_POINT('Ctrl Pts',(-3.75682360245,4.635573614044,-8.922909486779));
#45253=CARTESIAN_POINT('Ctrl Pts',(-3.571393820409,4.451722491939,-8.917364128898));
#45254=CARTESIAN_POINT('Ctrl Pts',(-3.374685391696,4.287862755454,-8.912889712537));
#45255=CARTESIAN_POINT('Ctrl Pts',(-3.166908514,4.14295750472,-8.909437356023));
#45256=CARTESIAN_POINT('Ctrl Pts',(-2.947784283048,4.016392071403,-8.906984289856));
#45257=CARTESIAN_POINT('Ctrl Pts',(-2.716575401331,3.908084602248,-8.905538460177));
#45258=CARTESIAN_POINT('Ctrl Pts',(-2.470263032896,3.817877379428,-8.905138263878));
#45259=CARTESIAN_POINT('Ctrl Pts',(-2.202177792142,3.746305952892,-8.905907855567));
#45260=CARTESIAN_POINT('Ctrl Pts',(-1.902141250127,3.696680270292,-8.908149149792));
#45261=CARTESIAN_POINT('Ctrl Pts',(-1.673459288454,3.683895992251,-8.91099064003));
#45262=CARTESIAN_POINT('Ctrl Pts',(-1.544864774431,3.685086791525,-8.912967262473));
#45263=CARTESIAN_POINT('Ctrl Pts',(-1.529192023974,3.685356654255,-8.913213783927));
#45264=CARTESIAN_POINT('Ctrl Pts',(-4.551445835519,6.748899079632,-8.43676403776));
#45265=CARTESIAN_POINT('Ctrl Pts',(-4.555316030739,6.654204804538,-8.432468577285));
#45266=CARTESIAN_POINT('Ctrl Pts',(-4.554009041628,6.413344898856,-8.421763232492));
#45267=CARTESIAN_POINT('Ctrl Pts',(-4.50813646724,6.044315347024,-8.406227812707));
#45268=CARTESIAN_POINT('Ctrl Pts',(-4.406998304746,5.664250402887,-8.39122687889));
#45269=CARTESIAN_POINT('Ctrl Pts',(-4.275820969953,5.338196002922,-8.379138040623));
#45270=CARTESIAN_POINT('Ctrl Pts',(-4.125918859847,5.059063976121,-8.369414768897));
#45271=CARTESIAN_POINT('Ctrl Pts',(-3.963230034915,4.81785346704,-8.361538711491));
#45272=CARTESIAN_POINT('Ctrl Pts',(-3.789148076767,4.605778526808,-8.355086998769));
#45273=CARTESIAN_POINT('Ctrl Pts',(-3.603102197143,4.416865877513,-8.349795833183));
#45274=CARTESIAN_POINT('Ctrl Pts',(-3.404816945335,4.248374826253,-8.34553936651));
#45275=CARTESIAN_POINT('Ctrl Pts',(-3.194612641259,4.099379337421,-8.342263036106));
#45276=CARTESIAN_POINT('Ctrl Pts',(-2.972311875782,3.969365921545,-8.339939216805));
#45277=CARTESIAN_POINT('Ctrl Pts',(-2.7372726709,3.858355006536,-8.338571196862));
#45278=CARTESIAN_POINT('Ctrl Pts',(-2.486539606334,3.766286063129,-8.338192764716));
#45279=CARTESIAN_POINT('Ctrl Pts',(-2.213451223554,3.693832607777,-8.338920550267));
#45280=CARTESIAN_POINT('Ctrl Pts',(-1.907815402646,3.644575726475,-8.341042072484));
#45281=CARTESIAN_POINT('Ctrl Pts',(-1.675073037896,3.633188818873,-8.343736117257));
#45282=CARTESIAN_POINT('Ctrl Pts',(-1.544341556226,3.635522541957,-8.34561460226));
#45283=CARTESIAN_POINT('Ctrl Pts',(-1.528410670948,3.635936933942,-8.345849180363));
#45284=CARTESIAN_POINT('Ctrl Pts',(-4.944357460806,6.754958137238,-8.02454051063));
#45285=CARTESIAN_POINT('Ctrl Pts',(-4.950178879718,6.648164231245,-8.021927553065));
#45286=CARTESIAN_POINT('Ctrl Pts',(-4.952314090325,6.376150039691,-8.015454344926));
#45287=CARTESIAN_POINT('Ctrl Pts',(-4.905540054373,5.957982614761,-8.006227774445));
#45288=CARTESIAN_POINT('Ctrl Pts',(-4.79557736435,5.525814961368,-7.997480967033));
#45289=CARTESIAN_POINT('Ctrl Pts',(-4.650154913714,5.154049620586,-7.990543071787));
#45290=CARTESIAN_POINT('Ctrl Pts',(-4.482325211086,4.835109890624,-7.985035586605));
#45291=CARTESIAN_POINT('Ctrl Pts',(-4.29905970525,4.559051487263,-7.980622885206));
#45292=CARTESIAN_POINT('Ctrl Pts',(-4.102123502363,4.316038923001,-7.977041098496));
#45293=CARTESIAN_POINT('Ctrl Pts',(-3.890984442267,4.099374026924,-7.974126196536));
#45294=CARTESIAN_POINT('Ctrl Pts',(-3.665406689107,3.90602233631,-7.97179632394));
#45295=CARTESIAN_POINT('Ctrl Pts',(-3.425821445495,3.735009363527,-7.970012165066));
#45296=CARTESIAN_POINT('Ctrl Pts',(-3.172091618693,3.585819602461,-7.968751607297));
#45297=CARTESIAN_POINT('Ctrl Pts',(-2.9035510228,3.458540431353,-7.968011444657));
#45298=CARTESIAN_POINT('Ctrl Pts',(-2.616895030684,3.353162131553,-7.967806962617));
#45299=CARTESIAN_POINT('Ctrl Pts',(-2.304590451932,3.270525568452,-7.968200269829));
#45300=CARTESIAN_POINT('Ctrl Pts',(-1.955097738855,3.214834608574,-7.96934911048));
#45301=CARTESIAN_POINT('Ctrl Pts',(-1.689114387761,3.202622899529,-7.97081316528));
#45302=CARTESIAN_POINT('Ctrl Pts',(-1.539811653485,3.205845373877,-7.971839221048));
#45303=CARTESIAN_POINT('Ctrl Pts',(-1.521619260623,3.206388153424,-7.971967698541));
#45304=CARTESIAN_POINT('Ctrl Pts',(-5.513310479943,6.763731920509,-8.00086707723));
#45305=CARTESIAN_POINT('Ctrl Pts',(-5.519503750751,6.639379390508,-8.000689974857));
#45306=CARTESIAN_POINT('Ctrl Pts',(-5.520479581067,6.322735001717,-8.000308619381));
#45307=CARTESIAN_POINT('Ctrl Pts',(-5.463673401723,5.836300034902,-8.00001310954));
#45308=CARTESIAN_POINT('Ctrl Pts',(-5.333278766416,5.333931092847,-7.999978096344));
#45309=CARTESIAN_POINT('Ctrl Pts',(-5.162027786566,4.902000836767,-8.000120924242));
#45310=CARTESIAN_POINT('Ctrl Pts',(-4.965069797,4.531581584195,-8.000348053384));
#45311=CARTESIAN_POINT('Ctrl Pts',(-4.750450918913,4.211041986036,-8.000606793039));
#45312=CARTESIAN_POINT('Ctrl Pts',(-4.520159124177,3.928909404814,-8.000869476857));
#45313=CARTESIAN_POINT('Ctrl Pts',(-4.273528000303,3.6773715762,-8.001119738332));
#45314=CARTESIAN_POINT('Ctrl Pts',(-4.010254167232,3.452877657092,-8.001344213877));
#45315=CARTESIAN_POINT('Ctrl Pts',(-3.730818261462,3.25427257492,-8.001531208702));
#45316=CARTESIAN_POINT('Ctrl Pts',(-3.435039708917,3.080936742835,-8.001671398203));
#45317=CARTESIAN_POINT('Ctrl Pts',(-3.122122169926,2.932951596962,-8.001756889332));
#45318=CARTESIAN_POINT('Ctrl Pts',(-2.788195105891,2.810283344696,-8.001780950925));
#45319=CARTESIAN_POINT('Ctrl Pts',(-2.424463009301,2.713875693873,-8.001734762281));
#45320=CARTESIAN_POINT('Ctrl Pts',(-2.017461124553,2.648557530889,-8.001603722034));
#45321=CARTESIAN_POINT('Ctrl Pts',(-1.707705622985,2.633761592545,-8.001445312088));
#45322=CARTESIAN_POINT('Ctrl Pts',(-1.533816508689,2.637120023378,-8.001342891059));
#45323=CARTESIAN_POINT('Ctrl Pts',(-1.512628024633,2.637703018638,-8.001330637038));
#45324=CARTESIAN_POINT('',(-4.56872735814743,6.21817739199662,-8.68455045311303));
#45325=CARTESIAN_POINT('Ctrl Pts',(-4.09999994889581,3.59647863419517,-7.9999999943637));
#45326=CARTESIAN_POINT('Ctrl Pts',(-4.10784885595024,3.63493711424939,-7.99999999507475));
#45327=CARTESIAN_POINT('Ctrl Pts',(-4.11563766356533,3.67273218799167,-8.00090976440895));
#45328=CARTESIAN_POINT('Ctrl Pts',(-4.12336776546972,3.7098404370961,-8.0025577781243));
#45329=CARTESIAN_POINT('Ctrl Pts',(-4.13082795095019,3.74565295607691,-8.00414824719481));
#45330=CARTESIAN_POINT('Ctrl Pts',(-4.13823314028214,3.78082671080731,-8.00642597730379));
#45331=CARTESIAN_POINT('Ctrl Pts',(-4.14556120029949,3.81537188993273,-8.00926132268278));
#45332=CARTESIAN_POINT('Ctrl Pts',(-4.14961303631167,3.83447263426291,-8.01082904381039));
#45333=CARTESIAN_POINT('Ctrl Pts',(-4.1536408997682,3.85338168668975,-8.01256771249665));
#45334=CARTESIAN_POINT('Ctrl Pts',(-4.15763848499059,3.87210352808029,-8.01445918360056));
#45335=CARTESIAN_POINT('Ctrl Pts',(-4.16604335298257,3.91146594231295,-8.01843597560237));
#45336=CARTESIAN_POINT('Ctrl Pts',(-4.1743216333607,3.94998873082823,-8.02308440620833));
#45337=CARTESIAN_POINT('Ctrl Pts',(-4.18247881285424,3.98770631964574,-8.02824998531657));
#45338=CARTESIAN_POINT('Ctrl Pts',(-4.1909009272832,4.02664892833259,-8.0335833359405));
#45339=CARTESIAN_POINT('Ctrl Pts',(-4.1991936928912,4.06473395988767,-8.03946758096497));
#45340=CARTESIAN_POINT('Ctrl Pts',(-4.20733446973179,4.10202191456589,-8.04577395397839));
#45341=CARTESIAN_POINT('Ctrl Pts',(-4.20886954901462,4.10905318048147,-8.04696312581693));
#45342=CARTESIAN_POINT('Ctrl Pts',(-4.21039915134647,4.1160561479542,-8.04816743038948));
#45343=CARTESIAN_POINT('Ctrl Pts',(-4.21192302832599,4.12303127501757,-8.04938617576649));
#45344=CARTESIAN_POINT('Ctrl Pts',(-4.21726041505002,4.14746169235889,-8.05365483753029));
#45345=CARTESIAN_POINT('Ctrl Pts',(-4.22253071088453,4.17154825128124,-8.05809915532785));
#45346=CARTESIAN_POINT('Ctrl Pts',(-4.22773274177579,4.19529368186173,-8.06268543417868));
#45347=CARTESIAN_POINT('Ctrl Pts',(-4.23698174367817,4.2375121033211,-8.07083965369463));
#45348=CARTESIAN_POINT('Ctrl Pts',(-4.24601616520686,4.27865162459762,-8.07943996562046));
#45349=CARTESIAN_POINT('Ctrl Pts',(-4.25481156728255,4.31874039069041,-8.08833311795105));
#45350=CARTESIAN_POINT('Ctrl Pts',(-4.25722631479631,4.32974662410862,-8.09077470246248));
#45351=CARTESIAN_POINT('Ctrl Pts',(-4.2596229178289,4.34067372356152,-8.0932386297565));
#45352=CARTESIAN_POINT('Ctrl Pts',(-4.26200060082954,4.35152238842346,-8.09572233653976));
#45353=CARTESIAN_POINT('Ctrl Pts',(-4.27113966826723,4.39322125229864,-8.10526892613202));
#45354=CARTESIAN_POINT('Ctrl Pts',(-4.2800021224755,4.43375752535204,-8.11510280598522));
#45355=CARTESIAN_POINT('Ctrl Pts',(-4.28859717867311,4.47321716789487,-8.12509676633268));
#45356=CARTESIAN_POINT('Ctrl Pts',(-4.29404107442491,4.49820992832222,-8.13142669333121));
#45357=CARTESIAN_POINT('Ctrl Pts',(-4.29937709674632,4.5227709357553,-8.13782181610565));
#45358=CARTESIAN_POINT('Ctrl Pts',(-4.3046026461297,4.54692215970033,-8.14425930542139));
#45359=CARTESIAN_POINT('Ctrl Pts',(-4.30548872710659,4.55101741142147,-8.14535089147351));
#45360=CARTESIAN_POINT('Ctrl Pts',(-4.30637162427403,4.55510087926121,-8.14644371200622));
#45361=CARTESIAN_POINT('Ctrl Pts',(-4.30725131830165,4.5591726673425,-8.14753767543186));
#45362=CARTESIAN_POINT('Ctrl Pts',(-4.31619737143733,4.60058073809078,-8.15866274236079));
#45363=CARTESIAN_POINT('Ctrl Pts',(-4.32481660242633,4.64077948467494,-8.16990037622455));
#45364=CARTESIAN_POINT('Ctrl Pts',(-4.33313053238231,4.67989643024333,-8.18116017355279));
#45365=CARTESIAN_POINT('Ctrl Pts',(-4.33806753938206,4.70312499183843,-8.18784650583121));
#45366=CARTESIAN_POINT('Ctrl Pts',(-4.34289632261169,4.72597200984736,-8.19454158619059));
#45367=CARTESIAN_POINT('Ctrl Pts',(-4.34761742866533,4.74846286165763,-8.20123397235553));
#45368=CARTESIAN_POINT('Ctrl Pts',(-4.35611858405088,4.78896147020831,-8.21328475326194));
#45369=CARTESIAN_POINT('Ctrl Pts',(-4.364273915394,4.82830494345656,-8.22532315857519));
#45370=CARTESIAN_POINT('Ctrl Pts',(-4.37211914663514,4.86667596289883,-8.23730455666148));
#45371=CARTESIAN_POINT('Ctrl Pts',(-4.37368661971269,4.87434247241082,-8.23969843370021));
#45372=CARTESIAN_POINT('Ctrl Pts',(-4.37524162712662,4.88197012218228,-8.242090172428));
#45373=CARTESIAN_POINT('Ctrl Pts',(-4.37678433287212,4.88956030660734,-8.2444796159815));
#45374=CARTESIAN_POINT('Ctrl Pts',(-4.37902935186565,4.90060590506209,-8.2479568482257));
#45375=CARTESIAN_POINT('Ctrl Pts',(-4.38124832515402,4.91157216617416,-8.25142920855899));
#45376=CARTESIAN_POINT('Ctrl Pts',(-4.38344168155448,4.92246328084618,-8.25489644172617));
#45377=CARTESIAN_POINT('Ctrl Pts',(-4.39166806457672,4.96331139874085,-8.26790061562817));
#45378=CARTESIAN_POINT('Ctrl Pts',(-4.39953784164126,5.00310352140156,-8.28082847158412));
#45379=CARTESIAN_POINT('Ctrl Pts',(-4.40710031519932,5.0420845185481,-8.29367497391344));
#45380=CARTESIAN_POINT('Ctrl Pts',(-4.40987453259679,5.05638430546631,-8.29838758414408));
#45381=CARTESIAN_POINT('Ctrl Pts',(-4.41260709492868,5.07057477963414,-8.30308964658198));
#45382=CARTESIAN_POINT('Ctrl Pts',(-4.41529949361838,5.08466746076063,-8.30778221778098));
#45383=CARTESIAN_POINT('Ctrl Pts',(-4.42221585975252,5.12086943294823,-8.31983672540163));
#45384=CARTESIAN_POINT('Ctrl Pts',(-4.42886821819497,5.15642611577934,-8.33182742100887));
#45385=CARTESIAN_POINT('Ctrl Pts',(-4.43533386389712,5.19175782809657,-8.34384585123646));
#45386=CARTESIAN_POINT('Ctrl Pts',(-4.43824630695621,5.20767295939887,-8.34925954003258));
#45387=CARTESIAN_POINT('Ctrl Pts',(-4.44112032917328,5.22354220343738,-8.3546793029189));
#45388=CARTESIAN_POINT('Ctrl Pts',(-4.44396054595061,5.2394028053282,-8.36011551828689));
#45389=CARTESIAN_POINT('Ctrl Pts',(-4.44405208094427,5.23991396352748,-8.36029071756857));
#45390=CARTESIAN_POINT('Ctrl Pts',(-4.4441435811585,5.24042511291043,-8.36046593366695));
#45391=CARTESIAN_POINT('Ctrl Pts',(-4.44423504674774,5.24093625444961,-8.36064116678035));
#45392=CARTESIAN_POINT('Ctrl Pts',(-4.45126642086968,5.28023001968963,-8.37411212989425));
#45393=CARTESIAN_POINT('Ctrl Pts',(-4.4580969244534,5.31947864261195,-8.38768154521493));
#45394=CARTESIAN_POINT('Ctrl Pts',(-4.46477647644197,5.35911589791667,-8.40145256371401));
#45395=CARTESIAN_POINT('Ctrl Pts',(-4.46669136199904,5.37047905637922,-8.40540042196486));
#45396=CARTESIAN_POINT('Ctrl Pts',(-4.46859356314506,5.38187406300918,-8.40936500143831));
#45397=CARTESIAN_POINT('Ctrl Pts',(-4.47048359648073,5.39331091775106,-8.41334907958716));
#45398=CARTESIAN_POINT('Ctrl Pts',(-4.47856333289223,5.44220252719894,-8.43038068462712));
#45399=CARTESIAN_POINT('Ctrl Pts',(-4.4864278178208,5.49186297696528,-8.4477622190913));
#45400=CARTESIAN_POINT('Ctrl Pts',(-4.49394679880183,5.5418615608125,-8.46523514881534));
#45401=CARTESIAN_POINT('Ctrl Pts',(-4.4944017865307,5.54488706947768,-8.46629246876759));
#45402=CARTESIAN_POINT('Ctrl Pts',(-4.49485551848749,5.54791382557571,-8.46735011515994));
#45403=CARTESIAN_POINT('Ctrl Pts',(-4.49530796933741,5.55094173716409,-8.46840802772342));
#45404=CARTESIAN_POINT('Ctrl Pts',(-4.49842936112357,5.57183085332511,-8.47570641071172));
#45405=CARTESIAN_POINT('Ctrl Pts',(-4.50148971645701,5.59277488701679,-8.48301746154873));
#45406=CARTESIAN_POINT('Ctrl Pts',(-4.50448016791163,5.61373871123014,-8.49031968227011));
#45407=CARTESIAN_POINT('Ctrl Pts',(-4.50908658699107,5.64603087891788,-8.50156784642317));
#45408=CARTESIAN_POINT('Ctrl Pts',(-4.51352685215888,5.67836985658108,-8.51279513010456));
#45409=CARTESIAN_POINT('Ctrl Pts',(-4.51777558989158,5.71063032301425,-8.52392064421601));
#45410=CARTESIAN_POINT('Ctrl Pts',(-4.52302272751204,5.75047159299255,-8.53766051410537));
#45411=CARTESIAN_POINT('Ctrl Pts',(-4.52797840478413,5.7901902785537,-8.55124943731126));
#45412=CARTESIAN_POINT('Ctrl Pts',(-4.5326783182324,5.83017642858429,-8.56472139707146));
#45413=CARTESIAN_POINT('Ctrl Pts',(-4.53425463127801,5.84358746064495,-8.56923978366596));
#45414=CARTESIAN_POINT('Ctrl Pts',(-4.53580175308728,5.85702853586363,-8.57374510959597));
#45415=CARTESIAN_POINT('Ctrl Pts',(-4.5373197575171,5.87051423416948,-8.57823892982017));
#45416=CARTESIAN_POINT('Ctrl Pts',(-4.5407839353761,5.90128941279634,-8.58849409918404));
#45417=CARTESIAN_POINT('Ctrl Pts',(-4.54409817423199,5.93229529921562,-8.59869252527202));
#45418=CARTESIAN_POINT('Ctrl Pts',(-4.54729858503435,5.96400552331454,-8.60889569284174));
#45419=CARTESIAN_POINT('Ctrl Pts',(-4.54906917871499,5.98154887192456,-8.61454048819366));
#45420=CARTESIAN_POINT('Ctrl Pts',(-4.55080405929922,5.99930777943827,-8.62018683029092));
#45421=CARTESIAN_POINT('Ctrl Pts',(-4.55250246845951,6.01736224798488,-8.62584575846157));
#45422=CARTESIAN_POINT('Ctrl Pts',(-4.5530903412421,6.02361146690753,-8.62780449133231));
#45423=CARTESIAN_POINT('Ctrl Pts',(-4.55367379927466,6.02989609461737,-8.62976473564345));
#45424=CARTESIAN_POINT('Ctrl Pts',(-4.55425268031317,6.03621944303901,-8.6317269597769));
#45425=CARTESIAN_POINT('Ctrl Pts',(-4.55790067810912,6.07606797766111,-8.64409252167612));
#45426=CARTESIAN_POINT('Ctrl Pts',(-4.56137444979074,6.11745813508607,-8.65653174714067));
#45427=CARTESIAN_POINT('Ctrl Pts',(-4.56459141140092,6.16021282589141,-8.66862512082167));
#45428=CARTESIAN_POINT('Ctrl Pts',(-4.56602514958334,6.17926777279885,-8.67401490587408));
#45429=CARTESIAN_POINT('Ctrl Pts',(-4.56740721900955,6.19859409140341,-8.67933586498138));
#45430=CARTESIAN_POINT('Ctrl Pts',(-4.56872735814743,6.21817739199662,-8.68455045311303));
#45431=CARTESIAN_POINT('',(-4.55640048587279,6.70157635552431,-8.9543685982643));
#45432=CARTESIAN_POINT('Ctrl Pts',(-4.55640048587279,6.70157635552431,-8.9543685982643));
#45433=CARTESIAN_POINT('Ctrl Pts',(-4.55718941624934,6.67123679535193,-8.93709741994231));
#45434=CARTESIAN_POINT('Ctrl Pts',(-4.55798670386089,6.64094052514093,-8.9197505370997));
#45435=CARTESIAN_POINT('Ctrl Pts',(-4.56052339181447,6.54280654655596,-8.86421763865645));
#45436=CARTESIAN_POINT('Ctrl Pts',(-4.56140069340555,6.50873740836523,-8.84501184706769));
#45437=CARTESIAN_POINT('Ctrl Pts',(-4.56478339758665,6.37642811190917,-8.77095805283272));
#45438=CARTESIAN_POINT('Ctrl Pts',(-4.56675535639669,6.29828421554187,-8.72778814374827));
#45439=CARTESIAN_POINT('Ctrl Pts',(-4.56873070446287,6.21818495489539,-8.68454403743452));
#45440=CARTESIAN_POINT('Origin',(-1.55120871661933,6.72678389660421,-8.99999785420734));
#45441=CARTESIAN_POINT('Ctrl Pts',(-4.045081305886,3.570670526222,-7.997140252951));
#45442=CARTESIAN_POINT('Ctrl Pts',(-4.046812898614,3.579264725453,-7.997221249461));
#45443=CARTESIAN_POINT('Ctrl Pts',(-4.067641295895,3.682284597448,-7.998756172751));
#45444=CARTESIAN_POINT('Ctrl Pts',(-4.107485147684,3.871753164572,-8.0136447426));
#45445=CARTESIAN_POINT('Ctrl Pts',(-4.164985230409,4.131365060025,-8.057273037248));
#45446=CARTESIAN_POINT('Ctrl Pts',(-4.218249503093,4.365529545906,-8.111730462255));
#45447=CARTESIAN_POINT('Ctrl Pts',(-4.266684104315,4.577338170023,-8.170825174353));
#45448=CARTESIAN_POINT('Ctrl Pts',(-4.310160116143,4.769912949898,-8.230914655747));
#45449=CARTESIAN_POINT('Ctrl Pts',(-4.349046949732,4.946950105447,-8.290246855678));
#45450=CARTESIAN_POINT('Ctrl Pts',(-4.384026666367,5.112794198023,-8.348441680794));
#45451=CARTESIAN_POINT('Ctrl Pts',(-4.416117162443,5.273132430747,-8.406311113417));
#45452=CARTESIAN_POINT('Ctrl Pts',(-4.446085672278,5.433323459631,-8.464981611408));
#45453=CARTESIAN_POINT('Ctrl Pts',(-4.473991447656,5.595899742481,-8.52460059918));
#45454=CARTESIAN_POINT('Ctrl Pts',(-4.499372620983,5.761043207801,-8.584261950216));
#45455=CARTESIAN_POINT('Ctrl Pts',(-4.522096645264,5.931133599072,-8.643540441466));
#45456=CARTESIAN_POINT('Ctrl Pts',(-4.539342084936,6.086914371239,-8.694069503927));
#45457=CARTESIAN_POINT('Ctrl Pts',(-4.548382886192,6.188750654892,-8.723456408556));
#45458=CARTESIAN_POINT('Ctrl Pts',(-4.551596987486,6.22933872244,-8.734309456469));
#45459=CARTESIAN_POINT('Ctrl Pts',(-4.38444310932,3.571151919152,-8.034638616021));
#45460=CARTESIAN_POINT('Ctrl Pts',(-4.386305205191,3.579569394099,-8.033539372566));
#45461=CARTESIAN_POINT('Ctrl Pts',(-4.408629897612,3.68066734286,-8.020861884741));
#45462=CARTESIAN_POINT('Ctrl Pts',(-4.449669636584,3.870894091304,-8.008352060743));
#45463=CARTESIAN_POINT('Ctrl Pts',(-4.504232539929,4.140353391516,-8.013736794392));
#45464=CARTESIAN_POINT('Ctrl Pts',(-4.55063177438,4.389097996571,-8.034425921765));
#45465=CARTESIAN_POINT('Ctrl Pts',(-4.589150445557,4.617533446599,-8.064277722446));
#45466=CARTESIAN_POINT('Ctrl Pts',(-4.620473992277,4.827070553768,-8.099234200262));
#45467=CARTESIAN_POINT('Ctrl Pts',(-4.645574637769,5.020459022684,-8.136859011721));
#45468=CARTESIAN_POINT('Ctrl Pts',(-4.665466157709,5.201634738077,-8.176014130233));
#45469=CARTESIAN_POINT('Ctrl Pts',(-4.681108266095,5.376219387118,-8.216640487237));
#45470=CARTESIAN_POINT('Ctrl Pts',(-4.693013028977,5.549502857778,-8.259177343643));
#45471=CARTESIAN_POINT('Ctrl Pts',(-4.701160151981,5.723479739884,-8.303369398396));
#45472=CARTESIAN_POINT('Ctrl Pts',(-4.705392710052,5.897297469717,-8.348024465499));
#45473=CARTESIAN_POINT('Ctrl Pts',(-4.70577776434,6.071962157169,-8.39204144798));
#45474=CARTESIAN_POINT('Ctrl Pts',(-4.702814699302,6.225389199561,-8.427814383606));
#45475=CARTESIAN_POINT('Ctrl Pts',(-4.699547889202,6.319867306073,-8.446724606978));
#45476=CARTESIAN_POINT('Ctrl Pts',(-4.698140530724,6.356053961272,-8.453204386312));
#45477=CARTESIAN_POINT('Ctrl Pts',(-4.628389217157,3.568085518823,-7.795779646061));
#45478=CARTESIAN_POINT('Ctrl Pts',(-4.629418893889,3.577521107695,-7.79381729154));
#45479=CARTESIAN_POINT('Ctrl Pts',(-4.641684342718,3.690860050951,-7.770895214064));
#45480=CARTESIAN_POINT('Ctrl Pts',(-4.662425768587,3.904374357362,-7.741811913326));
#45481=CARTESIAN_POINT('Ctrl Pts',(-4.684742285256,4.205673471946,-7.730144464707));
#45482=CARTESIAN_POINT('Ctrl Pts',(-4.698645983965,4.481620469159,-7.740018549965));
#45483=CARTESIAN_POINT('Ctrl Pts',(-4.705289198756,4.732378398938,-7.7636822036));
#45484=CARTESIAN_POINT('Ctrl Pts',(-4.705941242827,4.959625634746,-7.795795708981));
#45485=CARTESIAN_POINT('Ctrl Pts',(-4.701760894077,5.16663338348,-7.832943907084));
#45486=CARTESIAN_POINT('Ctrl Pts',(-4.693611570147,5.357939474718,-7.873319066008));
#45487=CARTESIAN_POINT('Ctrl Pts',(-4.681878224428,5.539622768666,-7.916425840639));
#45488=CARTESIAN_POINT('Ctrl Pts',(-4.666505871274,5.717138279957,-7.962487458925));
#45489=CARTESIAN_POINT('Ctrl Pts',(-4.647392526364,5.892143191488,-8.010987241641));
#45490=CARTESIAN_POINT('Ctrl Pts',(-4.624818466659,6.063207414259,-8.060275721544));
#45491=CARTESIAN_POINT('Ctrl Pts',(-4.599047213946,6.230443318226,-8.108633744215));
#45492=CARTESIAN_POINT('Ctrl Pts',(-4.574172291028,6.371245573819,-8.146796806519));
#45493=CARTESIAN_POINT('Ctrl Pts',(-4.558333187126,6.452902211151,-8.165676958464));
#45494=CARTESIAN_POINT('Ctrl Pts',(-4.552300465109,6.482885359553,-8.171767808125));
#45495=CARTESIAN_POINT('Ctrl Pts',(-4.59801848,3.563720111035,-7.455733771689));
#45496=CARTESIAN_POINT('Ctrl Pts',(-4.597863281049,3.574622004543,-7.453858409074));
#45497=CARTESIAN_POINT('Ctrl Pts',(-4.595891028734,3.705387762562,-7.432172570609));
#45498=CARTESIAN_POINT('Ctrl Pts',(-4.589725981319,3.947640760677,-7.409495091648));
#45499=CARTESIAN_POINT('Ctrl Pts',(-4.574135224093,4.279421944416,-7.414472286021));
#45500=CARTESIAN_POINT('Ctrl Pts',(-4.553743926439,4.57524436771,-7.444415940845));
#45501=CARTESIAN_POINT('Ctrl Pts',(-4.529928451882,4.83764994122,-7.489484372422));
#45502=CARTESIAN_POINT('Ctrl Pts',(-4.503883313521,5.07036714669,-7.543129868468));
#45503=CARTESIAN_POINT('Ctrl Pts',(-4.476400774158,5.278274260209,-7.601381759125));
#45504=CARTESIAN_POINT('Ctrl Pts',(-4.447822088052,5.467080233349,-7.662341972482));
#45505=CARTESIAN_POINT('Ctrl Pts',(-4.417862378173,5.643508514361,-7.725833610458));
#45506=CARTESIAN_POINT('Ctrl Pts',(-4.38600357872,5.813292041393,-7.792493462698));
#45507=CARTESIAN_POINT('Ctrl Pts',(-4.352119780053,5.978198493352,-7.861876504293));
#45508=CARTESIAN_POINT('Ctrl Pts',(-4.316740092663,6.137100758815,-7.932040118318));
#45509=CARTESIAN_POINT('Ctrl Pts',(-4.280177274426,6.290352797616,-8.001158170104));
#45510=CARTESIAN_POINT('Ctrl Pts',(-4.247756495264,6.41751776608,-8.057104781149));
#45511=CARTESIAN_POINT('Ctrl Pts',(-4.228300475361,6.490292438545,-8.086423524783));
#45512=CARTESIAN_POINT('Ctrl Pts',(-4.221030558413,6.516819410599,-8.096395010467));
#45513=CARTESIAN_POINT('',(-4.59947917151011,5.30712985987108,-8.01140192098629));
#45514=CARTESIAN_POINT('Ctrl Pts',(-4.56872994952894,6.2181719957563,-8.68456056436646));
#45515=CARTESIAN_POINT('Ctrl Pts',(-4.57549039229006,5.94407403599775,-8.53656168229868));
#45516=CARTESIAN_POINT('Ctrl Pts',(-4.58829230843072,5.57742483423423,-8.25630351813582));
#45517=CARTESIAN_POINT('Ctrl Pts',(-4.59463727532969,5.39767807259543,-8.1174001887258));
#45518=CARTESIAN_POINT('Ctrl Pts',(-4.59661627982459,5.34707828533855,-8.07407603627248));
#45519=CARTESIAN_POINT('Ctrl Pts',(-4.59817842627609,5.31873497780432,-8.03987769503683));
#45520=CARTESIAN_POINT('Ctrl Pts',(-4.59846257897685,5.31405574435703,-8.03365705483116));
#45521=CARTESIAN_POINT('Ctrl Pts',(-4.59885735472505,5.30945783900961,-8.02501466682989));
#45522=CARTESIAN_POINT('Ctrl Pts',(-4.59898970613569,5.3081737583618,-8.02211724405618));
#45523=CARTESIAN_POINT('Ctrl Pts',(-4.59918120343943,5.30709898285999,-8.01792500578503));
#45524=CARTESIAN_POINT('Ctrl Pts',(-4.59924313552705,5.30686343682691,-8.01656919521855));
#45525=CARTESIAN_POINT('Ctrl Pts',(-4.59936367370055,5.30673568281945,-8.01393038655558));
#45526=CARTESIAN_POINT('Ctrl Pts',(-4.59942203451764,5.3068253754564,-8.01265275785716));
#45527=CARTESIAN_POINT('Ctrl Pts',(-4.59947916602947,5.30713035297914,-8.01140204097648));
#45528=CARTESIAN_POINT('Origin',(-4.100000000002,3.596479003779,-7.500000152636));
#45529=CARTESIAN_POINT('Origin',(-4.16921629989938,5.30178033932293,-7.99516079097523));
#45530=CARTESIAN_POINT('Origin',(-4.6,0.,-8.));
#45531=CARTESIAN_POINT('',(-4.59947849846395,10.4125163640988,-8.01141603935184));
#45532=CARTESIAN_POINT('',(-4.599479171875,5.307129343005,-8.011401913));
#45533=CARTESIAN_POINT('',(-4.23,10.14289693909,-16.1));
#45534=CARTESIAN_POINT('',(-4.556403751801,6.701576438348,-8.954368601956));
#45535=CARTESIAN_POINT('Origin',(-3.762822538146,0.03215126727281,39.41676));
#45536=CARTESIAN_POINT('Origin',(0.2082147951869,9.091108462706,-47.51676));
#45537=CARTESIAN_POINT('',(-1.60105661523759,13.4097223134493,-8.00833023504569));
#45538=CARTESIAN_POINT('Ctrl Pts',(-4.59947852653901,10.4125163641,-8.01141604063367));
#45539=CARTESIAN_POINT('Ctrl Pts',(-4.59937714658466,10.5053599489842,-8.01363546696004));
#45540=CARTESIAN_POINT('Ctrl Pts',(-4.59496139431105,10.5981056187004,-8.01571294302175));
#45541=CARTESIAN_POINT('Ctrl Pts',(-4.58628390044264,10.6903162581727,-8.01764532333119));
#45542=CARTESIAN_POINT('Ctrl Pts',(-4.57759483258553,10.7826498876368,-8.01958028103776));
#45543=CARTESIAN_POINT('Ctrl Pts',(-4.56463275739157,10.8744466105326,-8.02136974578396));
#45544=CARTESIAN_POINT('Ctrl Pts',(-4.54750132154224,10.9652793145299,-8.02301327200983));
#45545=CARTESIAN_POINT('Ctrl Pts',(-4.54553480512527,10.9757059947673,-8.02320193227936));
#45546=CARTESIAN_POINT('Ctrl Pts',(-4.54351340395201,10.9861199893966,-8.0233886725801));
#45547=CARTESIAN_POINT('Ctrl Pts',(-4.54143731634338,10.9965206663834,-8.02357349460259));
#45548=CARTESIAN_POINT('Ctrl Pts',(-4.51373868008413,11.1352838705519,-8.02603934332322));
#45549=CARTESIAN_POINT('Ctrl Pts',(-4.47631109928855,11.2716724237222,-8.02816384317182));
#45550=CARTESIAN_POINT('Ctrl Pts',(-4.42949368679031,11.4047754243669,-8.02995529417993));
#45551=CARTESIAN_POINT('Ctrl Pts',(-4.41170336822207,11.4553537168761,-8.03063603415323));
#45552=CARTESIAN_POINT('Ctrl Pts',(-4.39255663241803,11.5054576939607,-8.03126866081907));
#45553=CARTESIAN_POINT('Ctrl Pts',(-4.37207018210256,11.5550370833454,-8.03185353288804));
#45554=CARTESIAN_POINT('Ctrl Pts',(-4.33487064946315,11.6450639101143,-8.03291555033294));
#45555=CARTESIAN_POINT('Ctrl Pts',(-4.29325008333227,11.7333572007709,-8.03381981135128));
#45556=CARTESIAN_POINT('Ctrl Pts',(-4.24739909147331,11.8194638381191,-8.03456476480664));
#45557=CARTESIAN_POINT('Ctrl Pts',(-4.20154809961434,11.9055704754674,-8.03530971826199));
#45558=CARTESIAN_POINT('Ctrl Pts',(-4.15146687069939,11.9894900264455,-8.03589535833731));
#45559=CARTESIAN_POINT('Ctrl Pts',(-4.09739699750768,12.070792842957,-8.03632324514469));
#45560=CARTESIAN_POINT('Ctrl Pts',(-4.04332712431596,12.1520956594685,-8.03675113195206));
#45561=CARTESIAN_POINT('Ctrl Pts',(-3.98526494673421,12.2307867534014,-8.03702126536406));
#45562=CARTESIAN_POINT('Ctrl Pts',(-3.92350391936216,12.306459541199,-8.03713533101613));
#45563=CARTESIAN_POINT('Ctrl Pts',(-3.8617428919901,12.3821323289966,-8.0372493966682));
#45564=CARTESIAN_POINT('Ctrl Pts',(-3.79628334587537,12.4547864053715,-8.03720739617268));
#45565=CARTESIAN_POINT('Ctrl Pts',(-3.7274646744854,12.5240527119111,-8.03701436444527));
#45566=CARTESIAN_POINT('Ctrl Pts',(-3.61008311621264,12.6421977855254,-8.03668511709856));
#45567=CARTESIAN_POINT('Ctrl Pts',(-3.48294186288595,12.7504976082822,-8.03591742735363));
#45568=CARTESIAN_POINT('Ctrl Pts',(-3.34726077786289,12.8477785188959,-8.03473979822533));
#45569=CARTESIAN_POINT('Ctrl Pts',(-3.32384716110428,12.86456566324,-8.0345365823011));
#45570=CARTESIAN_POINT('Ctrl Pts',(-3.30017927632364,12.8810245622901,-8.03432115655264));
#45571=CARTESIAN_POINT('Ctrl Pts',(-3.27626347960308,12.8971490029899,-8.03409366538231));
#45572=CARTESIAN_POINT('Ctrl Pts',(-3.19500998112919,12.9519315065,-8.03332076813462));
#45573=CARTESIAN_POINT('Ctrl Pts',(-3.11089288436003,13.0028487928325,-8.03240835728523));
#45574=CARTESIAN_POINT('Ctrl Pts',(-3.02431349873321,13.0495898432854,-8.03136655596011));
#45575=CARTESIAN_POINT('Ctrl Pts',(-2.93773411310639,13.0963308937382,-8.03032475463499));
#45576=CARTESIAN_POINT('Ctrl Pts',(-2.84869282192845,13.1388953619482,-8.02915356879778));
#45577=CARTESIAN_POINT('Ctrl Pts',(-2.75762808262276,13.1770189882356,-8.02786637709185));
#45578=CARTESIAN_POINT('Ctrl Pts',(-2.6767553243985,13.2108758117974,-8.02672324810016));
#45579=CARTESIAN_POINT('Ctrl Pts',(-2.59428155331456,13.2412318658843,-8.02548844708348));
#45580=CARTESIAN_POINT('Ctrl Pts',(-2.51057491999558,13.2679253202654,-8.02417544528473));
#45581=CARTESIAN_POINT('Ctrl Pts',(-2.42689667427439,13.2946097220419,-8.02286288876689));
#45582=CARTESIAN_POINT('Ctrl Pts',(-2.3419868696778,13.3176338274672,-8.02147219982988));
#45583=CARTESIAN_POINT('Ctrl Pts',(-2.25623169518505,13.3368846145964,-8.02001929854991));
#45584=CARTESIAN_POINT('Ctrl Pts',(-2.23458069613051,13.341744948406,-8.01965247795366));
#45585=CARTESIAN_POINT('Ctrl Pts',(-2.21287588198184,13.3463650071242,-8.01928170330574));
#45586=CARTESIAN_POINT('Ctrl Pts',(-2.19112359772689,13.3507434805461,-8.01890725370485));
#45587=CARTESIAN_POINT('Ctrl Pts',(-2.08550224293537,13.3720037900068,-8.01708905963921));
#45588=CARTESIAN_POINT('Ctrl Pts',(-1.97875576869714,13.3875653723446,-8.01518385709241));
#45589=CARTESIAN_POINT('Ctrl Pts',(-1.87146594973527,13.3973435107752,-8.01324431200059));
#45590=CARTESIAN_POINT('Ctrl Pts',(-1.781595528025,13.4055340868504,-8.01161966823649));
#45591=CARTESIAN_POINT('Ctrl Pts',(-1.6913440848234,13.4096676346005,-8.0099709675611));
#45592=CARTESIAN_POINT('Ctrl Pts',(-1.601056615238,13.4097223254853,-8.00833023544683));
#45593=CARTESIAN_POINT('',(-1.231437138339,13.14,-16.1));
#45594=CARTESIAN_POINT('Ctrl Pts',(-4.598789897208,10.36225164745,-8.016476101857));
#45595=CARTESIAN_POINT('Ctrl Pts',(-4.59904872628,10.37845482038,-8.016780636338));
#45596=CARTESIAN_POINT('Ctrl Pts',(-4.600707128738,10.59084307586,-8.020727567036));
#45597=CARTESIAN_POINT('Ctrl Pts',(-4.560432831713,10.99871853828,-8.027206255404));
#45598=CARTESIAN_POINT('Ctrl Pts',(-4.389548448443,11.56244686259,-8.033690401801));
#45599=CARTESIAN_POINT('Ctrl Pts',(-4.113161687858,12.08156245964,-8.03737709449));
#45600=CARTESIAN_POINT('Ctrl Pts',(-3.740911740519,12.53762144943,-8.038338406857));
#45601=CARTESIAN_POINT('Ctrl Pts',(-3.285897948442,12.91378212525,-8.036724743215));
#45602=CARTESIAN_POINT('Ctrl Pts',(-2.763990158324,13.19524941593,-8.032801897215));
#45603=CARTESIAN_POINT('Ctrl Pts',(-2.194549095368,13.36974564586,-8.027048720184));
#45604=CARTESIAN_POINT('Ctrl Pts',(-1.782256775266,13.41072702305,-8.022378740496));
#45605=CARTESIAN_POINT('Ctrl Pts',(-1.568450922092,13.40904708803,-8.020131894078));
#45606=CARTESIAN_POINT('Ctrl Pts',(-1.552548505891,13.40879470923,-8.019965863476));
#45607=CARTESIAN_POINT('Ctrl Pts',(-4.599357509043,10.36246318279,-8.006699568108));
#45608=CARTESIAN_POINT('Ctrl Pts',(-4.599615170043,10.37866779227,-8.007004055868));
#45609=CARTESIAN_POINT('Ctrl Pts',(-4.60125828296,10.59107480655,-8.010950502452));
#45610=CARTESIAN_POINT('Ctrl Pts',(-4.560955080986,10.99898457628,-8.017428460088));
#45611=CARTESIAN_POINT('Ctrl Pts',(-4.39003073768,11.56275691357,-8.0239118523));
#45612=CARTESIAN_POINT('Ctrl Pts',(-4.113605718657,12.08191367378,-8.027598129646));
#45613=CARTESIAN_POINT('Ctrl Pts',(-3.741317226717,12.53801415694,-8.028559340472));
#45614=CARTESIAN_POINT('Ctrl Pts',(-3.286260517087,12.91421890722,-8.026945846688));
#45615=CARTESIAN_POINT('Ctrl Pts',(-2.764299375992,13.19573306602,-8.023023342469));
#45616=CARTESIAN_POINT('Ctrl Pts',(-2.194786161204,13.37027585393,-8.017270521009));
#45617=CARTESIAN_POINT('Ctrl Pts',(-1.782422450544,13.41128407841,-8.012600588629));
#45618=CARTESIAN_POINT('Ctrl Pts',(-1.568567787561,13.40961256521,-8.010353640725));
#45619=CARTESIAN_POINT('Ctrl Pts',(-1.552661674054,13.40936077555,-8.01018761061));
#45620=CARTESIAN_POINT('Ctrl Pts',(-4.599637634666,10.36267951191,-7.996910682916));
#45621=CARTESIAN_POINT('Ctrl Pts',(-4.599894101587,10.37888400298,-7.997215123896));
#45622=CARTESIAN_POINT('Ctrl Pts',(-4.601521750683,10.59128939393,-8.001161085754));
#45623=CARTESIAN_POINT('Ctrl Pts',(-4.561193484141,10.99919432699,-8.007638311736));
#45624=CARTESIAN_POINT('Ctrl Pts',(-4.390245555465,11.56295657265,-8.01412094881));
#45625=CARTESIAN_POINT('Ctrl Pts',(-4.113808788278,12.08210467379,-8.017806810288));
#45626=CARTESIAN_POINT('Ctrl Pts',(-3.741517469637,12.53820288521,-8.018767919443));
#45627=CARTESIAN_POINT('Ctrl Pts',(-3.286461505785,12.91441562184,-8.017154595732));
#45628=CARTESIAN_POINT('Ctrl Pts',(-2.764497092176,13.19594965895,-8.013232433727));
#45629=CARTESIAN_POINT('Ctrl Pts',(-2.194966351295,13.37052228964,-8.007479968285));
#45630=CARTESIAN_POINT('Ctrl Pts',(-1.782570781966,13.41155345129,-8.002810083274));
#45631=CARTESIAN_POINT('Ctrl Pts',(-1.568687797996,13.40989052953,-8.000563033756));
#45632=CARTESIAN_POINT('Ctrl Pts',(-1.552779511032,13.40963935383,-8.000397004128));
#45633=CARTESIAN_POINT('Ctrl Pts',(-4.59963003227,10.36290044807,-7.987117896224));
#45634=CARTESIAN_POINT('Ctrl Pts',(-4.599885280135,10.37910326588,-7.987422290406));
#45635=CARTESIAN_POINT('Ctrl Pts',(-4.601497304476,10.59148665279,-7.991367767344));
#45636=CARTESIAN_POINT('Ctrl Pts',(-4.561147835383,10.99934760934,-7.997844261379));
#45637=CARTESIAN_POINT('Ctrl Pts',(-4.390192716364,11.56304566748,-8.004326143015));
#45638=CARTESIAN_POINT('Ctrl Pts',(-4.113770721428,12.08213529482,-8.00801158846));
#45639=CARTESIAN_POINT('Ctrl Pts',(-3.741512296425,12.53818747134,-8.008972595904));
#45640=CARTESIAN_POINT('Ctrl Pts',(-3.286500741038,12.91437209929,-8.007359442333));
#45641=CARTESIAN_POINT('Ctrl Pts',(-2.764583136204,13.19589900775,-8.003437622678));
#45642=CARTESIAN_POINT('Ctrl Pts',(-2.1950895101,13.37048474024,-7.997685513398));
#45643=CARTESIAN_POINT('Ctrl Pts',(-1.78270164149,13.41153490917,-7.993015675774));
#45644=CARTESIAN_POINT('Ctrl Pts',(-1.568810849802,13.40988074104,-7.990768524601));
#45645=CARTESIAN_POINT('Ctrl Pts',(-1.552901915106,13.4096302036,-7.99060249546));
#45646=CARTESIAN_POINT('Origin',(-4.16374842361929,10.412721159634,-7.98938980904604));
#45647=CARTESIAN_POINT('',(-1.59999999919565,13.4100000197175,-7.99166557366509));
#45648=CARTESIAN_POINT('Ctrl Pts',(-4.60000007096128,10.4099999970624,-7.98856626783489));
#45649=CARTESIAN_POINT('Ctrl Pts',(-4.60000004790308,10.4105031362908,-7.98857551592105));
#45650=CARTESIAN_POINT('Ctrl Pts',(-4.59999989765145,10.4110062701598,-7.98858476064926));
#45651=CARTESIAN_POINT('Ctrl Pts',(-4.59999962022458,10.4115093985946,-7.98859400202004));
#45652=CARTESIAN_POINT('Ctrl Pts',(-4.59993230689588,10.5335857136227,-7.99083627737669));
#45653=CARTESIAN_POINT('Ctrl Pts',(-4.59237725989827,10.6553379562347,-7.99288087440913));
#45654=CARTESIAN_POINT('Ctrl Pts',(-4.57759893061383,10.7757227708346,-7.99473560830003));
#45655=CARTESIAN_POINT('Ctrl Pts',(-4.56846846564521,10.8500998747211,-7.99588151474798));
#45656=CARTESIAN_POINT('Ctrl Pts',(-4.55658096803786,10.923955981217,-7.99695495345506));
#45657=CARTESIAN_POINT('Ctrl Pts',(-4.54200043259281,10.9970548991584,-7.99795781611259));
#45658=CARTESIAN_POINT('Ctrl Pts',(-4.52558397978909,11.0793581136673,-7.99908695485703));
#45659=CARTESIAN_POINT('Ctrl Pts',(-4.50575945226007,11.1606958296678,-8.0001261358151));
#45660=CARTESIAN_POINT('Ctrl Pts',(-4.48262123061731,11.2409571557528,-8.0010784943899));
#45661=CARTESIAN_POINT('Ctrl Pts',(-4.45934493853253,11.3216974173819,-8.00203653588067));
#45662=CARTESIAN_POINT('Ctrl Pts',(-4.43271510472733,11.4013490785121,-8.0029067152227));
#45663=CARTESIAN_POINT('Ctrl Pts',(-4.40277644619052,11.4797889721212,-8.00369093516911));
#45664=CARTESIAN_POINT('Ctrl Pts',(-4.39308369326812,11.5051841816988,-8.00394482931631));
#45665=CARTESIAN_POINT('Ctrl Pts',(-4.38304373262649,11.5304522553539,-8.00418970349656));
#45666=CARTESIAN_POINT('Ctrl Pts',(-4.3726569846437,11.5555886022102,-8.00442559364283));
#45667=CARTESIAN_POINT('Ctrl Pts',(-4.32570548047689,11.6692131260859,-8.0054918943949));
#45668=CARTESIAN_POINT('Ctrl Pts',(-4.27166654431615,11.780135431829,-8.00637598720223));
#45669=CARTESIAN_POINT('Ctrl Pts',(-4.21097666130231,11.8874037929216,-8.00707791501786));
#45670=CARTESIAN_POINT('Ctrl Pts',(-4.1755470119615,11.9500251101847,-8.00748768770377));
#45671=CARTESIAN_POINT('Ctrl Pts',(-4.13785171758996,12.0114012978217,-8.00783540238063));
#45672=CARTESIAN_POINT('Ctrl Pts',(-4.09798539657222,12.0713455265286,-8.00812126625666));
#45673=CARTESIAN_POINT('Ctrl Pts',(-4.01821661670886,12.1912883218939,-8.00869325313722));
#45674=CARTESIAN_POINT('Ctrl Pts',(-3.92974727531656,12.3055066806468,-8.0090173854157));
#45675=CARTESIAN_POINT('Ctrl Pts',(-3.83357869973105,12.4127697983396,-8.00910502114443));
#45676=CARTESIAN_POINT('Ctrl Pts',(-3.79935520257316,12.450941508601,-8.0091362080586));
#45677=CARTESIAN_POINT('Ctrl Pts',(-3.76415703204153,12.4882326737266,-8.00913745552344));
#45678=CARTESIAN_POINT('Ctrl Pts',(-3.7280304834056,12.5245889108034,-8.009109311589));
#45679=CARTESIAN_POINT('Ctrl Pts',(-3.65853132117118,12.5945299407175,-8.00905516913865));
#45680=CARTESIAN_POINT('Ctrl Pts',(-3.58560242986534,12.6610112485787,-8.00889192038084));
#45681=CARTESIAN_POINT('Ctrl Pts',(-3.50950976494343,12.7238085936419,-8.00862540876549));
#45682=CARTESIAN_POINT('Ctrl Pts',(-3.43490130270294,12.7853810639024,-8.00836409551261));
#45683=CARTESIAN_POINT('Ctrl Pts',(-3.35725059062315,12.843412269591,-8.00800349515826));
#45684=CARTESIAN_POINT('Ctrl Pts',(-3.27678144871871,12.8976502915845,-8.00754815778184));
#45685=CARTESIAN_POINT('Ctrl Pts',(-3.17058765355902,12.9692273118077,-8.00694725658));
#45686=CARTESIAN_POINT('Ctrl Pts',(-3.05948306544671,13.0341866726464,-8.0061819433219));
#45687=CARTESIAN_POINT('Ctrl Pts',(-2.94441965585415,13.0918749035054,-8.00527351756899));
#45688=CARTESIAN_POINT('Ctrl Pts',(-2.88336825523829,13.1224836548492,-8.00479151668994));
#45689=CARTESIAN_POINT('Ctrl Pts',(-2.82120321813055,13.1510457395272,-8.00426925202656));
#45690=CARTESIAN_POINT('Ctrl Pts',(-2.7580719769513,13.1774662231341,-8.00371006450633));
#45691=CARTESIAN_POINT('Ctrl Pts',(-2.64703765376743,13.2239341914599,-8.00272657350122));
#45692=CARTESIAN_POINT('Ctrl Pts',(-2.5330062475374,13.2637771321126,-8.00162880440515));
#45693=CARTESIAN_POINT('Ctrl Pts',(-2.41686575149847,13.2966459179422,-8.00044945974601));
#45694=CARTESIAN_POINT('Ctrl Pts',(-2.34251676502126,13.317687337572,-7.99969448552853));
#45695=CARTESIAN_POINT('Ctrl Pts',(-2.26730415745375,13.335871528974,-7.99890610901898));
#45696=CARTESIAN_POINT('Ctrl Pts',(-2.19146614940064,13.3511167596878,-7.9980931203695));
#45697=CARTESIAN_POINT('Ctrl Pts',(-2.08209765432325,13.3731024101957,-7.99692068259864));
#45698=CARTESIAN_POINT('Ctrl Pts',(-1.9714303709993,13.3889811469719,-7.9956970407022));
#45699=CARTESIAN_POINT('Ctrl Pts',(-1.86013185012544,13.3986735280725,-7.9944767393174));
#45700=CARTESIAN_POINT('Ctrl Pts',(-1.77390717570491,13.4061823646519,-7.9935313530825));
#45701=CARTESIAN_POINT('Ctrl Pts',(-1.68730334299757,13.4099772619015,-7.99258795667504));
#45702=CARTESIAN_POINT('Ctrl Pts',(-1.6006338528752,13.4099999330244,-7.99167226999386));
#45703=CARTESIAN_POINT('Ctrl Pts',(-1.60042256870131,13.4099999882924,-7.99167003771923));
#45704=CARTESIAN_POINT('Ctrl Pts',(-1.6002112841401,13.4100000211329,-7.99166780560954));
#45705=CARTESIAN_POINT('Ctrl Pts',(-1.59999999919616,13.4100000315449,-7.99166557366517));
#45706=CARTESIAN_POINT('Origin',(-1.59956987618261,12.9080292250358,-7.99148759263989));
#45707=CARTESIAN_POINT('Origin',(-1.655461430999,12.91,-7.991668980196));
#45708=CARTESIAN_POINT('',(-1.601056615238,13.40972231748,-8.00833023518));
#45709=CARTESIAN_POINT('',(2.2378444969905,13.41,-7.99166898016762));
#45710=CARTESIAN_POINT('',(-1.599999999195,13.41000000789,-7.991665573665));
#45711=CARTESIAN_POINT('Origin',(2.23784449531,12.91,-7.991668980205));
#45712=CARTESIAN_POINT('Origin',(-4.6,13.14,-16.1));
#45713=CARTESIAN_POINT('Ctrl Pts',(2.237584879956,13.40969719968,-8.009067185702));
#45714=CARTESIAN_POINT('Ctrl Pts',(2.237671468845,13.40969719968,-8.009067401558));
#45715=CARTESIAN_POINT('Ctrl Pts',(2.239198787813,13.40969719969,-8.009069273182));
#45716=CARTESIAN_POINT('Ctrl Pts',(2.24216509334,13.40969719965,-8.009006600652));
#45717=CARTESIAN_POINT('Ctrl Pts',(2.246462362136,13.40969719977,-8.008735050859));
#45718=CARTESIAN_POINT('Ctrl Pts',(2.24940692538,13.40969719947,-8.008431649983));
#45719=CARTESIAN_POINT('Ctrl Pts',(2.250913040081,13.40969719947,-8.0082427628));
#45720=CARTESIAN_POINT('Ctrl Pts',(2.251000426241,13.40969719947,-8.008231688651));
#45721=CARTESIAN_POINT('Ctrl Pts',(2.23759991999,13.40990301476,-8.003156059809));
#45722=CARTESIAN_POINT('Ctrl Pts',(2.237681494666,13.40990301476,-8.003156262383));
#45723=CARTESIAN_POINT('Ctrl Pts',(2.239120381434,13.40990301476,-8.003158014987));
#45724=CARTESIAN_POINT('Ctrl Pts',(2.241915466341,13.40990301475,-8.003099040079));
#45725=CARTESIAN_POINT('Ctrl Pts',(2.245971217721,13.40990301479,-8.002842672911));
#45726=CARTESIAN_POINT('Ctrl Pts',(2.248749025408,13.40990301469,-8.002556661255));
#45727=CARTESIAN_POINT('Ctrl Pts',(2.250172844306,13.40990301469,-8.002378138397));
#45728=CARTESIAN_POINT('Ctrl Pts',(2.250255466462,13.40990301469,-8.002367670494));
#45729=CARTESIAN_POINT('Ctrl Pts',(2.237614966948,13.41000391998,-7.997242212746));
#45730=CARTESIAN_POINT('Ctrl Pts',(2.237691525102,13.41000391998,-7.997242402031));
#45731=CARTESIAN_POINT('Ctrl Pts',(2.239041938962,13.41000391998,-7.99724403556));
#45732=CARTESIAN_POINT('Ctrl Pts',(2.241665724427,13.41000391998,-7.997188759977));
#45733=CARTESIAN_POINT('Ctrl Pts',(2.245479847208,13.41000391997,-7.996947582423));
#45734=CARTESIAN_POINT('Ctrl Pts',(2.248090822574,13.41000391998,-7.996678967993));
#45735=CARTESIAN_POINT('Ctrl Pts',(2.249432307784,13.41000391998,-7.996510814231));
#45736=CARTESIAN_POINT('Ctrl Pts',(2.249510163744,13.41000391998,-7.996500952852));
#45737=CARTESIAN_POINT('Ctrl Pts',(2.237630016093,13.40999988357,-7.991327506279));
#45738=CARTESIAN_POINT('Ctrl Pts',(2.237701556996,13.40999988357,-7.991327682274));
#45739=CARTESIAN_POINT('Ctrl Pts',(2.238963485089,13.40999988357,-7.991329196711));
#45740=CARTESIAN_POINT('Ctrl Pts',(2.24141594622,13.40999988357,-7.991277620989));
#45741=CARTESIAN_POINT('Ctrl Pts',(2.24498840529,13.40999988357,-7.991051635257));
#45742=CARTESIAN_POINT('Ctrl Pts',(2.247432524089,13.40999988357,-7.990800420582));
#45743=CARTESIAN_POINT('Ctrl Pts',(2.248691663647,13.40999988357,-7.990642637421));
#45744=CARTESIAN_POINT('Ctrl Pts',(2.248764752717,13.40999988357,-7.990633382656));
#45745=CARTESIAN_POINT('',(2.24859000193236,13.4099999999984,-7.99099916821552));
#45746=CARTESIAN_POINT('Origin',(2.24555455540351,13.4100000000148,-7.97888459757615));
#45747=CARTESIAN_POINT('Origin',(2.248590003289,12.90999965096,-7.990999166063));
#45748=CARTESIAN_POINT('Ctrl Pts',(2.278075340984,13.15718819574,-8.425336826683));
#45749=CARTESIAN_POINT('Ctrl Pts',(2.286140753447,13.15718819272,-8.424319735027));
#45750=CARTESIAN_POINT('Ctrl Pts',(2.35388291064,13.15718818874,-8.415807036881));
#45751=CARTESIAN_POINT('Ctrl Pts',(2.483820341006,13.15718844103,-8.399846720424));
#45752=CARTESIAN_POINT('Ctrl Pts',(2.655713713522,13.15718835356,-8.378231657577));
#45753=CARTESIAN_POINT('Ctrl Pts',(2.814178657447,13.15718837421,-8.358041618531));
#45754=CARTESIAN_POINT('Ctrl Pts',(2.958673491815,13.15718836941,-8.339207395949));
#45755=CARTESIAN_POINT('Ctrl Pts',(3.089582223425,13.15718837051,-8.321679161787));
#45756=CARTESIAN_POINT('Ctrl Pts',(3.208956769851,13.15718837026,-8.305254092409));
#45757=CARTESIAN_POINT('Ctrl Pts',(3.320120581901,13.15718837032,-8.289476173224));
#45758=CARTESIAN_POINT('Ctrl Pts',(3.426484163409,13.1571883703,-8.273855324399));
#45759=CARTESIAN_POINT('Ctrl Pts',(3.530967273143,13.15718837031,-8.257942363676));
#45760=CARTESIAN_POINT('Ctrl Pts',(3.635235631839,13.15718837031,-8.24140149434));
#45761=CARTESIAN_POINT('Ctrl Pts',(3.740376492139,13.15718837031,-8.223909889447));
#45762=CARTESIAN_POINT('Ctrl Pts',(3.848559055294,13.1571883703,-8.204917648829));
#45763=CARTESIAN_POINT('Ctrl Pts',(3.963755801124,13.15718837033,-8.183374059621));
#45764=CARTESIAN_POINT('Ctrl Pts',(4.05254074859,13.15718837025,-8.165401404086));
#45765=CARTESIAN_POINT('Ctrl Pts',(4.103430937961,13.15718837026,-8.154442560125));
#45766=CARTESIAN_POINT('Ctrl Pts',(4.112378765212,13.15718837026,-8.152494402827));
#45767=CARTESIAN_POINT('Ctrl Pts',(2.265371289856,13.33424242924,-8.325443171538));
#45768=CARTESIAN_POINT('Ctrl Pts',(2.273525484251,13.33424242834,-8.324414990892));
#45769=CARTESIAN_POINT('Ctrl Pts',(2.341879625082,13.33424242715,-8.315825860922));
#45770=CARTESIAN_POINT('Ctrl Pts',(2.471265663326,13.33424250275,-8.299934497874));
#45771=CARTESIAN_POINT('Ctrl Pts',(2.643103570828,13.33424247653,-8.278326401));
#45772=CARTESIAN_POINT('Ctrl Pts',(2.801329586393,13.33424248272,-8.258166691294));
#45773=CARTESIAN_POINT('Ctrl Pts',(2.945496865447,13.33424248129,-8.239375100594));
#45774=CARTESIAN_POINT('Ctrl Pts',(3.076049794216,13.33424248162,-8.221894455168));
#45775=CARTESIAN_POINT('Ctrl Pts',(3.195038588614,13.33424248154,-8.20552238341));
#45776=CARTESIAN_POINT('Ctrl Pts',(3.305742731698,13.33424248156,-8.189809589949));
#45777=CARTESIAN_POINT('Ctrl Pts',(3.411596899129,13.33424248155,-8.174263494606));
#45778=CARTESIAN_POINT('Ctrl Pts',(3.51551924109,13.33424248155,-8.158435800941));
#45779=CARTESIAN_POINT('Ctrl Pts',(3.619104977514,13.33424248155,-8.142002990221));
#45780=CARTESIAN_POINT('Ctrl Pts',(3.723429040626,13.33424248155,-8.124647006269));
#45781=CARTESIAN_POINT('Ctrl Pts',(3.830626058125,13.33424248155,-8.105827356883));
#45782=CARTESIAN_POINT('Ctrl Pts',(3.944552759001,13.33424248156,-8.08452044384));
#45783=CARTESIAN_POINT('Ctrl Pts',(4.032102539776,13.33424248154,-8.066796360282));
#45784=CARTESIAN_POINT('Ctrl Pts',(4.082151021483,13.33424248154,-8.056018666363));
#45785=CARTESIAN_POINT('Ctrl Pts',(4.09094646625,13.33424248154,-8.054103647986));
#45786=CARTESIAN_POINT('Ctrl Pts',(2.242543304394,13.42776922549,-8.145943665092));
#45787=CARTESIAN_POINT('Ctrl Pts',(2.250857031574,13.4277692257,-8.144895558574));
#45788=CARTESIAN_POINT('Ctrl Pts',(2.320310849465,13.42776922598,-8.136169087801));
#45789=CARTESIAN_POINT('Ctrl Pts',(2.448706087905,13.42776920825,-8.120401627548));
#45790=CARTESIAN_POINT('Ctrl Pts',(2.620444329994,13.4277692144,-8.098806047871));
#45791=CARTESIAN_POINT('Ctrl Pts',(2.778241013758,13.42776921295,-8.078700837139));
#45792=CARTESIAN_POINT('Ctrl Pts',(2.921819706712,13.42776921328,-8.059985851922));
#45793=CARTESIAN_POINT('Ctrl Pts',(3.051733291228,13.42776921321,-8.042590718981));
#45794=CARTESIAN_POINT('Ctrl Pts',(3.170028925497,13.42776921323,-8.026313878963));
#45795=CARTESIAN_POINT('Ctrl Pts',(3.279907086667,13.42776921322,-8.010718110303));
#45796=CARTESIAN_POINT('Ctrl Pts',(3.384845884895,13.42776921322,-7.995306339941));
#45797=CARTESIAN_POINT('Ctrl Pts',(3.487760579892,13.42776921322,-7.979631863162));
#45798=CARTESIAN_POINT('Ctrl Pts',(3.590119708273,13.42776921322,-7.963393223616));
#45799=CARTESIAN_POINT('Ctrl Pts',(3.692976063632,13.42776921322,-7.946280937741));
#45800=CARTESIAN_POINT('Ctrl Pts',(3.798402148244,13.42776921322,-7.927771418573));
#45801=CARTESIAN_POINT('Ctrl Pts',(3.910046697746,13.42776921322,-7.906889790346));
#45802=CARTESIAN_POINT('Ctrl Pts',(3.995377000107,13.42776921323,-7.889612367263));
#45803=CARTESIAN_POINT('Ctrl Pts',(4.043913012279,13.42776921323,-7.879160182937));
#45804=CARTESIAN_POINT('Ctrl Pts',(4.052434640046,13.42776921323,-7.877304712087));
#45805=CARTESIAN_POINT('Ctrl Pts',(2.216973445714,13.40752410553,-7.94488444239));
#45806=CARTESIAN_POINT('Ctrl Pts',(2.225465867189,13.4075241055,-7.9438140167));
#45807=CARTESIAN_POINT('Ctrl Pts',(2.296151444539,13.40752410546,-7.934933709098));
#45808=CARTESIAN_POINT('Ctrl Pts',(2.423436878043,13.40752410793,-7.919305033624));
#45809=CARTESIAN_POINT('Ctrl Pts',(2.595063483889,13.40752410708,-7.897723474586));
#45810=CARTESIAN_POINT('Ctrl Pts',(2.752379268737,13.40752410728,-7.87767930871));
#45811=CARTESIAN_POINT('Ctrl Pts',(2.895298680413,13.40752410723,-7.859050130073));
#45812=CARTESIAN_POINT('Ctrl Pts',(3.024496128928,13.40752410724,-7.841750780536));
#45813=CARTESIAN_POINT('Ctrl Pts',(3.142015347489,13.40752410724,-7.82558061056));
#45814=CARTESIAN_POINT('Ctrl Pts',(3.250968317917,13.40752410724,-7.810115922569));
#45815=CARTESIAN_POINT('Ctrl Pts',(3.354881801791,13.40752410724,-7.794854610983));
#45816=CARTESIAN_POINT('Ctrl Pts',(3.456667821175,13.40752410724,-7.779351753998));
#45817=CARTESIAN_POINT('Ctrl Pts',(3.557653013413,13.40752410724,-7.763330607559));
#45818=CARTESIAN_POINT('Ctrl Pts',(3.65886537439,13.40752410724,-7.746491290379));
#45819=CARTESIAN_POINT('Ctrl Pts',(3.762307819065,13.40752410724,-7.728329151223));
#45820=CARTESIAN_POINT('Ctrl Pts',(3.871396107604,13.40752410724,-7.707923888843));
#45821=CARTESIAN_POINT('Ctrl Pts',(3.954240349621,13.40752410724,-7.6911467747));
#45822=CARTESIAN_POINT('Ctrl Pts',(4.001082229283,13.40752410724,-7.68105919698));
#45823=CARTESIAN_POINT('Ctrl Pts',(4.009297151845,13.40752410724,-7.679270425919));
#45824=CARTESIAN_POINT('Ctrl Pts',(2.25070093407567,13.4097088394601,-8.00792902136249));
#45825=CARTESIAN_POINT('Ctrl Pts',(2.25070142686699,13.4097088356214,-8.00792907293275));
#45826=CARTESIAN_POINT('Ctrl Pts',(2.25070191965817,13.4097088317827,-8.007929124503));
#45827=CARTESIAN_POINT('Ctrl Pts',(2.25070241244921,13.4097088279439,-8.00792917607324));
#45828=CARTESIAN_POINT('Ctrl Pts',(2.27794362486571,13.4094966216791,-8.01077995025102));
#45829=CARTESIAN_POINT('Ctrl Pts',(2.30476118430153,13.4091718850223,-8.01360907290453));
#45830=CARTESIAN_POINT('Ctrl Pts',(2.33118325787516,13.4087450676421,-8.0163942422403));
#45831=CARTESIAN_POINT('Ctrl Pts',(2.35999938229403,13.408279577199,-8.01943177015739));
#45832=CARTESIAN_POINT('Ctrl Pts',(2.38834468584762,13.4076926978792,-8.02241701648861));
#45833=CARTESIAN_POINT('Ctrl Pts',(2.41619478593185,13.4069965329008,-8.02533510968307));
#45834=CARTESIAN_POINT('Ctrl Pts',(2.42477884851803,13.406781958313,-8.02623453534179));
#45835=CARTESIAN_POINT('Ctrl Pts',(2.43331548901635,13.4065569900252,-8.02712767440583));
#45836=CARTESIAN_POINT('Ctrl Pts',(2.44180307769693,13.4063219516077,-8.02801432599494));
#45837=CARTESIAN_POINT('Ctrl Pts',(2.48538791449942,13.4051149997328,-8.03256739357004));
#45838=CARTESIAN_POINT('Ctrl Pts',(2.52773990785003,13.4036436248157,-8.03693549898386));
#45839=CARTESIAN_POINT('Ctrl Pts',(2.56891103034342,13.4019523661277,-8.04113042432577));
#45840=CARTESIAN_POINT('Ctrl Pts',(2.58562190995613,13.4012659039033,-8.04283309571599));
#45841=CARTESIAN_POINT('Ctrl Pts',(2.60213891571461,13.4005431591336,-8.04450719695673));
#45842=CARTESIAN_POINT('Ctrl Pts',(2.61846777138499,13.3997868594101,-8.04615339980819));
#45843=CARTESIAN_POINT('Ctrl Pts',(2.67502654508264,13.397167240144,-8.05185540467708));
#45844=CARTESIAN_POINT('Ctrl Pts',(2.7293135332922,13.3941445132716,-8.05722302128092));
#45845=CARTESIAN_POINT('Ctrl Pts',(2.78107106661417,13.3908432614605,-8.06222510384196));
#45846=CARTESIAN_POINT('Ctrl Pts',(2.83282859993615,13.3875420096493,-8.06722718640301));
#45847=CARTESIAN_POINT('Ctrl Pts',(2.88205673194293,13.3839633579127,-8.07186414347928));
#45848=CARTESIAN_POINT('Ctrl Pts',(2.92878849763644,13.380217612112,-8.07613720207639));
#45849=CARTESIAN_POINT('Ctrl Pts',(2.97552026332994,13.3764718663113,-8.0804102606735));
#45850=CARTESIAN_POINT('Ctrl Pts',(3.01975576917847,13.372561337648,-8.0843202277642));
#45851=CARTESIAN_POINT('Ctrl Pts',(3.06193261059204,13.3685399555076,-8.08792588768494));
#45852=CARTESIAN_POINT('Ctrl Pts',(3.10410945200556,13.3645185733671,-8.09153154760569));
#45853=CARTESIAN_POINT('Ctrl Pts',(3.14422766443156,13.3603870338277,-8.09483316581655));
#45854=CARTESIAN_POINT('Ctrl Pts',(3.18291144942371,13.3561410864198,-8.09789654337337));
#45855=CARTESIAN_POINT('Ctrl Pts',(3.22159523441592,13.3518951390118,-8.1009599209302));
#45856=CARTESIAN_POINT('Ctrl Pts',(3.25884458823385,13.3475347577083,-8.10378503371712));
#45857=CARTESIAN_POINT('Ctrl Pts',(3.29532012225226,13.3430188597012,-8.10641940803316));
#45858=CARTESIAN_POINT('Ctrl Pts',(3.33179565627067,13.3385029616941,-8.10905378234921));
#45859=CARTESIAN_POINT('Ctrl Pts',(3.36749736453129,13.3338314262824,-8.11149737027822));
#45860=CARTESIAN_POINT('Ctrl Pts',(3.40302221319701,13.3289360949713,-8.11378048183653));
#45861=CARTESIAN_POINT('Ctrl Pts',(3.43854706186268,13.3240407636603,-8.11606359339485));
#45862=CARTESIAN_POINT('Ctrl Pts',(3.47389500089121,13.3189213316682,-8.11818593114135));
#45863=CARTESIAN_POINT('Ctrl Pts',(3.50947489449939,13.3134962224709,-8.12015680508066));
#45864=CARTESIAN_POINT('Ctrl Pts',(3.54505478810762,13.3080711132736,-8.12212767901997));
#45865=CARTESIAN_POINT('Ctrl Pts',(3.58086623287029,13.3023365335503,-8.12394444876931));
#45866=CARTESIAN_POINT('Ctrl Pts',(3.61654311190259,13.2963278639491,-8.12555585329945));
#45867=CARTESIAN_POINT('Ctrl Pts',(3.65221999093489,13.2903191943479,-8.12716725782958));
#45868=CARTESIAN_POINT('Ctrl Pts',(3.68776288736539,13.2840406765724,-8.12857684740129));
#45869=CARTESIAN_POINT('Ctrl Pts',(3.72363861368408,13.2773820882215,-8.12976222303873));
#45870=CARTESIAN_POINT('Ctrl Pts',(3.75236529817654,13.2720503727039,-8.13071138603656));
#45871=CARTESIAN_POINT('Ctrl Pts',(3.78130602030519,13.2664765012613,-8.13151659935786));
#45872=CARTESIAN_POINT('Ctrl Pts',(3.81091149710654,13.2605331055368,-8.13215612642615));
#45873=CARTESIAN_POINT('Ctrl Pts',(3.81827923883093,13.2590540074308,-8.13231528178435));
#45874=CARTESIAN_POINT('Ctrl Pts',(3.82568817679555,13.2575519470327,-8.13246394080603));
#45875=CARTESIAN_POINT('Ctrl Pts',(3.83314531426046,13.2560248155579,-8.13260127222032));
#45876=CARTESIAN_POINT('Ctrl Pts',(3.85778472246543,13.2509789630487,-8.13305503410844));
#45877=CARTESIAN_POINT('Ctrl Pts',(3.88295097129545,13.2456623141355,-8.13338659784483));
#45878=CARTESIAN_POINT('Ctrl Pts',(3.90899354542653,13.2399434928449,-8.13356657373334));
#45879=CARTESIAN_POINT('Ctrl Pts',(3.92250390029888,13.2369766853128,-8.13365994154369));
#45880=CARTESIAN_POINT('Ctrl Pts',(3.93625018293504,13.2339014430577,-8.13371178145361));
#45881=CARTESIAN_POINT('Ctrl Pts',(3.95028185158443,13.2306982824754,-8.13371247872827));
#45882=CARTESIAN_POINT('Ctrl Pts',(3.98739045364131,13.2222271010112,-8.13371432276327));
#45883=CARTESIAN_POINT('Ctrl Pts',(4.02649097892153,13.212856018128,-8.13336322175475));
#45884=CARTESIAN_POINT('Ctrl Pts',(4.06694679202954,13.202515578365,-8.13245141709027));
#45885=CARTESIAN_POINT('Ctrl Pts',(4.07127546077212,13.2014091777035,-8.13235385631848));
#45886=CARTESIAN_POINT('Ctrl Pts',(4.07561965073057,13.2002917055087,-8.13224983579308));
#45887=CARTESIAN_POINT('Ctrl Pts',(4.07997858462006,13.1991630971381,-8.13213907538709));
#45888=CARTESIAN_POINT('',(3.99496190950109,13.4099999999998,-7.73319438214748));
#45889=CARTESIAN_POINT('Ctrl Pts',(2.24859000168769,13.4099999999975,-7.99099916626274));
#45890=CARTESIAN_POINT('Ctrl Pts',(2.30138639266896,13.409999999997,-7.98438415500106));
#45891=CARTESIAN_POINT('Ctrl Pts',(2.35261444485792,13.4099999999934,-7.97807171786754));
#45892=CARTESIAN_POINT('Ctrl Pts',(2.40222264371354,13.4099999999962,-7.97192548958838));
#45893=CARTESIAN_POINT('Ctrl Pts',(2.41299850134135,13.4099999999968,-7.9705904102585));
#45894=CARTESIAN_POINT('Ctrl Pts',(2.42369792263813,13.4099999999977,-7.96926336922857));
#45895=CARTESIAN_POINT('Ctrl Pts',(2.43432037163303,13.4099999999979,-7.96794328908766));
#45896=CARTESIAN_POINT('Ctrl Pts',(2.493845504109,13.4099999999988,-7.96054594170533));
#45897=CARTESIAN_POINT('Ctrl Pts',(2.55095381197397,13.4100000000006,-7.95335804203067));
#45898=CARTESIAN_POINT('Ctrl Pts',(2.60584016881678,13.4100000000012,-7.94640684095368));
#45899=CARTESIAN_POINT('Ctrl Pts',(2.66072652565963,13.4100000000018,-7.93945563987667));
#45900=CARTESIAN_POINT('Ctrl Pts',(2.71339093148032,13.4100000000012,-7.93274113739734));
#45901=CARTESIAN_POINT('Ctrl Pts',(2.76354134874866,13.4100000000003,-7.92627486699083));
#45902=CARTESIAN_POINT('Ctrl Pts',(2.813691766017,13.4099999999995,-7.91980859658434));
#45903=CARTESIAN_POINT('Ctrl Pts',(2.861328194733,13.4099999999983,-7.91359055825067));
#45904=CARTESIAN_POINT('Ctrl Pts',(2.90650757886068,13.4099999999979,-7.90761729845183));
#45905=CARTESIAN_POINT('Ctrl Pts',(2.95168696298835,13.4099999999975,-7.901644038653));
#45906=CARTESIAN_POINT('Ctrl Pts',(2.99440930252771,13.4099999999978,-7.895915557389));
#45907=CARTESIAN_POINT('Ctrl Pts',(3.03509758705189,13.4099999999984,-7.89038857294066));
#45908=CARTESIAN_POINT('Ctrl Pts',(3.07578587157602,13.4099999999989,-7.88486158849233));
#45909=CARTESIAN_POINT('Ctrl Pts',(3.11444010108498,13.4099999999997,-7.87953610085967));
#45910=CARTESIAN_POINT('Ctrl Pts',(3.15164810591261,13.4099999999997,-7.87433282904934));
#45911=CARTESIAN_POINT('Ctrl Pts',(3.1888561107403,13.4099999999998,-7.869129557239));
#45912=CARTESIAN_POINT('Ctrl Pts',(3.22461789088665,13.4099999999993,-7.864048501251));
#45913=CARTESIAN_POINT('Ctrl Pts',(3.25957932564517,13.409999999999,-7.85899818299083));
#45914=CARTESIAN_POINT('Ctrl Pts',(3.29454076040368,13.4099999999987,-7.85394786473066));
#45915=CARTESIAN_POINT('Ctrl Pts',(3.32870184977437,13.4099999999986,-7.84892828419833));
#45916=CARTESIAN_POINT('Ctrl Pts',(3.36263775530638,13.4099999999986,-7.84385152101549));
#45917=CARTESIAN_POINT('Ctrl Pts',(3.39657366083835,13.4099999999986,-7.83877475783267));
#45918=CARTESIAN_POINT('Ctrl Pts',(3.43028438253165,13.4099999999986,-7.83364081199933));
#45919=CARTESIAN_POINT('Ctrl Pts',(3.46411762057695,13.4099999999986,-7.82838032187151));
#45920=CARTESIAN_POINT('Ctrl Pts',(3.4979508586223,13.4099999999986,-7.82311983174367));
#45921=CARTESIAN_POINT('Ctrl Pts',(3.53190661301965,13.4099999999986,-7.81773279732134));
#45922=CARTESIAN_POINT('Ctrl Pts',(3.56562768693499,13.4099999999986,-7.81225344182417));
#45923=CARTESIAN_POINT('Ctrl Pts',(3.59934876085033,13.4099999999986,-7.806774086327));
#45924=CARTESIAN_POINT('Ctrl Pts',(3.63283515428367,13.4099999999986,-7.801202409755));
#45925=CARTESIAN_POINT('Ctrl Pts',(3.66649691169818,13.4099999999986,-7.79544915546967));
#45926=CARTESIAN_POINT('Ctrl Pts',(3.70015866911268,13.4099999999986,-7.78969590118433));
#45927=CARTESIAN_POINT('Ctrl Pts',(3.73399579050837,13.4099999999986,-7.78376106918566));
#45928=CARTESIAN_POINT('Ctrl Pts',(3.76882549197522,13.4099999999986,-7.77745371488882));
#45929=CARTESIAN_POINT('Ctrl Pts',(3.79950885807498,13.4099999999986,-7.77189722566095));
#45930=CARTESIAN_POINT('Ctrl Pts',(3.83096170362461,13.4099999999984,-7.76605064457506));
#45931=CARTESIAN_POINT('Ctrl Pts',(3.86372916609635,13.4099999999989,-7.75974007885942));
#45932=CARTESIAN_POINT('Ctrl Pts',(3.86815713166221,13.409999999999,-7.75888731317107));
#45933=CARTESIAN_POINT('Ctrl Pts',(3.87260905245847,13.409999999999,-7.75802601485461));
#45934=CARTESIAN_POINT('Ctrl Pts',(3.8770862219782,13.4099999999991,-7.75715569492626));
#45935=CARTESIAN_POINT('Ctrl Pts',(3.91190350686239,13.4099999999994,-7.75038754001229));
#45936=CARTESIAN_POINT('Ctrl Pts',(3.94825130413398,13.4100000000001,-7.7430782376179));
#45937=CARTESIAN_POINT('Ctrl Pts',(3.98588409196118,13.4100000000003,-7.73512119656737));
#45938=CARTESIAN_POINT('Ctrl Pts',(3.98890128591575,13.4100000000003,-7.73448324393244));
#45939=CARTESIAN_POINT('Ctrl Pts',(3.99192671687108,13.4100000000003,-7.73384111172618));
#45940=CARTESIAN_POINT('Ctrl Pts',(3.99496024621,13.4100000000004,-7.733194736626));
#45941=CARTESIAN_POINT('Origin',(3.994963573291,12.9099999999,-7.733194027536));
#45942=CARTESIAN_POINT('Ctrl Pts',(3.739203750449,12.9180458811,-8.891362475312));
#45943=CARTESIAN_POINT('Ctrl Pts',(3.73146660992,12.92315978193,-8.889112682545));
#45944=CARTESIAN_POINT('Ctrl Pts',(3.643055660205,12.98106721331,-8.862733317068));
#45945=CARTESIAN_POINT('Ctrl Pts',(3.462068739991,13.08744838347,-8.79359290624));
#45946=CARTESIAN_POINT('Ctrl Pts',(3.185389292547,13.21644881828,-8.656430471233));
#45947=CARTESIAN_POINT('Ctrl Pts',(2.87990332086,13.32045340503,-8.478983152178));
#45948=CARTESIAN_POINT('Ctrl Pts',(2.552976861821,13.38969339755,-8.270214273238));
#45949=CARTESIAN_POINT('Ctrl Pts',(2.32535497479,13.40826165724,-8.117787218622));
#45950=CARTESIAN_POINT('Ctrl Pts',(2.20750057804,13.40989482807,-8.038538555201));
#45951=CARTESIAN_POINT('Ctrl Pts',(2.203441286853,13.40994161843,-8.03580865607));
#45952=CARTESIAN_POINT('Ctrl Pts',(3.803158684465,12.89472761344,-8.566360772745));
#45953=CARTESIAN_POINT('Ctrl Pts',(3.796388461278,12.89934439347,-8.564337486772));
#45954=CARTESIAN_POINT('Ctrl Pts',(3.718914974065,12.95177154022,-8.540571264521));
#45955=CARTESIAN_POINT('Ctrl Pts',(3.55770110028,13.05139891642,-8.477273832003));
#45956=CARTESIAN_POINT('Ctrl Pts',(3.304530173815,13.17905954386,-8.348467736982));
#45957=CARTESIAN_POINT('Ctrl Pts',(3.017846351306,13.2886957054,-8.178410744612));
#45958=CARTESIAN_POINT('Ctrl Pts',(2.703644178881,13.36890354346,-7.974894308892));
#45959=CARTESIAN_POINT('Ctrl Pts',(2.479858161105,13.39690127167,-7.824049236676));
#45960=CARTESIAN_POINT('Ctrl Pts',(2.362668879712,13.40348799783,-7.745039942689));
#45961=CARTESIAN_POINT('Ctrl Pts',(2.358630951334,13.40370547786,-7.742317582132));
#45962=CARTESIAN_POINT('Ctrl Pts',(3.942747596141,13.00246573178,-8.284993708305));
#45963=CARTESIAN_POINT('Ctrl Pts',(3.9364609035,13.00688490927,-8.283135183149));
#45964=CARTESIAN_POINT('Ctrl Pts',(3.864406309965,13.05720985831,-8.261272807038));
#45965=CARTESIAN_POINT('Ctrl Pts',(3.711790014713,13.15598759483,-8.202287599445));
#45966=CARTESIAN_POINT('Ctrl Pts',(3.465401337309,13.28883036506,-8.079461983691));
#45967=CARTESIAN_POINT('Ctrl Pts',(3.17947995917,13.40871254137,-7.914244697299));
#45968=CARTESIAN_POINT('Ctrl Pts',(2.859189437579,13.50224374698,-7.71339622914));
#45969=CARTESIAN_POINT('Ctrl Pts',(2.626512259222,13.53963961786,-7.562459200681));
#45970=CARTESIAN_POINT('Ctrl Pts',(2.503505827146,13.55074997021,-7.482859510525));
#45971=CARTESIAN_POINT('Ctrl Pts',(2.499266117154,13.55112284234,-7.48011615425));
#45972=CARTESIAN_POINT('Ctrl Pts',(4.126573294533,13.21702712022,-8.110548081366));
#45973=CARTESIAN_POINT('Ctrl Pts',(4.120177986995,13.22159265941,-8.10875551204));
#45974=CARTESIAN_POINT('Ctrl Pts',(4.046804867636,13.27366633679,-8.087659460274));
#45975=CARTESIAN_POINT('Ctrl Pts',(3.889676863125,13.37768969408,-8.030485792242));
#45976=CARTESIAN_POINT('Ctrl Pts',(3.631818657962,13.52107095805,-7.909919629098));
#45977=CARTESIAN_POINT('Ctrl Pts',(3.32844852574,13.65350899285,-7.745902851738));
#45978=CARTESIAN_POINT('Ctrl Pts',(2.984626447899,13.75972231478,-7.544537779912));
#45979=CARTESIAN_POINT('Ctrl Pts',(2.73233093329,13.80437111482,-7.391855539927));
#45980=CARTESIAN_POINT('Ctrl Pts',(2.598333513568,13.81855768255,-7.310968483515));
#45981=CARTESIAN_POINT('Ctrl Pts',(2.593714263493,13.81903569747,-7.308180319716));
#45982=CARTESIAN_POINT('Ctrl Pts',(4.049148071614,13.05937723215,-8.208772713831));
#45983=CARTESIAN_POINT('Ctrl Pts',(4.064894678394,13.05937723208,-8.205946355611));
#45984=CARTESIAN_POINT('Ctrl Pts',(4.100886611793,13.05937723204,-8.198815606686));
#45985=CARTESIAN_POINT('Ctrl Pts',(4.153076125832,13.05937723217,-8.186493455414));
#45986=CARTESIAN_POINT('Ctrl Pts',(4.208582748717,13.05937723213,-8.171878615881));
#45987=CARTESIAN_POINT('Ctrl Pts',(4.264585919179,13.05937723214,-8.156133113951));
#45988=CARTESIAN_POINT('Ctrl Pts',(4.323333002791,13.05937723213,-8.139058904706));
#45989=CARTESIAN_POINT('Ctrl Pts',(4.372134051461,13.05937723214,-8.124730690516));
#45990=CARTESIAN_POINT('Ctrl Pts',(4.40143305218,13.05937723213,-8.116204585805));
#45991=CARTESIAN_POINT('Ctrl Pts',(4.410246257208,13.05937723213,-8.113652741193));
#45992=CARTESIAN_POINT('Ctrl Pts',(4.036444039793,13.29564346116,-8.135894285009));
#45993=CARTESIAN_POINT('Ctrl Pts',(4.051118792472,13.29564346114,-8.133268259165));
#45994=CARTESIAN_POINT('Ctrl Pts',(4.084982381981,13.29564346112,-8.126565695879));
#45995=CARTESIAN_POINT('Ctrl Pts',(4.135046057456,13.29564346117,-8.114753411066));
#45996=CARTESIAN_POINT('Ctrl Pts',(4.189047146895,13.29564346115,-8.100538275903));
#45997=CARTESIAN_POINT('Ctrl Pts',(4.24416519593,13.29564346116,-8.085043648133));
#45998=CARTESIAN_POINT('Ctrl Pts',(4.302523744979,13.29564346116,-8.068083020918));
#45999=CARTESIAN_POINT('Ctrl Pts',(4.351341025745,13.29564346116,-8.053750009283));
#46000=CARTESIAN_POINT('Ctrl Pts',(4.380795426626,13.29564346116,-8.045178569442));
#46001=CARTESIAN_POINT('Ctrl Pts',(4.389668354159,13.29564346116,-8.042609311642));
#46002=CARTESIAN_POINT('Ctrl Pts',(4.000966626673,13.43213122111,-7.9323732168));
#46003=CARTESIAN_POINT('Ctrl Pts',(4.012648108297,13.43213122111,-7.930306641258));
#46004=CARTESIAN_POINT('Ctrl Pts',(4.040568062233,13.43213122111,-7.9247998337));
#46005=CARTESIAN_POINT('Ctrl Pts',(4.084695098534,13.4321312211,-7.914411407335));
#46006=CARTESIAN_POINT('Ctrl Pts',(4.134491819411,13.43213122111,-7.901312490802));
#46007=CARTESIAN_POINT('Ctrl Pts',(4.187138069023,13.43213122111,-7.886518456859));
#46008=CARTESIAN_POINT('Ctrl Pts',(4.244411592357,13.43213122111,-7.869875020014));
#46009=CARTESIAN_POINT('Ctrl Pts',(4.293274203046,13.43213122111,-7.855528610986));
#46010=CARTESIAN_POINT('Ctrl Pts',(4.323162576058,13.43213122111,-7.846830567784));
#46011=CARTESIAN_POINT('Ctrl Pts',(4.332202285286,13.43213122111,-7.844212681733));
#46012=CARTESIAN_POINT('Ctrl Pts',(3.958653872581,13.40752410724,-7.689640273377));
#46013=CARTESIAN_POINT('Ctrl Pts',(3.966765377397,13.40752410724,-7.688240935973));
#46014=CARTESIAN_POINT('Ctrl Pts',(3.987596550943,13.40752410724,-7.684160267291));
#46015=CARTESIAN_POINT('Ctrl Pts',(4.024643151232,13.40752410724,-7.67547003048));
#46016=CARTESIAN_POINT('Ctrl Pts',(4.069425458784,13.40752410724,-7.663702391521));
#46017=CARTESIAN_POINT('Ctrl Pts',(4.119123673802,13.40752410724,-7.649743932995));
#46018=CARTESIAN_POINT('Ctrl Pts',(4.175103122337,13.40752410724,-7.633478798764));
#46019=CARTESIAN_POINT('Ctrl Pts',(4.224019796546,13.40752410724,-7.619116411102));
#46020=CARTESIAN_POINT('Ctrl Pts',(4.254425753972,13.40752410724,-7.610267372199));
#46021=CARTESIAN_POINT('Ctrl Pts',(4.263664378291,13.40752410724,-7.607591488817));
#46022=CARTESIAN_POINT('Ctrl Pts',(3.99496190950166,13.41,-7.73319438213609));
#46023=CARTESIAN_POINT('Ctrl Pts',(4.00851215418661,13.41,-7.730306466485));
#46024=CARTESIAN_POINT('Ctrl Pts',(4.03662735941919,13.41,-7.72369650207739));
#46025=CARTESIAN_POINT('Ctrl Pts',(4.080565611154,13.41,-7.7121736621));
#46026=CARTESIAN_POINT('Ctrl Pts',(4.130494585122,13.41,-7.698184085465));
#46027=CARTESIAN_POINT('Ctrl Pts',(4.186228983442,13.41,-7.682004638378));
#46028=CARTESIAN_POINT('Ctrl Pts',(4.227999624963,13.41,-7.66974072988));
#46029=CARTESIAN_POINT('Ctrl Pts',(4.24999999921,13.41,-7.66332099539));
#46030=CARTESIAN_POINT('Origin',(-4.6,13.41,-8.));
#46031=CARTESIAN_POINT('',(-1.599999999708,13.41,7.5));
#46032=CARTESIAN_POINT('',(4.249999999336,13.41,7.5));
#46033=CARTESIAN_POINT('',(-1.599999999708,13.41,7.5));
#46034=CARTESIAN_POINT('Origin',(4.345740905029,12.91,7.5));
#46035=CARTESIAN_POINT('Origin',(-1.6,12.91,7.5));
#46036=CARTESIAN_POINT('Origin',(-1.6,10.41,7.5));
#46037=CARTESIAN_POINT('Origin',(-1.6,10.41,7.5));
#46038=CARTESIAN_POINT('Origin',(-4.1,10.41,7.5));
#46039=CARTESIAN_POINT('Origin',(-4.1,10.465461431,7.5));
#46040=CARTESIAN_POINT('Origin',(-4.1,1.41,7.5));
#46041=CARTESIAN_POINT('Origin',(-4.1,1.41,0.));
#46042=CARTESIAN_POINT('Origin',(-4.1,1.41,-7.5));
#46043=CARTESIAN_POINT('Origin',(-4.1,1.343139657048,-7.5));
#46044=CARTESIAN_POINT('Origin',(-1.6,10.41,39.41676));
#46045=CARTESIAN_POINT('Origin',(-4.1,-39.88672151809,-7.988586197742));
#46046=CARTESIAN_POINT('Origin',(4.75,1.348669871537,7.5));
#46047=CARTESIAN_POINT('',(0.,0.,0.));
#46048=CARTESIAN_POINT('Origin',(0.,0.,0.));
#46049=CARTESIAN_POINT('',(6.19994098326668,0.,0.0270518762789905));
#46050=CARTESIAN_POINT('Origin',(0.,0.,0.));
#46051=CARTESIAN_POINT('',(-4.,0.,4.89858719658941E-16));
#46052=CARTESIAN_POINT('Origin',(0.,0.,0.));
#46053=CARTESIAN_POINT('Origin',(0.,0.,0.));
#46054=CARTESIAN_POINT('',(-4.,1.6,4.89858719658941E-16));
#46055=CARTESIAN_POINT('',(-4.,0.,4.89858719658941E-16));
#46056=CARTESIAN_POINT('Origin',(0.,1.6,0.));
#46057=CARTESIAN_POINT('Origin',(0.,1.6,0.));
#46058=CARTESIAN_POINT('',(6.19994098326668,1.6,0.0270518762789905));
#46059=CARTESIAN_POINT('Origin',(0.,1.6,0.));
#46060=CARTESIAN_POINT('Origin',(0.,0.8,0.));
#46061=CARTESIAN_POINT('Origin',(6.19994098326668,0.8,0.0270518762789905));
#46062=CARTESIAN_POINT('',(0.,0.,0.));
#46063=CARTESIAN_POINT('Origin',(0.,0.,0.));
#46064=CARTESIAN_POINT('',(3.48003877702181,-0.646332386289707,7.2890636783777E-5));
#46065=CARTESIAN_POINT('',(3.47936545704605,-0.650670105535317,-4.76018332824096E-10));
#46066=CARTESIAN_POINT('Ctrl Pts',(3.4800387770396,-0.646332386169619,7.2890641512717E-5));
#46067=CARTESIAN_POINT('Ctrl Pts',(3.47981522939477,-0.647778405716227,
4.85936023357466E-5));
#46068=CARTESIAN_POINT('Ctrl Pts',(3.47959078938191,-0.649224312550689,
2.42965631587873E-5));
#46069=CARTESIAN_POINT('Ctrl Pts',(3.47936545704605,-0.650670105535317,
-4.76018183204197E-10));
#46070=CARTESIAN_POINT('',(-0.264621262814254,3.52921885147511,9.97465998686664E-17));
#46071=CARTESIAN_POINT('Ctrl Pts',(3.48016653829928,-0.646334509992552,
-5.89805981832114E-17));
#46072=CARTESIAN_POINT('Ctrl Pts',(3.49317607817561,-0.575677005108545,
-4.47285692339558E-17));
#46073=CARTESIAN_POINT('Ctrl Pts',(3.50395521937367,-0.50501662146249,-2.70647475776074E-16));
#46074=CARTESIAN_POINT('Ctrl Pts',(3.51259146904678,-0.434285235184753,
-9.71445146547012E-17));
#46075=CARTESIAN_POINT('Ctrl Pts',(3.52000759887453,-0.373546701285584,
5.18461391449629E-17));
#46076=CARTESIAN_POINT('Ctrl Pts',(3.5258427031227,-0.312755312469289,3.08838204074247E-17));
#46077=CARTESIAN_POINT('Ctrl Pts',(3.53012221027278,-0.251861352637095,
6.93889390390723E-18));
#46078=CARTESIAN_POINT('Ctrl Pts',(3.53326008626827,-0.207211889947475,
-1.06183171145701E-17));
#46079=CARTESIAN_POINT('Ctrl Pts',(3.53556105447104,-0.162507144984163,
-9.16607259699049E-18));
#46080=CARTESIAN_POINT('Ctrl Pts',(3.53702575001128,-0.11772666792086,-4.85722573273506E-17));
#46081=CARTESIAN_POINT('Ctrl Pts',(3.53979104880602,-0.0331825453716335,
-1.22969886149647E-16));
#46082=CARTESIAN_POINT('Ctrl Pts',(3.53956910994069,0.0516350306695476,
-6.18610164700975E-17));
#46083=CARTESIAN_POINT('Ctrl Pts',(3.53634427120997,0.136328894393368,-1.31838984174237E-16));
#46084=CARTESIAN_POINT('Ctrl Pts',(3.53350080053847,0.211006897749522,-1.93541387126446E-16));
#46085=CARTESIAN_POINT('Ctrl Pts',(3.52832339789583,0.285588347755748,-7.27345771358064E-17));
#46086=CARTESIAN_POINT('Ctrl Pts',(3.52083348352867,0.359802147884021,-1.31838984174237E-16));
#46087=CARTESIAN_POINT('Ctrl Pts',(3.51700351154709,0.397751416888196,-1.620620564082E-16));
#46088=CARTESIAN_POINT('Ctrl Pts',(3.5125699817729,0.435600311646885,2.2803504033583E-16));
#46089=CARTESIAN_POINT('Ctrl Pts',(3.5075361770783,0.473331412925596,1.87350135405495E-16));
#46090=CARTESIAN_POINT('Ctrl Pts',(3.49608873487737,0.559136212132028,9.48280520320672E-17));
#46091=CARTESIAN_POINT('Ctrl Pts',(3.48153875813074,0.644349892122457,9.44312770845489E-18));
#46092=CARTESIAN_POINT('Ctrl Pts',(3.46387334496763,0.72891602679703,-5.55111512312578E-17));
#46093=CARTESIAN_POINT('Ctrl Pts',(3.45224750382509,0.784570114176018,-9.82584179670611E-17));
#46094=CARTESIAN_POINT('Ctrl Pts',(3.43927126982642,0.839943685437852,2.39787204036035E-17));
#46095=CARTESIAN_POINT('Ctrl Pts',(3.42492877103772,0.895018163495264,-4.16333634234434E-17));
#46096=CARTESIAN_POINT('Ctrl Pts',(3.41442478500919,0.935352944523725,-8.96855488881198E-17));
#46097=CARTESIAN_POINT('Ctrl Pts',(3.40318658623661,0.975530746433315,1.11794948779964E-16));
#46098=CARTESIAN_POINT('Ctrl Pts',(3.39121177775683,1.0155208901864,1.2490009027033E-16));
#46099=CARTESIAN_POINT('Ctrl Pts',(3.36752469815931,1.09462442823421,1.80738876930359E-16));
#46100=CARTESIAN_POINT('Ctrl Pts',(3.34095533515231,1.17299052953756,-1.19499472761792E-16));
#46101=CARTESIAN_POINT('Ctrl Pts',(3.3116102147096,1.2503974394701,-1.2490009027033E-16));
#46102=CARTESIAN_POINT('Ctrl Pts',(3.28815858462756,1.31225842999066,-1.29216081553176E-16));
#46103=CARTESIAN_POINT('Ctrl Pts',(3.2629344689088,1.37350678139125,3.39993763381456E-16));
#46104=CARTESIAN_POINT('Ctrl Pts',(3.23599822549168,1.43403048862511,2.77555756156289E-16));
#46105=CARTESIAN_POINT('Ctrl Pts',(3.20059471381763,1.51357950897026,1.95490685557198E-16));
#46106=CARTESIAN_POINT('Ctrl Pts',(3.16223650327715,1.59188240530522,1.34206159441388E-16));
#46107=CARTESIAN_POINT('Ctrl Pts',(3.12094944371241,1.66888339837784,9.71445146547012E-17));
#46108=CARTESIAN_POINT('Ctrl Pts',(3.08975243467893,1.72706629398237,6.91402808973229E-17));
#46109=CARTESIAN_POINT('Ctrl Pts',(3.0568822049507,1.78450547174452,-3.62912008896638E-17));
#46110=CARTESIAN_POINT('Ctrl Pts',(3.02233378145072,1.84116537654111,0.));
#46111=CARTESIAN_POINT('Ctrl Pts',(2.99901028957703,1.87941623418409,2.45000333817547E-17));
#46112=CARTESIAN_POINT('Ctrl Pts',(2.974919809587,1.91731447029493,2.10095953603969E-16));
#46113=CARTESIAN_POINT('Ctrl Pts',(2.95006469153859,1.95483542786409,2.08166817117217E-16));
#46114=CARTESIAN_POINT('Ctrl Pts',(2.88489660607661,2.05321230801891,2.03108779123126E-16));
#46115=CARTESIAN_POINT('Ctrl Pts',(2.8144819340267,2.14897369239657,-2.965152410952E-17));
#46116=CARTESIAN_POINT('Ctrl Pts',(2.73904724714154,2.24141498451818,-8.32667268468867E-17));
#46117=CARTESIAN_POINT('Ctrl Pts',(2.70229826855952,2.28644894972098,-1.0938606290333E-16));
#46118=CARTESIAN_POINT('Ctrl Pts',(2.66435761337232,2.33069592454894,-3.5640658198706E-17));
#46119=CARTESIAN_POINT('Ctrl Pts',(2.62525892065778,2.37406997285321,-2.77555756156289E-17));
#46120=CARTESIAN_POINT('Ctrl Pts',(2.5707368279943,2.4345539357852,-1.67600365475454E-17));
#46121=CARTESIAN_POINT('Ctrl Pts',(2.51397031226346,2.49332645267094,5.10850161412582E-17));
#46122=CARTESIAN_POINT('Ctrl Pts',(2.45517505526017,2.55006466651292,-8.32667268468867E-17));
#46123=CARTESIAN_POINT('Ctrl Pts',(2.40728457699653,2.5962796221949,-1.92700200824151E-16));
#46124=CARTESIAN_POINT('Ctrl Pts',(2.3580489717218,2.64114531836818,-2.20460030602934E-16));
#46125=CARTESIAN_POINT('Ctrl Pts',(2.30760323636819,2.68450503882998,-2.77555756156289E-16));
#46126=CARTESIAN_POINT('Ctrl Pts',(2.27865530387642,2.7093867112249,-3.38235922399021E-16));
#46127=CARTESIAN_POINT('Ctrl Pts',(2.24931159991021,2.73377088022847,1.71863076464404E-16));
#46128=CARTESIAN_POINT('Ctrl Pts',(2.21959827171105,2.75764646490264,1.38777878078145E-16));
#46129=CARTESIAN_POINT('Ctrl Pts',(2.14143730410158,2.82045123681735,5.17471993844663E-17));
#46130=CARTESIAN_POINT('Ctrl Pts',(2.06070142653763,2.87975713463521,-1.56650036923279E-16));
#46131=CARTESIAN_POINT('Ctrl Pts',(1.97762156218559,2.93552733768934,-1.11022302462516E-16));
#46132=CARTESIAN_POINT('Ctrl Pts',(1.92211983121906,2.97278477461466,-8.05405694649354E-17));
#46133=CARTESIAN_POINT('Ctrl Pts',(1.86557114727434,3.00846349169955,-2.42724910906657E-17));
#46134=CARTESIAN_POINT('Ctrl Pts',(1.80803658801739,3.0425422416155,0.));
#46135=CARTESIAN_POINT('Ctrl Pts',(1.7188400885876,3.09537492577444,3.76299265291851E-17));
#46136=CARTESIAN_POINT('Ctrl Pts',(1.62727618984203,3.14435347841968,-5.86239920736008E-20));
#46137=CARTESIAN_POINT('Ctrl Pts',(1.53385010392579,3.18924471308555,5.55111512312578E-17));
#46138=CARTESIAN_POINT('Ctrl Pts',(1.47764192286276,3.21625274431682,8.89437408206909E-17));
#46139=CARTESIAN_POINT('Ctrl Pts',(1.42076021590392,3.24178219173936,8.07486977161786E-17));
#46140=CARTESIAN_POINT('Ctrl Pts',(1.36331845320285,3.26579067475782,1.11022302462516E-16));
#46141=CARTESIAN_POINT('Ctrl Pts',(1.31009042500589,3.28803797621554,1.39075137391133E-16));
#46142=CARTESIAN_POINT('Ctrl Pts',(1.25638952610923,3.3089769997134,-7.7221606089057E-17));
#46143=CARTESIAN_POINT('Ctrl Pts',(1.20225233191348,3.32859739842768,-5.55111512312578E-17));
#46144=CARTESIAN_POINT('Ctrl Pts',(1.1142617813533,3.36048692855069,-2.0224600012103E-17));
#46145=CARTESIAN_POINT('Ctrl Pts',(1.02511436445074,3.38889779844708,-1.78457313905869E-17));
#46146=CARTESIAN_POINT('Ctrl Pts',(0.934925304373438,3.41375797748399,-5.55111512312578E-17));
#46147=CARTESIAN_POINT('Ctrl Pts',(0.885809238120318,3.42729658404664,-7.60233647387536E-17));
#46148=CARTESIAN_POINT('Ctrl Pts',(0.836383195275312,3.43978145529386,-2.05712469523657E-16));
#46149=CARTESIAN_POINT('Ctrl Pts',(0.786666628307869,3.4511940464116,-1.38777878078145E-16));
#46150=CARTESIAN_POINT('Ctrl Pts',(0.690297762049071,3.47331581656142,-9.03419132430871E-18));
#46151=CARTESIAN_POINT('Ctrl Pts',(0.59285483884902,3.49139795611778,8.42365090681754E-17));
#46152=CARTESIAN_POINT('Ctrl Pts',(0.494841798296601,3.50524344299471,1.11022302462516E-16));
#46153=CARTESIAN_POINT('Ctrl Pts',(0.432069322108475,3.51411078850706,1.28713363252148E-16));
#46154=CARTESIAN_POINT('Ctrl Pts',(0.369063375024884,3.52124159998704,1.271306364805E-16));
#46155=CARTESIAN_POINT('Ctrl Pts',(0.305964768744507,3.52664906588399,1.66533453693773E-16));
#46156=CARTESIAN_POINT('Ctrl Pts',(0.269285915132926,3.52979239442539,1.89438082649088E-16));
#46157=CARTESIAN_POINT('Ctrl Pts',(0.232581119446525,3.53235340649015,2.30811615431158E-17));
#46158=CARTESIAN_POINT('Ctrl Pts',(0.19585282992679,3.5343374073664,2.77555756156289E-17));
#46159=CARTESIAN_POINT('Ctrl Pts',(0.119441498428624,3.53846501991332,3.74804554813947E-17));
#46160=CARTESIAN_POINT('Ctrl Pts',(0.0429151096247929,3.54010034667225,
6.94070683690155E-17));
#46161=CARTESIAN_POINT('Ctrl Pts',(-0.0338049752335097,3.53925398805205,
1.38777878078145E-16));
#46162=CARTESIAN_POINT('Ctrl Pts',(-0.110525060091812,3.53840762943185,
2.08148687787274E-16));
#46163=CARTESIAN_POINT('Ctrl Pts',(-0.187439519225311,3.5350795447432,-4.39206313887317E-17));
#46164=CARTESIAN_POINT('Ctrl Pts',(-0.264621262814249,3.52921885147511,
-1.11022302462516E-16));
#46165=CARTESIAN_POINT('',(-0.278675535189408,3.52854398769841,0.000242178628510733));
#46166=CARTESIAN_POINT('Ctrl Pts',(-0.278642183567104,3.52812649287716,
0.000242178628510788));
#46167=CARTESIAN_POINT('Ctrl Pts',(-0.273969233930499,3.52849979200248,
0.000161453268946271));
#46168=CARTESIAN_POINT('Ctrl Pts',(-0.26929558191709,3.52886391325551,8.07279093816785E-5));
#46169=CARTESIAN_POINT('Ctrl Pts',(-0.264621264353401,3.52921885135824,
2.54981716296676E-9));
#46170=CARTESIAN_POINT('',(-2.97253954097099,-2.67651699463381,-6.72783956812026E-18));
#46171=CARTESIAN_POINT('Ctrl Pts',(-0.278697848415911,3.52896236434037,
2.38524477946811E-17));
#46172=CARTESIAN_POINT('Ctrl Pts',(-0.754955028066917,3.51933407567894,
2.38524477946811E-17));
#46173=CARTESIAN_POINT('Ctrl Pts',(-1.18674072769151,3.41430558451068,-1.24655644773836E-14));
#46174=CARTESIAN_POINT('Ctrl Pts',(-1.96733714971687,3.09598181816572,-1.24622173902629E-14));
#46175=CARTESIAN_POINT('Ctrl Pts',(-2.34699951566166,2.85180221342043,-2.1094237467878E-14));
#46176=CARTESIAN_POINT('Ctrl Pts',(-2.99020885234353,2.24735338315926,-2.1094237467878E-14));
#46177=CARTESIAN_POINT('Ctrl Pts',(-3.29244004341223,1.85806081342808,-4.6609974510937E-14));
#46178=CARTESIAN_POINT('Ctrl Pts',(-3.71972888834082,0.9162945088732,-4.66139109655266E-14));
#46179=CARTESIAN_POINT('Ctrl Pts',(-3.83362815108384,0.428864103968153,
-7.34116402883767E-14));
#46180=CARTESIAN_POINT('Ctrl Pts',(-3.86808345271407,-0.535129438249572,
-7.34152353651497E-14));
#46181=CARTESIAN_POINT('Ctrl Pts',(-3.79982816305649,-0.999034854858048,
-5.31172328344098E-14));
#46182=CARTESIAN_POINT('Ctrl Pts',(-3.48665287488867,-1.93562500296496,
-5.31172328344098E-14));
#46183=CARTESIAN_POINT('Ctrl Pts',(-3.23969235129666,-2.34687602292039,
-1.9992468236924E-17));
#46184=CARTESIAN_POINT('Ctrl Pts',(-2.97252122137584,-2.6765004993568,-1.9992468236924E-17));
#46185=CARTESIAN_POINT('Ctrl Pts',(-2.97255786056614,-2.67653348991082,
6.53678910068347E-18));
#46186=CARTESIAN_POINT('Ctrl Pts',(-2.66529278319453,-2.98406739191157,
6.53678910068347E-18));
#46187=CARTESIAN_POINT('Ctrl Pts',(-2.30678228389453,-3.24050676320864,
3.24897772374216E-14));
#46188=CARTESIAN_POINT('Ctrl Pts',(-1.53166232714772,-3.62228294569805,
3.24929449932003E-14));
#46189=CARTESIAN_POINT('Ctrl Pts',(-1.12143089614916,-3.74638918522431,
3.97756064862856E-14));
#46190=CARTESIAN_POINT('Ctrl Pts',(-0.259412793720378,-3.85602623074799,
3.97788478927697E-14));
#46191=CARTESIAN_POINT('Ctrl Pts',(0.239543577753453,-3.84465005200125,
4.68007943103259E-14));
#46192=CARTESIAN_POINT('Ctrl Pts',(1.22159631150557,-3.5865596742176,4.68046624085105E-14));
#46193=CARTESIAN_POINT('Ctrl Pts',(1.66110604070138,-3.37568430365941,3.39640246886428E-14));
#46194=CARTESIAN_POINT('Ctrl Pts',(2.54221189401124,-2.72072246706673,3.3968295615247E-14));
#46195=CARTESIAN_POINT('Ctrl Pts',(2.83181469633017,-2.31316909850315,2.74445762896468E-14));
#46196=CARTESIAN_POINT('Ctrl Pts',(3.1232636873208,-1.82954859920293,2.74423321302002E-14));
#46197=CARTESIAN_POINT('Ctrl Pts',(3.23034582646799,-1.60226308336958,2.94209101525666E-14));
#46198=CARTESIAN_POINT('Ctrl Pts',(3.39277224036371,-1.13390966780497,2.94209101525666E-14));
#46199=CARTESIAN_POINT('Ctrl Pts',(3.44860799855318,-0.893678441777806,
-3.9176209116266E-18));
#46200=CARTESIAN_POINT('Ctrl Pts',(3.47936545786246,-0.65067010563865,-3.9176209116266E-18));
#46201=CARTESIAN_POINT('',(-3.82702124733548E-16,3.125,0.));
#46202=CARTESIAN_POINT('Origin',(0.,0.,0.));
#46203=CARTESIAN_POINT('Origin',(0.,0.,0.));
#46204=CARTESIAN_POINT('',(-3.82702124733548E-16,3.125,-12.2));
#46205=CARTESIAN_POINT('Origin',(0.,0.,-12.2));
#46206=CARTESIAN_POINT('',(-3.82702124733548E-16,3.125,0.));
#46207=CARTESIAN_POINT('Origin',(0.,0.,-12.2));
#46208=CARTESIAN_POINT('',(-3.5,3.32700602805782E-12,-12.2));
#46209=CARTESIAN_POINT('Origin',(0.,0.,-12.2));
#46210=CARTESIAN_POINT('Ctrl Pts',(-3.49999999998833,3.32743465443771E-12,
-12.2000000000021));
#46211=CARTESIAN_POINT('Ctrl Pts',(-3.49999999998833,-3.49999999998997,
-12.2000000000024));
#46212=CARTESIAN_POINT('Ctrl Pts',(4.96254670649323E-12,-3.49999999998997,
-12.2000000000027));
#46213=CARTESIAN_POINT('Ctrl Pts',(3.49999999999826,-3.49999999998997,-12.200000000003));
#46214=CARTESIAN_POINT('Ctrl Pts',(3.49999999999826,3.32743465443771E-12,
-12.2000000000027));
#46215=CARTESIAN_POINT('Ctrl Pts',(3.49999999999826,3.49999999999662,-12.2000000000024));
#46216=CARTESIAN_POINT('Ctrl Pts',(4.96254670649327E-12,3.49999999999662,
-12.2000000000021));
#46217=CARTESIAN_POINT('Ctrl Pts',(-3.49999999998833,3.49999999999662,-12.2000000000018));
#46218=CARTESIAN_POINT('Ctrl Pts',(-3.49999999998833,3.32743465443771E-12,
-12.2000000000021));
#46219=CARTESIAN_POINT('Ctrl Pts',(-4.62347603751425,3.32743465443744E-12,
-12.199999999999));
#46220=CARTESIAN_POINT('Ctrl Pts',(-4.62347603751425,-4.62347603751589,
-12.1999999999994));
#46221=CARTESIAN_POINT('Ctrl Pts',(4.96254670649346E-12,-4.62347603751589,
-12.1999999999998));
#46222=CARTESIAN_POINT('Ctrl Pts',(4.62347603752418,-4.62347603751589,-12.2000000000002));
#46223=CARTESIAN_POINT('Ctrl Pts',(4.62347603752418,3.32743465443745E-12,
-12.1999999999998));
#46224=CARTESIAN_POINT('Ctrl Pts',(4.62347603752418,4.62347603752254,-12.1999999999994));
#46225=CARTESIAN_POINT('Ctrl Pts',(4.96254670649352E-12,4.62347603752254,
-12.199999999999));
#46226=CARTESIAN_POINT('Ctrl Pts',(-4.62347603751425,4.62347603752254,-12.1999999999986));
#46227=CARTESIAN_POINT('Ctrl Pts',(-4.62347603751425,3.32743465443744E-12,
-12.199999999999));
#46228=CARTESIAN_POINT('Ctrl Pts',(-5.62084621677168,3.28230425252773E-12,
-11.6828432225872));
#46229=CARTESIAN_POINT('Ctrl Pts',(-5.62084621677167,-5.6208462167734,-11.6828432225877));
#46230=CARTESIAN_POINT('Ctrl Pts',(5.00412375663656E-12,-5.6208462167734,
-11.6828432225882));
#46231=CARTESIAN_POINT('Ctrl Pts',(5.62084621678168,-5.6208462167734,-11.6828432225886));
#46232=CARTESIAN_POINT('Ctrl Pts',(5.62084621678168,3.28230425252773E-12,
-11.6828432225881));
#46233=CARTESIAN_POINT('Ctrl Pts',(5.62084621678168,5.62084621677996,-11.6828432225876));
#46234=CARTESIAN_POINT('Ctrl Pts',(5.00412375663663E-12,5.62084621677996,
-11.6828432225872));
#46235=CARTESIAN_POINT('Ctrl Pts',(-5.62084621677167,5.62084621677996,-11.6828432225867));
#46236=CARTESIAN_POINT('Ctrl Pts',(-5.62084621677168,3.28230425252773E-12,
-11.6828432225872));
#46237=CARTESIAN_POINT('',(-0.5,5.484827557301,-11.73961639634));
#46238=CARTESIAN_POINT('',(0.5,5.484827557301,-11.73961639634));
#46239=CARTESIAN_POINT('Ctrl Pts',(0.500000000000787,5.48482755730098,-11.7396163963385));
#46240=CARTESIAN_POINT('Ctrl Pts',(0.442684070576578,5.51791892458297,-11.7261817950198));
#46241=CARTESIAN_POINT('Ctrl Pts',(0.381778410179616,5.54550032053989,-11.7147465052769));
#46242=CARTESIAN_POINT('Ctrl Pts',(0.225874984854292,5.59779342699823,-11.6928840241783));
#46243=CARTESIAN_POINT('Ctrl Pts',(0.129395940067804,5.6152273204819,-11.685424085685));
#46244=CARTESIAN_POINT('Ctrl Pts',(-0.0633603875161564,5.62128903423765,
-11.6828439564321));
#46245=CARTESIAN_POINT('Ctrl Pts',(-0.15776624407999,5.6107743725528,-11.6873559211886));
#46246=CARTESIAN_POINT('Ctrl Pts',(-0.337799258730956,5.56446316521236,
-11.706856455775));
#46247=CARTESIAN_POINT('Ctrl Pts',(-0.422085563497117,5.5298114781902,-11.7213535957186));
#46248=CARTESIAN_POINT('Ctrl Pts',(-0.500000000000555,5.48482755730112,
-11.7396163963379));
#46249=CARTESIAN_POINT('',(4.5,3.175426480543,-11.73961639634));
#46250=CARTESIAN_POINT('Ctrl Pts',(4.49999999999983,3.17542648054266,-11.7396163963401));
#46251=CARTESIAN_POINT('Ctrl Pts',(4.44888679227145,3.20493670478379,-11.7515971070228));
#46252=CARTESIAN_POINT('Ctrl Pts',(4.39760419976511,3.23454472337207,-11.7629653582921));
#46253=CARTESIAN_POINT('Ctrl Pts',(3.72427898920667,3.62328921494017,-11.9041229940746));
#46254=CARTESIAN_POINT('Ctrl Pts',(3.08384652281725,3.99304307180789,-11.9489869609561));
#46255=CARTESIAN_POINT('Ctrl Pts',(2.50000000000225,4.33012701892057,-11.9489869609561));
#46256=CARTESIAN_POINT('Ctrl Pts',(1.91615347718725,4.66721096603325,-11.948986960956));
#46257=CARTESIAN_POINT('Ctrl Pts',(1.27572101079784,5.03696482290097,-11.9041229940743));
#46258=CARTESIAN_POINT('Ctrl Pts',(0.602395800237954,5.4257093144699,-11.7629653582913));
#46259=CARTESIAN_POINT('Ctrl Pts',(0.551113207730164,5.45531733305902,-11.7515971070216));
#46260=CARTESIAN_POINT('Ctrl Pts',(0.500000000000331,5.48482755730098,-11.7396163963385));
#46261=CARTESIAN_POINT('',(5.,2.309401076759,-11.73961639634));
#46262=CARTESIAN_POINT('Ctrl Pts',(4.50000000000015,3.17542648054335,-11.7396163963398));
#46263=CARTESIAN_POINT('Ctrl Pts',(4.57791443650374,3.13044255965423,-11.7213535957204));
#46264=CARTESIAN_POINT('Ctrl Pts',(4.65006683013206,3.07477432204653,-11.7068564557768));
#46265=CARTESIAN_POINT('Ctrl Pts',(4.78019001949428,2.94201676150879,-11.6873559211905));
#46266=CARTESIAN_POINT('Ctrl Pts',(4.83649891190742,2.86551622230077,-11.682843956434));
#46267=CARTESIAN_POINT('Ctrl Pts',(4.92762747759628,2.6955534889947,-11.6854240856869));
#46268=CARTESIAN_POINT('Ctrl Pts',(4.96076880534568,2.60328323853475,-11.6928840241803));
#46269=CARTESIAN_POINT('Ctrl Pts',(4.99343335937216,2.44212035843757,-11.7147465052788));
#46270=CARTESIAN_POINT('Ctrl Pts',(5.,2.37558381132197,-11.7261817950215));
#46271=CARTESIAN_POINT('Ctrl Pts',(5.,2.30940107675898,-11.7396163963399));
#46272=CARTESIAN_POINT('',(5.,-2.309401076759,-11.73961639634));
#46273=CARTESIAN_POINT('Ctrl Pts',(5.,-2.30940107675881,-11.739616396339));
#46274=CARTESIAN_POINT('Ctrl Pts',(5.,-2.25038062827441,-11.7515971070222));
#46275=CARTESIAN_POINT('Ctrl Pts',(5.,-2.19116459109572,-11.762965358292));
#46276=CARTESIAN_POINT('Ctrl Pts',(5.,-1.41367560795741,-11.9041229940749));
#46277=CARTESIAN_POINT('Ctrl Pts',(5.,-0.674167894222026,-11.9489869609566));
#46278=CARTESIAN_POINT('Ctrl Pts',(5.,3.30552965419114E-12,-11.9489869609566));
#46279=CARTESIAN_POINT('Ctrl Pts',(5.,0.674167894228636,-11.9489869609565));
#46280=CARTESIAN_POINT('Ctrl Pts',(5.,1.41367560796401,-11.9041229940747));
#46281=CARTESIAN_POINT('Ctrl Pts',(5.,2.19116459110015,-11.762965358292));
#46282=CARTESIAN_POINT('Ctrl Pts',(5.,2.25038062827671,-11.7515971070227));
#46283=CARTESIAN_POINT('Ctrl Pts',(5.,2.30940107675899,-11.7396163963399));
#46284=CARTESIAN_POINT('',(4.5,-3.175426480543,-11.73961639634));
#46285=CARTESIAN_POINT('Ctrl Pts',(5.,-2.3094010767588,-11.739616396339));
#46286=CARTESIAN_POINT('Ctrl Pts',(5.00000000000002,-2.39936891853743,-11.7213535957195));
#46287=CARTESIAN_POINT('Ctrl Pts',(4.98786608886193,-2.48968884316767,-11.7068564557758));
#46288=CARTESIAN_POINT('Ctrl Pts',(4.93795626357266,-2.66875761104596,-11.6873559211893));
#46289=CARTESIAN_POINT('Ctrl Pts',(4.89985929942184,-2.75577281193861,-11.6828439564328));
#46290=CARTESIAN_POINT('Ctrl Pts',(4.79823153752659,-2.91967383148839,-11.6854240856856));
#46291=CARTESIAN_POINT('Ctrl Pts',(4.73489382048948,-2.99451018846436,-11.692884024179));
#46292=CARTESIAN_POINT('Ctrl Pts',(4.61165494919162,-3.10337996210302,-11.7147465052774));
#46293=CARTESIAN_POINT('Ctrl Pts',(4.55731592942336,-3.14233511326201,-11.7261817950201));
#46294=CARTESIAN_POINT('Ctrl Pts',(4.49999999999993,-3.17542648054348,-11.7396163963385));
#46295=CARTESIAN_POINT('',(0.5,-5.484827557301,-11.73961639634));
#46296=CARTESIAN_POINT('Ctrl Pts',(0.500000000000835,-5.48482755730095,
-11.7396163963363));
#46297=CARTESIAN_POINT('Ctrl Pts',(0.551113207731787,-5.45531733305834,
-11.7515971070197));
#46298=CARTESIAN_POINT('Ctrl Pts',(0.602395800240705,-5.42570931446857,
-11.7629653582897));
#46299=CARTESIAN_POINT('Ctrl Pts',(1.27572101080142,-5.03696482289917,-11.904122994073));
#46300=CARTESIAN_POINT('Ctrl Pts',(1.91615347719049,-4.66721096603164,-11.948986960955));
#46301=CARTESIAN_POINT('Ctrl Pts',(2.50000000000522,-4.33012701891911,-11.948986960955));
#46302=CARTESIAN_POINT('Ctrl Pts',(3.08384652281996,-3.99304307180658,-11.948986960955));
#46303=CARTESIAN_POINT('Ctrl Pts',(3.72427898920903,-3.62328921493906,-11.9041229940731));
#46304=CARTESIAN_POINT('Ctrl Pts',(4.39760419976643,-3.23454472337157,-11.7629653582905));
#46305=CARTESIAN_POINT('Ctrl Pts',(4.44888679227204,-3.20493670478371,-11.7515971070213));
#46306=CARTESIAN_POINT('Ctrl Pts',(4.49999999999971,-3.17542648054299,-11.7396163963387));
#46307=CARTESIAN_POINT('',(-0.5,-5.484827557301,-11.73961639634));
#46308=CARTESIAN_POINT('Ctrl Pts',(0.50000000000084,-5.48482755730095,-11.7396163963363));
#46309=CARTESIAN_POINT('Ctrl Pts',(0.422085563496947,-5.52981147819033,
-11.7213535957167));
#46310=CARTESIAN_POINT('Ctrl Pts',(0.337799258730246,-5.56446316521267,
-11.7068564557729));
#46311=CARTESIAN_POINT('Ctrl Pts',(0.157766244078805,-5.61077437255297,
-11.6873559211863));
#46312=CARTESIAN_POINT('Ctrl Pts',(0.0633603875151218,-5.6212890342377,
-11.6828439564298));
#46313=CARTESIAN_POINT('Ctrl Pts',(-0.129395940068389,-5.6152273204818,
-11.6854240856825));
#46314=CARTESIAN_POINT('Ctrl Pts',(-0.225874984854586,-5.59779342699814,
-11.6928840241757));
#46315=CARTESIAN_POINT('Ctrl Pts',(-0.381778410179812,-5.54550032053983,
-11.7147465052743));
#46316=CARTESIAN_POINT('Ctrl Pts',(-0.442684070576918,-5.51791892458282,
-11.7261817950172));
#46317=CARTESIAN_POINT('Ctrl Pts',(-0.500000000001249,-5.48482755730072,
-11.7396163963359));
#46318=CARTESIAN_POINT('',(-4.5,-3.175426480543,-11.73961639634));
#46319=CARTESIAN_POINT('Ctrl Pts',(-4.49999999999882,-3.17542648054325,
-11.7396163963343));
#46320=CARTESIAN_POINT('Ctrl Pts',(-4.44888679226865,-3.20493670478541,
-11.7515971070176));
#46321=CARTESIAN_POINT('Ctrl Pts',(-4.39760419976052,-3.23454472337472,
-11.7629653582874));
#46322=CARTESIAN_POINT('Ctrl Pts',(-3.72427898920092,-3.62328921494349,
-11.9041229940708));
#46323=CARTESIAN_POINT('Ctrl Pts',(-3.08384652281212,-3.99304307181085,
-11.9489869609528));
#46324=CARTESIAN_POINT('Ctrl Pts',(-2.49999999999764,-4.33012701892324,
-11.9489869609528));
#46325=CARTESIAN_POINT('Ctrl Pts',(-1.91615347718316,-4.66721096603562,
-11.9489869609529));
#46326=CARTESIAN_POINT('Ctrl Pts',(-1.27572101079435,-5.03696482290299,
-11.9041229940711));
#46327=CARTESIAN_POINT('Ctrl Pts',(-0.602395800236188,-5.42570931447092,
-11.7629653582882));
#46328=CARTESIAN_POINT('Ctrl Pts',(-0.551113207729517,-5.45531733305939,
-11.7515971070188));
#46329=CARTESIAN_POINT('Ctrl Pts',(-0.500000000000796,-5.48482755730071,
-11.7396163963359));
#46330=CARTESIAN_POINT('',(-5.,-2.309401076759,-11.73961639634));
#46331=CARTESIAN_POINT('Ctrl Pts',(-4.49999999999914,-3.17542648054393,
-11.739616396334));
#46332=CARTESIAN_POINT('Ctrl Pts',(-4.5779144365027,-3.13044255965495,-11.7213535957145));
#46333=CARTESIAN_POINT('Ctrl Pts',(-4.65006683013103,-3.0747743220474,-11.7068564557708));
#46334=CARTESIAN_POINT('Ctrl Pts',(-4.78019001949316,-2.94201676151012,
-11.6873559211842));
#46335=CARTESIAN_POINT('Ctrl Pts',(-4.83649891190626,-2.86551622230246,
-11.6828439564276));
#46336=CARTESIAN_POINT('Ctrl Pts',(-4.92762747759513,-2.69555348899732,
-11.6854240856803));
#46337=CARTESIAN_POINT('Ctrl Pts',(-4.96076880534464,-2.60328323853797,
-11.6928840241735));
#46338=CARTESIAN_POINT('Ctrl Pts',(-4.99343335937199,-2.44212035843974,
-11.7147465052721));
#46339=CARTESIAN_POINT('Ctrl Pts',(-5.00000000000008,-2.37558381132245,
-11.7261817950152));
#46340=CARTESIAN_POINT('Ctrl Pts',(-5.,-2.30940107675779,-11.739616396334));
#46341=CARTESIAN_POINT('',(-5.,3.30530319330631E-12,-11.9489869609522));
#46342=CARTESIAN_POINT('Ctrl Pts',(-5.,3.30541150006525E-12,-11.9489869609522));
#46343=CARTESIAN_POINT('Ctrl Pts',(-5.,-0.674167894221416,-11.9489869609523));
#46344=CARTESIAN_POINT('Ctrl Pts',(-5.,-1.41367560795614,-11.9041229940705));
#46345=CARTESIAN_POINT('Ctrl Pts',(-5.,-2.19116459109405,-11.7629653582872));
#46346=CARTESIAN_POINT('Ctrl Pts',(-5.,-2.25038062827307,-11.7515971070173));
#46347=CARTESIAN_POINT('Ctrl Pts',(-5.,-2.30940107675779,-11.739616396334));
#46348=CARTESIAN_POINT('Ctrl Pts',(-5.,3.3055296541908E-12,-11.9489869609522));
#46349=CARTESIAN_POINT('Ctrl Pts',(-4.27100251525133,3.32743465443753E-12,
-12.2));
#46350=CARTESIAN_POINT('Ctrl Pts',(-3.49999999998833,3.32743465443771E-12,
-12.2000000000021));
#46351=CARTESIAN_POINT('',(-5.,2.309401076758,-11.73961639634));
#46352=CARTESIAN_POINT('Ctrl Pts',(-5.,2.30940107675701,-11.7396163963351));
#46353=CARTESIAN_POINT('Ctrl Pts',(-5.,2.25038062827473,-11.7515971070179));
#46354=CARTESIAN_POINT('Ctrl Pts',(-5.,2.19116459109816,-11.7629653582873));
#46355=CARTESIAN_POINT('Ctrl Pts',(-5.,1.41367560796274,-11.9041229940702));
#46356=CARTESIAN_POINT('Ctrl Pts',(-5.,0.674167894228026,-11.9489869609522));
#46357=CARTESIAN_POINT('Ctrl Pts',(-5.,3.3056890558214E-12,-11.9489869609522));
#46358=CARTESIAN_POINT('',(-4.5,3.175426480543,-11.73961639634));
#46359=CARTESIAN_POINT('Ctrl Pts',(-5.,2.30940107675701,-11.7396163963351));
#46360=CARTESIAN_POINT('Ctrl Pts',(-5.00000000000018,2.39936891853531,-11.7213535957156));
#46361=CARTESIAN_POINT('Ctrl Pts',(-4.98786608886234,2.48968884316526,-11.7068564557719));
#46362=CARTESIAN_POINT('Ctrl Pts',(-4.93795626357369,2.66875761104321,-11.6873559211853));
#46363=CARTESIAN_POINT('Ctrl Pts',(-4.8998592994232,2.75577281193584,-11.6828439564288));
#46364=CARTESIAN_POINT('Ctrl Pts',(-4.79823153752867,2.91967383148563,-11.6854240856815));
#46365=CARTESIAN_POINT('Ctrl Pts',(-4.73489382049198,2.99451018846164,-11.6928840241748));
#46366=CARTESIAN_POINT('Ctrl Pts',(-4.61165494919357,3.10337996210165,-11.7147465052734));
#46367=CARTESIAN_POINT('Ctrl Pts',(-4.55731592942412,3.14233511326163,-11.7261817950164));
#46368=CARTESIAN_POINT('Ctrl Pts',(-4.49999999999936,3.17542648054381,-11.7396163963353));
#46369=CARTESIAN_POINT('Ctrl Pts',(-0.500000000000548,5.48482755730111,
-11.7396163963379));
#46370=CARTESIAN_POINT('Ctrl Pts',(-0.551113207728163,5.45531733306043,
-11.7515971070205));
#46371=CARTESIAN_POINT('Ctrl Pts',(-0.60239580023372,5.4257093144726,-11.7629653582897));
#46372=CARTESIAN_POINT('Ctrl Pts',(-1.27572101079105,5.03696482290515,-11.9041229940722));
#46373=CARTESIAN_POINT('Ctrl Pts',(-1.91615347718016,4.6672109660376,-11.9489869609538));
#46374=CARTESIAN_POINT('Ctrl Pts',(-2.49999999999489,4.33012701892508,-11.9489869609538));
#46375=CARTESIAN_POINT('Ctrl Pts',(-3.08384652280961,3.99304307181256,-11.9489869609537));
#46376=CARTESIAN_POINT('Ctrl Pts',(-3.72427898919873,3.62328921494501,-11.9041229940721));
#46377=CARTESIAN_POINT('Ctrl Pts',(-4.39760419975937,3.23454472337564,-11.7629653582888));
#46378=CARTESIAN_POINT('Ctrl Pts',(-4.44888679226823,3.20493670478591,-11.7515971070189));
#46379=CARTESIAN_POINT('Ctrl Pts',(-4.49999999999913,3.17542648054333,-11.7396163963355));
#46380=CARTESIAN_POINT('Origin',(0.,4.618802153517,-28.10392));
#46381=CARTESIAN_POINT('',(0.5,5.484827557301,-10.5));
#46382=CARTESIAN_POINT('',(-0.5,5.484827557301,-10.5));
#46383=CARTESIAN_POINT('Origin',(0.,4.618802153517,-10.5));
#46384=CARTESIAN_POINT('',(0.5,5.484827557301,-11.73961639634));
#46385=CARTESIAN_POINT('',(-0.5,5.484827557301,-11.73961639634));
#46386=CARTESIAN_POINT('Origin',(0.,0.,-10.5));
#46387=CARTESIAN_POINT('',(-4.5,3.175426480543,-10.5));
#46388=CARTESIAN_POINT('',(-4.5,3.175426480543,-10.5));
#46389=CARTESIAN_POINT('',(-5.,2.309401076759,-10.5));
#46390=CARTESIAN_POINT('Origin',(-4.,2.309401076759,-10.5));
#46391=CARTESIAN_POINT('',(-5.,-2.309401076759,-10.5));
#46392=CARTESIAN_POINT('',(-5.,-2.309401076759,-10.5));
#46393=CARTESIAN_POINT('',(-4.5,-3.175426480543,-10.5));
#46394=CARTESIAN_POINT('Origin',(-4.,-2.309401076759,-10.5));
#46395=CARTESIAN_POINT('',(-0.5,-5.484827557301,-10.5));
#46396=CARTESIAN_POINT('',(-0.5,-5.484827557301,-10.5));
#46397=CARTESIAN_POINT('',(0.5,-5.484827557301,-10.5));
#46398=CARTESIAN_POINT('Origin',(0.,-4.618802153517,-10.5));
#46399=CARTESIAN_POINT('',(4.5,-3.175426480543,-10.5));
#46400=CARTESIAN_POINT('',(4.5,-3.175426480543,-10.5));
#46401=CARTESIAN_POINT('',(5.,-2.309401076759,-10.5));
#46402=CARTESIAN_POINT('Origin',(4.,-2.309401076759,-10.5));
#46403=CARTESIAN_POINT('',(5.,2.309401076759,-10.5));
#46404=CARTESIAN_POINT('',(5.,2.309401076759,-10.5));
#46405=CARTESIAN_POINT('',(4.5,3.175426480543,-10.5));
#46406=CARTESIAN_POINT('Origin',(4.,2.309401076759,-10.5));
#46407=CARTESIAN_POINT('',(0.5,5.484827557301,-10.5));
#46408=CARTESIAN_POINT('',(0.,4.,-10.5));
#46409=CARTESIAN_POINT('Origin',(0.,0.,-10.5));
#46410=CARTESIAN_POINT('Origin',(0.,0.,0.525));
#46411=CARTESIAN_POINT('',(5.89886872482066E-17,4.,-7.77511165445773));
#46412=CARTESIAN_POINT('',(4.89858719658941E-16,4.,0.525));
#46413=CARTESIAN_POINT('',(3.46410161481665,-1.99999999976831,-8.02507037766139));
#46414=CARTESIAN_POINT('Ctrl Pts',(3.2612801348364E-15,4.,-7.77511165445773));
#46415=CARTESIAN_POINT('Ctrl Pts',(0.140778732285844,4.,-7.77934161327365));
#46416=CARTESIAN_POINT('Ctrl Pts',(0.281562623126605,3.99256795970819,-7.78354814467748));
#46417=CARTESIAN_POINT('Ctrl Pts',(0.653870198275523,3.95309174821613,-7.79466178870193));
#46418=CARTESIAN_POINT('Ctrl Pts',(0.883378592649572,3.90821221631589,-7.80149898784317));
#46419=CARTESIAN_POINT('Ctrl Pts',(1.41065467753745,3.75625914261328,-7.81796018704639));
#46420=CARTESIAN_POINT('Ctrl Pts',(1.70226943948582,3.63341618820113,-7.82745442148589));
#46421=CARTESIAN_POINT('Ctrl Pts',(2.19330078093717,3.35434968240981,-7.8441809508052));
#46422=CARTESIAN_POINT('Ctrl Pts',(2.39817450095537,3.21107275634099,-7.85153722441686));
#46423=CARTESIAN_POINT('Ctrl Pts',(2.78217511180761,2.88515562249177,-7.86670078290223));
#46424=CARTESIAN_POINT('Ctrl Pts',(2.95986659741527,2.70255684997506,-7.87432379850575));
#46425=CARTESIAN_POINT('Ctrl Pts',(3.2746594474262,2.31049777386795,-7.88922429124318));
#46426=CARTESIAN_POINT('Ctrl Pts',(3.41188551680376,2.10257724441769,-7.89653713856435));
#46427=CARTESIAN_POINT('Ctrl Pts',(3.64749116775576,1.66109269263352,-7.91159591530977));
#46428=CARTESIAN_POINT('Ctrl Pts',(3.74481430291147,1.42821183215052,-7.91916263122237));
#46429=CARTESIAN_POINT('Ctrl Pts',(3.89268525469654,0.952677249501694,-7.93393539966148));
#46430=CARTESIAN_POINT('Ctrl Pts',(3.9439231690797,0.711380494141654,-7.9411566697106));
#46431=CARTESIAN_POINT('Ctrl Pts',(3.99685095219547,0.261048337853231,-7.95478618466598));
#46432=CARTESIAN_POINT('Ctrl Pts',(4.00500813357676,0.0536167255429015,
-7.96103764007249));
#46433=CARTESIAN_POINT('Ctrl Pts',(3.98489990856592,-0.469954806053514,
-7.97666285858365));
#46434=CARTESIAN_POINT('Ctrl Pts',(3.93521088393896,-0.78383650500982,-7.98590074114378));
#46435=CARTESIAN_POINT('Ctrl Pts',(3.80435504362991,-1.24652798426401,-8.00036597408868));
#46436=CARTESIAN_POINT('Ctrl Pts',(3.74999731300928,-1.40159549116537,-8.00531733948733));
#46437=CARTESIAN_POINT('Ctrl Pts',(3.62159245785615,-1.70640549464178,-8.0152126777857));
#46438=CARTESIAN_POINT('Ctrl Pts',(3.54739645091892,-1.85572911241389,-8.02014529730486));
#46439=CARTESIAN_POINT('Ctrl Pts',(3.46410161516789,-1.9999999999478,-8.02507037834385));
#46440=CARTESIAN_POINT('',(3.4640667802615,-1.999976852445,-7.27511360468106));
#46441=CARTESIAN_POINT('',(3.464101615138,-2.,-8.025));
#46442=CARTESIAN_POINT('Ctrl Pts',(3.46410332849671,-1.99999703237231,-7.27513768185083));
#46443=CARTESIAN_POINT('Ctrl Pts',(3.35586300106758,-2.18747514981733,-7.28160344842495));
#46444=CARTESIAN_POINT('Ctrl Pts',(3.23258197797168,-2.36585667498483,-7.28797035088014));
#46445=CARTESIAN_POINT('Ctrl Pts',(2.96253849585541,-2.69581554812532,-7.30060798938785));
#46446=CARTESIAN_POINT('Ctrl Pts',(2.81702488992057,-2.84752954740615,-7.30693910263489));
#46447=CARTESIAN_POINT('Ctrl Pts',(2.34305642289716,-3.26963843275094,-7.32602735225743));
#46448=CARTESIAN_POINT('Ctrl Pts',(1.98284299927815,-3.49982606803557,-7.33834991377517));
#46449=CARTESIAN_POINT('Ctrl Pts',(1.3604085738985,-3.77010588037409,-7.35876508310621));
#46450=CARTESIAN_POINT('Ctrl Pts',(1.11852150423245,-3.84880786584587,-7.3663943452422));
#46451=CARTESIAN_POINT('Ctrl Pts',(0.616447115067628,-3.96079714425207,
-7.38165683539358));
#46452=CARTESIAN_POINT('Ctrl Pts',(0.357146543798483,-3.992538907047,-7.38930579330697));
#46453=CARTESIAN_POINT('Ctrl Pts',(-0.157696072795193,-4.00497685917401,
-7.40479909079884));
#46454=CARTESIAN_POINT('Ctrl Pts',(-0.412009437255292,-3.98684818401563,
-7.412446025683));
#46455=CARTESIAN_POINT('Ctrl Pts',(-0.919900651375685,-3.90150110816807,
-7.4277259558367));
#46456=CARTESIAN_POINT('Ctrl Pts',(-1.17208922886167,-3.83329289933414,
-7.4353757396454));
#46457=CARTESIAN_POINT('Ctrl Pts',(-1.65312578169036,-3.65123835423638,
-7.45084951467785));
#46458=CARTESIAN_POINT('Ctrl Pts',(-1.88132825994924,-3.53906383830923,
-7.45847619461585));
#46459=CARTESIAN_POINT('Ctrl Pts',(-2.31928013956748,-3.26938214774931,
-7.47373613423981));
#46460=CARTESIAN_POINT('Ctrl Pts',(-2.52730851911268,-3.11137126658911,
-7.48138496898291));
#46461=CARTESIAN_POINT('Ctrl Pts',(-2.90515881640126,-2.76130583412243,
-7.49688111703797));
#46462=CARTESIAN_POINT('Ctrl Pts',(-3.07490559617139,-2.57093674770182,
-7.50453101279154));
#46463=CARTESIAN_POINT('Ctrl Pts',(-3.37956067272974,-2.15557391372885,
-7.51981386213054));
#46464=CARTESIAN_POINT('Ctrl Pts',(-3.51279729686478,-1.93085056262191,
-7.52746378143529));
#46465=CARTESIAN_POINT('Ctrl Pts',(-3.7306700897575,-1.46506312330292,-7.54293428241289));
#46466=CARTESIAN_POINT('Ctrl Pts',(-3.81602919117647,-1.22565614517854,
-7.55055756936701));
#46467=CARTESIAN_POINT('Ctrl Pts',(-3.94198275788177,-0.727111070355683,
-7.56581415670827));
#46468=CARTESIAN_POINT('Ctrl Pts',(-3.98097214940275,-0.468805753691623,
-7.57346282862271));
#46469=CARTESIAN_POINT('Ctrl Pts',(-4.00783408750042,0.0457088510394772,
-7.58896272305745));
#46470=CARTESIAN_POINT('Ctrl Pts',(-3.99680256889971,0.300657827573293,
-7.59661651140217));
#46471=CARTESIAN_POINT('Ctrl Pts',(-3.9255927125405,0.810957805583728,-7.61190319735917));
#46472=CARTESIAN_POINT('Ctrl Pts',(-3.86442850093518,1.06495191091268,-7.61955329356721));
#46473=CARTESIAN_POINT('Ctrl Pts',(-3.69591527108494,1.55062713376603,-7.63501948572712));
#46474=CARTESIAN_POINT('Ctrl Pts',(-3.59026664206739,1.7816346800881,-7.64263830916872));
#46475=CARTESIAN_POINT('Ctrl Pts',(-3.34220362495083,2.21098074661499,-7.65735043678452));
#46476=CARTESIAN_POINT('Ctrl Pts',(-3.20210686624951,2.40941328215933,-7.66445800738338));
#46477=CARTESIAN_POINT('Ctrl Pts',(-2.90970717095085,2.75264826764198,-7.67800500544158));
#46478=CARTESIAN_POINT('Ctrl Pts',(-2.76230107077787,2.9005451583952,-7.6842970732713));
#46479=CARTESIAN_POINT('Ctrl Pts',(-2.4505214701389,3.16794066444546,-7.69655196788191));
#46480=CARTESIAN_POINT('Ctrl Pts',(-2.28723825110935,3.28777200012571,-7.7025029263712));
#46481=CARTESIAN_POINT('Ctrl Pts',(-1.71869730004351,3.64208556189983,-7.72235370186981));
#46482=CARTESIAN_POINT('Ctrl Pts',(-1.28148120429361,3.81791991428226,-7.73646510285903));
#46483=CARTESIAN_POINT('Ctrl Pts',(-0.696644060123244,3.94101312641292,
-7.75413628251737));
#46484=CARTESIAN_POINT('Ctrl Pts',(-0.568212890367792,3.96156931347538,
-7.7579824927024));
#46485=CARTESIAN_POINT('Ctrl Pts',(-0.293121491848629,3.99194467622145,
-7.76627846400883));
#46486=CARTESIAN_POINT('Ctrl Pts',(-0.146563545278887,4.,-7.77070788017748));
#46487=CARTESIAN_POINT('Ctrl Pts',(1.38777878078145E-15,4.,-7.77511165445773));
#46488=CARTESIAN_POINT('Origin',(3.464101615138,-2.,-8.5));
#46489=CARTESIAN_POINT('',(3.06563522285152,-1.76994531315727,-7.75941845703217));
#46490=CARTESIAN_POINT('Ctrl Pts',(3.0656354288223,-1.76994544006766,-7.75941803818134));
#46491=CARTESIAN_POINT('Ctrl Pts',(3.13205392611679,-1.80829217735981,-7.8036984058573));
#46492=CARTESIAN_POINT('Ctrl Pts',(3.19847242341131,-1.84663891465196,-7.84797877353323));
#46493=CARTESIAN_POINT('Ctrl Pts',(3.33129448534567,-1.92332376786409,-7.9365295534741));
#46494=CARTESIAN_POINT('Ctrl Pts',(3.39769804998552,-1.96166188378406,-7.98079996573903));
#46495=CARTESIAN_POINT('Ctrl Pts',(3.46410161462537,-1.99999999970403,-8.02507037800398));
#46496=CARTESIAN_POINT('',(3.06563502767401,-1.76994519830837,-7.54058067576584));
#46497=CARTESIAN_POINT('Ctrl Pts',(3.06563511413263,-1.76994525838149,-7.54058067576584));
#46498=CARTESIAN_POINT('Ctrl Pts',(3.06563511413263,-1.76994525838149,-7.57705378384389));
#46499=CARTESIAN_POINT('Ctrl Pts',(3.06563511413263,-1.76994525838149,-7.61352689192195));
#46500=CARTESIAN_POINT('Ctrl Pts',(3.06563511413263,-1.76994525838149,-7.68647281901072));
#46501=CARTESIAN_POINT('Ctrl Pts',(3.06563511413263,-1.76994525838149,-7.72294563802144));
#46502=CARTESIAN_POINT('Ctrl Pts',(3.06563511413263,-1.76994525838149,-7.75941845703217));
#46503=CARTESIAN_POINT('Ctrl Pts',(3.46400702067617,-1.999945385862,-7.27499059099672));
#46504=CARTESIAN_POINT('Ctrl Pts',(3.39763472540694,-1.96162532332158,-7.3192401563699));
#46505=CARTESIAN_POINT('Ctrl Pts',(3.33126243013771,-1.92330526078116,-7.36348972174309));
#46506=CARTESIAN_POINT('Ctrl Pts',(3.19847169694209,-1.84663849522478,-7.45201961521233));
#46507=CARTESIAN_POINT('Ctrl Pts',(3.13205325901568,-1.8082917922088,-7.49629994330838));
#46508=CARTESIAN_POINT('Ctrl Pts',(3.06563482108927,-1.76994508919283,-7.54058027140441));
#46509=CARTESIAN_POINT('Ctrl Pts',(0.5039879501212,-3.989475419894,-4.372769611617));
#46510=CARTESIAN_POINT('Ctrl Pts',(-0.0089492302955,-4.054274455078,-4.388116833839));
#46511=CARTESIAN_POINT('Ctrl Pts',(-1.059906716638,-3.983530501776,-4.418811278284));
#46512=CARTESIAN_POINT('Ctrl Pts',(-2.480771754885,-3.292085724309,-4.46485294495));
#46513=CARTESIAN_POINT('Ctrl Pts',(-3.537058667077,-2.116886952389,-4.510894611617));
#46514=CARTESIAN_POINT('Ctrl Pts',(-4.073613014997,-0.6306285969564,-4.556936278284));
#46515=CARTESIAN_POINT('Ctrl Pts',(-4.011576156733,0.9482964751911,-4.60297794495));
#46516=CARTESIAN_POINT('Ctrl Pts',(-3.360068212288,2.387876153023,-4.649019611617));
#46517=CARTESIAN_POINT('Ctrl Pts',(-2.214822403112,3.476574800745,-4.695061278284));
#46518=CARTESIAN_POINT('Ctrl Pts',(-0.7441245898171,4.054416019338,-4.74110294495));
#46519=CARTESIAN_POINT('Ctrl Pts',(0.8359169456045,4.036490248204,-4.787144611617));
#46520=CARTESIAN_POINT('Ctrl Pts',(2.29312655145,3.425431546469,-4.833186278284));
#46521=CARTESIAN_POINT('Ctrl Pts',(3.413377863899,2.311030553742,-4.87922794495));
#46522=CARTESIAN_POINT('Ctrl Pts',(4.03205808599,0.8570404032131,-4.925269611617));
#46523=CARTESIAN_POINT('Ctrl Pts',(4.058256652206,-0.7228856109492,-4.971311278284));
#46524=CARTESIAN_POINT('Ctrl Pts',(3.488123873377,-2.196588833996,-5.01735294495));
#46525=CARTESIAN_POINT('Ctrl Pts',(2.405436621222,-3.347519278951,-5.063394611617));
#46526=CARTESIAN_POINT('Ctrl Pts',(0.9692879252418,-4.006556074691,-5.109436278284));
#46527=CARTESIAN_POINT('Ctrl Pts',(-0.6092905926321,-4.076858549839,-5.15547794495));
#46528=CARTESIAN_POINT('Ctrl Pts',(-2.098338282431,-3.548096266189,-5.201519611617));
#46529=CARTESIAN_POINT('Ctrl Pts',(-3.279050399221,-2.497967001589,-5.247561278284));
#46530=CARTESIAN_POINT('Ctrl Pts',(-3.97792987147,-1.080779625702,-5.29360294495));
#46531=CARTESIAN_POINT('Ctrl Pts',(-4.092281435813,0.4952204678384,-5.339644611617));
#46532=CARTESIAN_POINT('Ctrl Pts',(-3.605301960262,1.998451509793,-5.385686278284));
#46533=CARTESIAN_POINT('Ctrl Pts',(-2.588549542429,3.208024614627,-5.43172794495));
#46534=CARTESIAN_POINT('Ctrl Pts',(-1.19142856672,3.946201798194,-5.477769611617));
#46535=CARTESIAN_POINT('Ctrl Pts',(0.3807641850203,4.104513283822,-5.523811278284));
#46536=CARTESIAN_POINT('Ctrl Pts',(1.897006404783,3.659696348315,-5.56985294495));
#46537=CARTESIAN_POINT('Ctrl Pts',(3.134497308938,2.677113610201,-5.615894611617));
#46538=CARTESIAN_POINT('Ctrl Pts',(3.91139659546,1.30114846758,-5.661936278284));
#46539=CARTESIAN_POINT('Ctrl Pts',(4.113544555839,-0.2660109937444,-5.70797794495));
#46540=CARTESIAN_POINT('Ctrl Pts',(3.711237015243,-1.794082071242,-5.754019611617));
#46541=CARTESIAN_POINT('Ctrl Pts',(2.763590145309,-3.058525816535,-5.800061278284));
#46542=CARTESIAN_POINT('Ctrl Pts',(1.409853772006,-3.873541403319,-5.84610294495));
#46543=CARTESIAN_POINT('Ctrl Pts',(-0.1510503750974,-4.119368209549,-5.892144611617));
#46544=CARTESIAN_POINT('Ctrl Pts',(-1.689758766469,-3.759883771183,-5.938186278284));
#46545=CARTESIAN_POINT('Ctrl Pts',(-2.980169377703,-2.847911715953,-5.98422794495));
#46546=CARTESIAN_POINT('Ctrl Pts',(-3.83266574011,-1.517459714869,-6.030269611617));
#46547=CARTESIAN_POINT('Ctrl Pts',(-4.121979703844,0.03597197191163,-6.076311278284));
#46548=CARTESIAN_POINT('Ctrl Pts',(-3.805598682858,1.584117838639,-6.12235294495));
#46549=CARTESIAN_POINT('Ctrl Pts',(-2.930012570708,2.899489092436,-6.168394611617));
#46550=CARTESIAN_POINT('Ctrl Pts',(-1.623882388293,3.788801479446,-6.214436278284));
#46551=CARTESIAN_POINT('Ctrl Pts',(-0.07913448113579,4.121377002357,-6.26047794495));
#46552=CARTESIAN_POINT('Ctrl Pts',(1.47724166337,3.848346103155,-6.306519611617));
#46553=CARTESIAN_POINT('Ctrl Pts',(2.816547872794,3.009828689797,-6.352561278284));
#46554=CARTESIAN_POINT('Ctrl Pts',(3.741982825359,1.729038807078,-6.39860294495));
#46555=CARTESIAN_POINT('Ctrl Pts',(4.117560575058,0.1941792274952,-6.444644611617));
#46556=CARTESIAN_POINT('Ctrl Pts',(3.888092698922,-1.369213579488,-6.490686278284));
#46557=CARTESIAN_POINT('Ctrl Pts',(3.087297835011,-2.731410393844,-6.53672794495));
#46558=CARTESIAN_POINT('Ctrl Pts',(1.832846973412,-3.692246285626,-6.582769611617));
#46559=CARTESIAN_POINT('Ctrl Pts',(0.3090725587339,-4.110533397882,-6.628811278284));
#46560=CARTESIAN_POINT('Ctrl Pts',(-1.260117824043,-3.924807476958,-6.67485294495));
#46561=CARTESIAN_POINT('Ctrl Pts',(-2.644143043235,-3.162359598245,-6.720894611617));
#46562=CARTESIAN_POINT('Ctrl Pts',(-3.639630643292,-1.935225940801,-6.766936278284));
#46563=CARTESIAN_POINT('Ctrl Pts',(-4.100300950458,-0.4237248845199,-6.81297794495));
#46564=CARTESIAN_POINT('Ctrl Pts',(-3.958461808006,1.150039466741,-6.859019611617));
#46565=CARTESIAN_POINT('Ctrl Pts',(-3.234955449255,2.554813868979,-6.905061278284));
#46566=CARTESIAN_POINT('Ctrl Pts',(-2.036095874727,3.584176928104,-6.95110294495));
#46567=CARTESIAN_POINT('Ctrl Pts',(-0.5380468116679,4.086871205575,-6.997144611617));
#46568=CARTESIAN_POINT('Ctrl Pts',(1.039064377895,3.98902947244,-7.043186278284));
#46569=CARTESIAN_POINT('Ctrl Pts',(2.463492398452,3.305028694111,-7.08922794495));
#46570=CARTESIAN_POINT('Ctrl Pts',(3.525928861993,2.135378440328,-7.135269611617));
#46571=CARTESIAN_POINT('Ctrl Pts',(4.070252841003,0.6519479993433,-7.181311278284));
#46572=CARTESIAN_POINT('Ctrl Pts',(4.016493331088,-0.9272746288775,-7.22735294495));
#46573=CARTESIAN_POINT('Ctrl Pts',(3.372499699855,-2.370266500001,-7.273394611617));
#46574=CARTESIAN_POINT('Ctrl Pts',(2.612892894131,-3.100001962842,-7.304089056061));
#46575=CARTESIAN_POINT('Ctrl Pts',(2.178308200468,-3.380072686139,-7.319436278284));
#46576=CARTESIAN_POINT('Ctrl Pts',(0.4830001770654,-3.823340089268,-4.469450245148));
#46577=CARTESIAN_POINT('Ctrl Pts',(-0.008576553896349,-3.885440672149,-4.48479746737));
#46578=CARTESIAN_POINT('Ctrl Pts',(-1.015768594638,-3.817642737768,-4.515491911815));
#46579=CARTESIAN_POINT('Ctrl Pts',(-2.377463978216,-3.154992073467,-4.561533578481));
#46580=CARTESIAN_POINT('Ctrl Pts',(-3.389763509381,-2.028732577009,-4.607575245148));
#46581=CARTESIAN_POINT('Ctrl Pts',(-3.903973908634,-0.604367076473,-4.653616911815));
#46582=CARTESIAN_POINT('Ctrl Pts',(-3.844520476228,0.908806183397,-4.699658578481));
#46583=CARTESIAN_POINT('Ctrl Pts',(-3.220143539338,2.288436865292,-4.745700245148));
#46584=CARTESIAN_POINT('Ctrl Pts',(-2.12258966234,3.331798397039,-4.791741911815));
#46585=CARTESIAN_POINT('Ctrl Pts',(-0.7131367100223,3.885576341192,-4.837783578481));
#46586=CARTESIAN_POINT('Ctrl Pts',(0.8011065197924,3.86839706016,-4.883825245148));
#46587=CARTESIAN_POINT('Ctrl Pts',(2.197632959513,3.282784921885,-4.929866911815));
#46588=CARTESIAN_POINT('Ctrl Pts',(3.27123319567,2.214791378231,-4.975908578481));
#46589=CARTESIAN_POINT('Ctrl Pts',(3.864149468261,0.8213503247539,-5.021950245148));
#46590=CARTESIAN_POINT('Ctrl Pts',(3.88925703704,-0.6927821944998,-5.067991911815));
#46591=CARTESIAN_POINT('Ctrl Pts',(3.342866526991,-2.105115401081,-5.114033578481));
#46592=CARTESIAN_POINT('Ctrl Pts',(2.305266055846,-3.208117186282,-5.160075245148));
#46593=CARTESIAN_POINT('Ctrl Pts',(0.9289234780445,-3.839709447483,-5.206116911815));
#46594=CARTESIAN_POINT('Ctrl Pts',(-0.5839176592511,-3.907084288362,-5.252158578481));
#46595=CARTESIAN_POINT('Ctrl Pts',(-2.01095633678,-3.400341465311,-5.298200245148));
#46596=CARTESIAN_POINT('Ctrl Pts',(-3.142499583669,-2.393943156341,-5.344241911815));
#46597=CARTESIAN_POINT('Ctrl Pts',(-3.812275336764,-1.035772284748,-5.390283578481));
#46598=CARTESIAN_POINT('Ctrl Pts',(-3.921864912888,0.474597802576,-5.436325245148));
#46599=CARTESIAN_POINT('Ctrl Pts',(-3.455164919641,1.915229189219,-5.482366911815));
#46600=CARTESIAN_POINT('Ctrl Pts',(-2.480753531974,3.07443155441,-5.528408578481));
#46601=CARTESIAN_POINT('Ctrl Pts',(-1.14181342738,3.781868528414,-5.574450245148));
#46602=CARTESIAN_POINT('Ctrl Pts',(0.3649078688106,3.933587385127,-5.620491911815));
#46603=CARTESIAN_POINT('Ctrl Pts',(1.818008603547,3.5072941403,-5.666533578481));
#46604=CARTESIAN_POINT('Ctrl Pts',(3.003966175905,2.565629490626,-5.712575245148));
#46605=CARTESIAN_POINT('Ctrl Pts',(3.748512732746,1.246964218249,-5.758616911815));
#46606=CARTESIAN_POINT('Ctrl Pts',(3.942242564249,-0.2549333908657,-5.804658578481));
#46607=CARTESIAN_POINT('Ctrl Pts',(3.55668847849,-1.719370389453,-5.850700245148));
#46608=CARTESIAN_POINT('Ctrl Pts',(2.648504848577,-2.931158394938,-5.896741911815));
#46609=CARTESIAN_POINT('Ctrl Pts',(1.351142663929,-3.712233959607,-5.942783578481));
#46610=CARTESIAN_POINT('Ctrl Pts',(-0.1447601235313,-3.947823701204,-5.988825245148));
#46611=CARTESIAN_POINT('Ctrl Pts',(-1.61939146205,-3.603309417992,-6.034866911815));
#46612=CARTESIAN_POINT('Ctrl Pts',(-2.856064984826,-2.729314982116,-6.080908578481));
#46613=CARTESIAN_POINT('Ctrl Pts',(-3.673060498094,-1.454267529204,-6.126950245148));
#46614=CARTESIAN_POINT('Ctrl Pts',(-3.95032644399,0.03447397660704,-6.172991911815));
#46615=CARTESIAN_POINT('Ctrl Pts',(-3.647120605201,1.518149781897,-6.219033578481));
#46616=CARTESIAN_POINT('Ctrl Pts',(-2.807996877932,2.778744501151,-6.265075245148));
#46617=CARTESIAN_POINT('Ctrl Pts',(-1.556258400404,3.631022894492,-6.311116911815));
#46618=CARTESIAN_POINT('Ctrl Pts',(-0.07583905208719,3.949748841044,-6.357158578481));
#46619=CARTESIAN_POINT('Ctrl Pts',(1.41572429421,3.688087877469,-6.403200245148));
#46620=CARTESIAN_POINT('Ctrl Pts',(2.699257236101,2.884489182249,-6.449241911815));
#46621=CARTESIAN_POINT('Ctrl Pts',(3.58615392846,1.657035748118,-6.495283578481));
#46622=CARTESIAN_POINT('Ctrl Pts',(3.946091342763,0.1860929437699,-6.541325245148));
#46623=CARTESIAN_POINT('Ctrl Pts',(3.726179289751,-1.312194867306,-6.587366911815));
#46624=CARTESIAN_POINT('Ctrl Pts',(2.958732248669,-2.617665171454,-6.633408578481));
#46625=CARTESIAN_POINT('Ctrl Pts',(1.7565209892,-3.53848858747,-6.679450245148));
#46626=CARTESIAN_POINT('Ctrl Pts',(0.2962017257726,-3.939356801155,-6.725491911815));
#46627=CARTESIAN_POINT('Ctrl Pts',(-1.207642230314,-3.761365139508,-6.771533578481));
#46628=CARTESIAN_POINT('Ctrl Pts',(-2.53403193025,-3.030668184684,-6.817575245148));
#46629=CARTESIAN_POINT('Ctrl Pts',(-3.488064039506,-1.854636548043,-6.863616911815));
#46630=CARTESIAN_POINT('Ctrl Pts',(-3.929550467657,-0.4060795386098,-6.909658578481));
#46631=CARTESIAN_POINT('Ctrl Pts',(-3.793617989703,1.102147910351,-6.955700245148));
#46632=CARTESIAN_POINT('Ctrl Pts',(-3.100240897452,2.448422726752,-7.001741911815));
#46633=CARTESIAN_POINT('Ctrl Pts',(-1.951305914712,3.434919605699,-7.047783578481));
#46634=CARTESIAN_POINT('Ctrl Pts',(-0.5156407117324,3.916679983045,-7.093825245148));
#46635=CARTESIAN_POINT('Ctrl Pts',(0.9957942017955,3.822912712584,-7.139866911815));
#46636=CARTESIAN_POINT('Ctrl Pts',(2.360904192978,3.167396053969,-7.185908578481));
#46637=CARTESIAN_POINT('Ctrl Pts',(3.37909718725,2.046454016474,-7.231950245148));
#46638=CARTESIAN_POINT('Ctrl Pts',(3.900753663718,0.6247986664056,-7.277991911815));
#46639=CARTESIAN_POINT('Ctrl Pts',(3.849232882712,-0.8886597582904,-7.324033578481));
#46640=CARTESIAN_POINT('Ctrl Pts',(3.232057337464,-2.271560538139,-7.370075245148));
#46641=CARTESIAN_POINT('Ctrl Pts',(2.504083143683,-2.97090733339,-7.400769689593));
#46642=CARTESIAN_POINT('Ctrl Pts',(2.087596035333,-3.239314958832,-7.416116911815));
#46643=CARTESIAN_POINT('Ctrl Pts',(0.4620124040095,-3.657204758643,-4.566130878679));
#46644=CARTESIAN_POINT('Ctrl Pts',(-0.008203877497198,-3.716606889221,-4.581478100901));
#46645=CARTESIAN_POINT('Ctrl Pts',(-0.9716304726375,-3.65175497376,-4.612172545346));
#46646=CARTESIAN_POINT('Ctrl Pts',(-2.274156201548,-3.017898422626,-4.658214212012));
#46647=CARTESIAN_POINT('Ctrl Pts',(-3.242468351686,-1.94057820163,-4.704255878679));
#46648=CARTESIAN_POINT('Ctrl Pts',(-3.734334802272,-0.5781055559897,-4.750297545346));
#46649=CARTESIAN_POINT('Ctrl Pts',(-3.677464795723,0.8693158916029,-4.796339212012));
#46650=CARTESIAN_POINT('Ctrl Pts',(-3.080218866387,2.188997577561,-4.842380878679));
#46651=CARTESIAN_POINT('Ctrl Pts',(-2.030356921569,3.187021993332,-4.888422545346));
#46652=CARTESIAN_POINT('Ctrl Pts',(-0.6821488302275,3.716736663046,-4.934464212013));
#46653=CARTESIAN_POINT('Ctrl Pts',(0.7662960939803,3.700303872116,-4.980505878679));
#46654=CARTESIAN_POINT('Ctrl Pts',(2.102139367575,3.140138297301,-5.026547545346));
#46655=CARTESIAN_POINT('Ctrl Pts',(3.129088527441,2.11855220272,-5.072589212013));
#46656=CARTESIAN_POINT('Ctrl Pts',(3.696240850532,0.7856602462946,-5.118630878679));
#46657=CARTESIAN_POINT('Ctrl Pts',(3.720257421874,-0.6626787780505,-5.164672545346));
#46658=CARTESIAN_POINT('Ctrl Pts',(3.197609180605,-2.013641968167,-5.210714212013));
#46659=CARTESIAN_POINT('Ctrl Pts',(2.20509549047,-3.068715093613,-5.256755878679));
#46660=CARTESIAN_POINT('Ctrl Pts',(0.8885590308471,-3.672862820275,-5.302797545346));
#46661=CARTESIAN_POINT('Ctrl Pts',(-0.5585447258702,-3.737310026886,-5.348839212013));
#46662=CARTESIAN_POINT('Ctrl Pts',(-1.92357439113,-3.252586664433,-5.394880878679));
#46663=CARTESIAN_POINT('Ctrl Pts',(-3.005948768117,-2.289919311093,-5.440922545346));
#46664=CARTESIAN_POINT('Ctrl Pts',(-3.646620802058,-0.9907649437943,-5.486964212013));
#46665=CARTESIAN_POINT('Ctrl Pts',(-3.751448389963,0.4539751373136,-5.533005878679));
#46666=CARTESIAN_POINT('Ctrl Pts',(-3.30502787902,1.832006868644,-5.579047545346));
#46667=CARTESIAN_POINT('Ctrl Pts',(-2.372957521519,2.940838494192,-5.625089212013));
#46668=CARTESIAN_POINT('Ctrl Pts',(-1.092198288041,3.617535258634,-5.671130878679));
#46669=CARTESIAN_POINT('Ctrl Pts',(0.3490515526009,3.762661486433,-5.717172545346));
#46670=CARTESIAN_POINT('Ctrl Pts',(1.739010802311,3.354891932284,-5.763214212013));
#46671=CARTESIAN_POINT('Ctrl Pts',(2.873435042872,2.454145371051,-5.809255878679));
#46672=CARTESIAN_POINT('Ctrl Pts',(3.585628870032,1.192779968917,-5.855297545346));
#46673=CARTESIAN_POINT('Ctrl Pts',(3.770940572659,-0.2438557879871,-5.901339212013));
#46674=CARTESIAN_POINT('Ctrl Pts',(3.402139941737,-1.644658707665,-5.947380878679));
#46675=CARTESIAN_POINT('Ctrl Pts',(2.533419551845,-2.803790973341,-5.993422545346));
#46676=CARTESIAN_POINT('Ctrl Pts',(1.292431555853,-3.550926515896,-6.039464212013));
#46677=CARTESIAN_POINT('Ctrl Pts',(-0.1384698719652,-3.776279192858,-6.085505878679));
#46678=CARTESIAN_POINT('Ctrl Pts',(-1.549024157631,-3.446735064802,-6.131547545346));
#46679=CARTESIAN_POINT('Ctrl Pts',(-2.731960591949,-2.610718248279,-6.177589212013));
#46680=CARTESIAN_POINT('Ctrl Pts',(-3.513455256077,-1.391075343539,-6.223630878679));
#46681=CARTESIAN_POINT('Ctrl Pts',(-3.778673184137,0.03297598130244,-6.269672545346));
#46682=CARTESIAN_POINT('Ctrl Pts',(-3.488642527544,1.452181725154,-6.315714212013));
#46683=CARTESIAN_POINT('Ctrl Pts',(-2.685981185156,2.657999909866,-6.361755878679));
#46684=CARTESIAN_POINT('Ctrl Pts',(-1.488634412516,3.473244309537,-6.407797545346));
#46685=CARTESIAN_POINT('Ctrl Pts',(-0.07254362303861,3.778120679731,-6.453839212012));
#46686=CARTESIAN_POINT('Ctrl Pts',(1.354206925051,3.527829651783,-6.499880878679));
#46687=CARTESIAN_POINT('Ctrl Pts',(2.581966599408,2.7591496747,-6.545922545346));
#46688=CARTESIAN_POINT('Ctrl Pts',(3.430325031562,1.585032689158,-6.591964212013));
#46689=CARTESIAN_POINT('Ctrl Pts',(3.774622110468,0.1780066600445,-6.638005878679));
#46690=CARTESIAN_POINT('Ctrl Pts',(3.56426588058,-1.255176155123,-6.684047545346));
#46691=CARTESIAN_POINT('Ctrl Pts',(2.830166662326,-2.503919949063,-6.730089212013));
#46692=CARTESIAN_POINT('Ctrl Pts',(1.680195004987,-3.384730889313,-6.776130878679));
#46693=CARTESIAN_POINT('Ctrl Pts',(0.2833308928114,-3.768180204427,-6.822172545346));
#46694=CARTESIAN_POINT('Ctrl Pts',(-1.155166636586,-3.597922802058,-6.868214212013));
#46695=CARTESIAN_POINT('Ctrl Pts',(-2.423920817265,-2.898976771123,-6.914255878679));
#46696=CARTESIAN_POINT('Ctrl Pts',(-3.336497435721,-1.774047155286,-6.960297545346));
#46697=CARTESIAN_POINT('Ctrl Pts',(-3.758799984856,-0.3884341926996,-7.006339212013));
#46698=CARTESIAN_POINT('Ctrl Pts',(-3.6287741714,1.054256353961,-7.052380878679));
#46699=CARTESIAN_POINT('Ctrl Pts',(-2.965526345649,2.342031584525,-7.098422545346));
#46700=CARTESIAN_POINT('Ctrl Pts',(-1.866515954698,3.285662283295,-7.144464212013));
#46701=CARTESIAN_POINT('Ctrl Pts',(-0.4932346117968,3.746488760516,-7.190505878679));
#46702=CARTESIAN_POINT('Ctrl Pts',(0.9525240256962,3.656795952728,-7.236547545346));
#46703=CARTESIAN_POINT('Ctrl Pts',(2.258315987503,3.029763413827,-7.282589212013));
#46704=CARTESIAN_POINT('Ctrl Pts',(3.232265512507,1.957529592619,-7.328630878679));
#46705=CARTESIAN_POINT('Ctrl Pts',(3.731254486433,0.5976493334679,-7.374672545346));
#46706=CARTESIAN_POINT('Ctrl Pts',(3.681972434336,-0.8500448877034,-7.420714212013));
#46707=CARTESIAN_POINT('Ctrl Pts',(3.091614975073,-2.172854576276,-7.466755878679));
#46708=CARTESIAN_POINT('Ctrl Pts',(2.395273393235,-2.841812703939,-7.497450323124));
#46709=CARTESIAN_POINT('Ctrl Pts',(1.996883870199,-3.098557231525,-7.512797545346));
#46710=CARTESIAN_POINT('Ctrl Pts',(0.4410246309536,-3.491069428017,-4.66281151221));
#46711=CARTESIAN_POINT('Ctrl Pts',(-0.007831201098047,-3.547773106292,-4.678158734432));
#46712=CARTESIAN_POINT('Ctrl Pts',(-0.9274923506371,-3.485867209753,-4.708853178877));
#46713=CARTESIAN_POINT('Ctrl Pts',(-2.170848424879,-2.880804771784,-4.754894845544));
#46714=CARTESIAN_POINT('Ctrl Pts',(-3.09517319399,-1.85242382625,-4.80093651221));
#46715=CARTESIAN_POINT('Ctrl Pts',(-3.564695695909,-0.5518440355064,-4.846978178877));
#46716=CARTESIAN_POINT('Ctrl Pts',(-3.510409115218,0.8298255998088,-4.893019845544));
#46717=CARTESIAN_POINT('Ctrl Pts',(-2.940294193437,2.08955828983,-4.93906151221));
#46718=CARTESIAN_POINT('Ctrl Pts',(-1.938124180797,3.042245589626,-4.985103178877));
#46719=CARTESIAN_POINT('Ctrl Pts',(-0.6511609504327,3.5478969849,-5.031144845544));
#46720=CARTESIAN_POINT('Ctrl Pts',(0.7314856681681,3.532210684072,-5.07718651221));
#46721=CARTESIAN_POINT('Ctrl Pts',(2.006645775638,2.997491672717,-5.123228178877));
#46722=CARTESIAN_POINT('Ctrl Pts',(2.986943859211,2.022313027209,-5.169269845544));
#46723=CARTESIAN_POINT('Ctrl Pts',(3.528332232803,0.7499701678353,-5.21531151221));
#46724=CARTESIAN_POINT('Ctrl Pts',(3.551257806707,-0.6325753616011,-5.261353178877));
#46725=CARTESIAN_POINT('Ctrl Pts',(3.052351834218,-1.922168535253,-5.307394845544));
#46726=CARTESIAN_POINT('Ctrl Pts',(2.104924925093,-2.929313000944,-5.35343651221));
#46727=CARTESIAN_POINT('Ctrl Pts',(0.8481945836498,-3.506016193067,-5.399478178877));
#46728=CARTESIAN_POINT('Ctrl Pts',(-0.5331717924892,-3.567535765409,-5.445519845544));
#46729=CARTESIAN_POINT('Ctrl Pts',(-1.836192445479,-3.104831863555,-5.49156151221));
#46730=CARTESIAN_POINT('Ctrl Pts',(-2.869397952564,-2.185895465844,-5.537603178877));
#46731=CARTESIAN_POINT('Ctrl Pts',(-3.480966267353,-0.9457576028406,-5.583644845544));
#46732=CARTESIAN_POINT('Ctrl Pts',(-3.581031867039,0.4333524720513,-5.62968651221));
#46733=CARTESIAN_POINT('Ctrl Pts',(-3.154890838399,1.74878454807,-5.675728178877));
#46734=CARTESIAN_POINT('Ctrl Pts',(-2.265161511065,2.807245433975,-5.721769845544));
#46735=CARTESIAN_POINT('Ctrl Pts',(-1.042583148702,3.453201988854,-5.76781151221));
#46736=CARTESIAN_POINT('Ctrl Pts',(0.3331952363912,3.591735587738,-5.813853178877));
#46737=CARTESIAN_POINT('Ctrl Pts',(1.660013001075,3.202489724268,-5.859894845544));
#46738=CARTESIAN_POINT('Ctrl Pts',(2.742903909839,2.342661251476,-5.90593651221));
#46739=CARTESIAN_POINT('Ctrl Pts',(3.422745007318,1.138595719585,-5.951978178877));
#46740=CARTESIAN_POINT('Ctrl Pts',(3.599638581068,-0.2327781851084,-5.998019845544));
#46741=CARTESIAN_POINT('Ctrl Pts',(3.247591404983,-1.569947025876,-6.04406151221));
#46742=CARTESIAN_POINT('Ctrl Pts',(2.418334255113,-2.676423551744,-6.090103178877));
#46743=CARTESIAN_POINT('Ctrl Pts',(1.233720447776,-3.389619072185,-6.136144845544));
#46744=CARTESIAN_POINT('Ctrl Pts',(-0.1321796203991,-3.604734684513,-6.18218651221));
#46745=CARTESIAN_POINT('Ctrl Pts',(-1.478656853211,-3.290160711611,-6.228228178877));
#46746=CARTESIAN_POINT('Ctrl Pts',(-2.607856199071,-2.492121514442,-6.274269845544));
#46747=CARTESIAN_POINT('Ctrl Pts',(-3.353850014061,-1.327883157873,-6.32031151221));
#46748=CARTESIAN_POINT('Ctrl Pts',(-3.607019924283,0.03147798599784,-6.366353178877));
#46749=CARTESIAN_POINT('Ctrl Pts',(-3.330164449886,1.386213668412,-6.412394845544));
#46750=CARTESIAN_POINT('Ctrl Pts',(-2.563965492379,2.537255318581,-6.45843651221));
#46751=CARTESIAN_POINT('Ctrl Pts',(-1.421010424628,3.315465724582,-6.504478178877));
#46752=CARTESIAN_POINT('Ctrl Pts',(-0.06924819399001,3.606492518418,-6.550519845544));
#46753=CARTESIAN_POINT('Ctrl Pts',(1.292689555892,3.367571426097,-6.59656151221));
#46754=CARTESIAN_POINT('Ctrl Pts',(2.464675962715,2.633810167152,-6.642603178877));
#46755=CARTESIAN_POINT('Ctrl Pts',(3.274496134663,1.513029630198,-6.688644845544));
#46756=CARTESIAN_POINT('Ctrl Pts',(3.603152878174,0.1699203763192,-6.73468651221));
#46757=CARTESIAN_POINT('Ctrl Pts',(3.402352471409,-1.198157442941,-6.780728178877));
#46758=CARTESIAN_POINT('Ctrl Pts',(2.701601075983,-2.390174726673,-6.826769845544));
#46759=CARTESIAN_POINT('Ctrl Pts',(1.603869020775,-3.230973191157,-6.87281151221));
#46760=CARTESIAN_POINT('Ctrl Pts',(0.2704600598501,-3.5970036077,-6.918853178877));
#46761=CARTESIAN_POINT('Ctrl Pts',(-1.102691042857,-3.434480464608,-6.964894845544));
#46762=CARTESIAN_POINT('Ctrl Pts',(-2.313809704281,-2.767285357563,-7.01093651221));
#46763=CARTESIAN_POINT('Ctrl Pts',(-3.184930831936,-1.693457762528,-7.056978178877));
#46764=CARTESIAN_POINT('Ctrl Pts',(-3.588049502055,-0.3707888467895,-7.103019845544));
#46765=CARTESIAN_POINT('Ctrl Pts',(-3.463930353097,1.00636479757,-7.14906151221));
#46766=CARTESIAN_POINT('Ctrl Pts',(-2.830811793846,2.235640442297,-7.195103178877));
#46767=CARTESIAN_POINT('Ctrl Pts',(-1.781725994683,3.136404960891,-7.241144845544));
#46768=CARTESIAN_POINT('Ctrl Pts',(-0.4708285118613,3.576297537987,-7.28718651221));
#46769=CARTESIAN_POINT('Ctrl Pts',(0.9092538495968,3.490679192871,-7.333228178877));
#46770=CARTESIAN_POINT('Ctrl Pts',(2.155727782029,2.892130773684,-7.379269845544));
#46771=CARTESIAN_POINT('Ctrl Pts',(3.085433837764,1.868605168765,-7.42531151221));
#46772=CARTESIAN_POINT('Ctrl Pts',(3.561755309148,0.5705000005301,-7.471353178877));
#46773=CARTESIAN_POINT('Ctrl Pts',(3.514711985961,-0.8114300171164,-7.517394845544));
#46774=CARTESIAN_POINT('Ctrl Pts',(2.951172612682,-2.074148614413,-7.56343651221));
#46775=CARTESIAN_POINT('Ctrl Pts',(2.286463642788,-2.712718074487,-7.594130956655));
#46776=CARTESIAN_POINT('Ctrl Pts',(1.906171705064,-2.957799504219,-7.609478178877));
#46777=CARTESIAN_POINT('',(-1.36802931223802,-3.75862971277667,-4.44175420669655));
#46778=CARTESIAN_POINT('',(-1.36802935610884,-3.75862969680846,-5.19157912663668));
#46779=CARTESIAN_POINT('Ctrl Pts',(-1.36802039437616,-3.75860055108868,
-4.4417004147709));
#46780=CARTESIAN_POINT('Ctrl Pts',(-1.54934259720315,-3.69255062029612,
-4.44743516912771));
#46781=CARTESIAN_POINT('Ctrl Pts',(-1.72591270644782,-3.6134218564521,-4.45314749519308));
#46782=CARTESIAN_POINT('Ctrl Pts',(-2.06238627200896,-3.43244958138755,
-4.46452909116531));
#46783=CARTESIAN_POINT('Ctrl Pts',(-2.22197510880567,-3.33140913413749,
-4.47020811100648));
#46784=CARTESIAN_POINT('Ctrl Pts',(-2.67039775514929,-3.00061382058344,
-4.48693544612448));
#46785=CARTESIAN_POINT('Ctrl Pts',(-2.93619045066687,-2.74087836244429,
-4.49776118719158));
#46786=CARTESIAN_POINT('Ctrl Pts',(-3.32094587933198,-2.24473313507897,
-4.51652534385179));
#46787=CARTESIAN_POINT('Ctrl Pts',(-3.45938490375627,-2.02471873790244,
-4.52434738236671));
#46788=CARTESIAN_POINT('Ctrl Pts',(-3.68290281614523,-1.57848021809534,
-4.53919298992134));
#46789=CARTESIAN_POINT('Ctrl Pts',(-3.77092815157509,-1.35492446506356,
-4.54626688100694));
#46790=CARTESIAN_POINT('Ctrl Pts',(-3.9111203086744,-0.877355368442583,
-4.56112310443606));
#46791=CARTESIAN_POINT('Ctrl Pts',(-3.95946409788148,-0.623612474524625,
-4.56890506844228));
#46792=CARTESIAN_POINT('Ctrl Pts',(-4.00582222878401,-0.117779763933944,
-4.5840291674816));
#46793=CARTESIAN_POINT('Ctrl Pts',(-4.00537282225662,0.132956592148152,
-4.59140521803478));
#46794=CARTESIAN_POINT('Ctrl Pts',(-3.95717640564138,0.637870792459528,
-4.60653661088045));
#46795=CARTESIAN_POINT('Ctrl Pts',(-3.90804180281148,0.890569392092889,
-4.61429431867432));
#46796=CARTESIAN_POINT('Ctrl Pts',(-3.76233568622444,1.38119307228273,-4.62954027014657));
#46797=CARTESIAN_POINT('Ctrl Pts',(-3.66671564796724,1.61808381901511,-4.6370525954201));
#46798=CARTESIAN_POINT('Ctrl Pts',(-3.44683563797407,2.04174570453694,-4.65128932926735));
#46799=CARTESIAN_POINT('Ctrl Pts',(-3.32795075461521,2.23030869406375,-4.65801151888381));
#46800=CARTESIAN_POINT('Ctrl Pts',(-3.11488696706555,2.51264969004533,-4.66857772675018));
#46801=CARTESIAN_POINT('Ctrl Pts',(-3.03104639549336,2.61309949615091,-4.67245981466471));
#46802=CARTESIAN_POINT('Ctrl Pts',(-2.76702348189746,2.89980230975733,-4.68402679092864));
#46803=CARTESIAN_POINT('Ctrl Pts',(-2.57297416693329,3.07355090652908,-4.69171991493211));
#46804=CARTESIAN_POINT('Ctrl Pts',(-2.15293080174829,3.381235303862,-4.70737436130896));
#46805=CARTESIAN_POINT('Ctrl Pts',(-1.92789479525138,3.51419071409789,-4.71514797546484));
#46806=CARTESIAN_POINT('Ctrl Pts',(-1.45736426369289,3.73380167561811,-4.7305573131301));
#46807=CARTESIAN_POINT('Ctrl Pts',(-1.21209415691628,3.82069058044626,-4.73824828416753));
#46808=CARTESIAN_POINT('Ctrl Pts',(-0.707017424571773,3.94561402719561,
-4.7538939255643));
#46809=CARTESIAN_POINT('Ctrl Pts',(-0.448488883432865,3.98309040011465,
-4.76165606365684));
#46810=CARTESIAN_POINT('Ctrl Pts',(0.336804092028381,4.02011287173604,-4.78498496689132));
#46811=CARTESIAN_POINT('Ctrl Pts',(0.859994522360031,3.94156082988392,-4.80064435867064));
#46812=CARTESIAN_POINT('Ctrl Pts',(1.85025226377309,3.5849168365716,-4.83187570141402));
#46813=CARTESIAN_POINT('Ctrl Pts',(2.30357138893829,3.31188808767728,-4.84753994308384));
#46814=CARTESIAN_POINT('Ctrl Pts',(3.08187051358349,2.6033735312351,-4.87877043664423));
#46815=CARTESIAN_POINT('Ctrl Pts',(3.39594107651066,2.17767785925985,-4.89442864532868));
#46816=CARTESIAN_POINT('Ctrl Pts',(3.73051023029279,1.4661277116197,-4.9177611077362));
#46817=CARTESIAN_POINT('Ctrl Pts',(3.81832167123335,1.21993708328814,-4.92552839839978));
#46818=CARTESIAN_POINT('Ctrl Pts',(3.94409941527293,0.714821941134461,-4.94118109301224));
#46819=CARTESIAN_POINT('Ctrl Pts',(3.98197372209973,0.457289881862814,-4.94887423797372));
#46820=CARTESIAN_POINT('Ctrl Pts',(4.00781859492935,-0.0615669812030529,
-4.96429090075327));
#46821=CARTESIAN_POINT('Ctrl Pts',(3.9954657396674,-0.322795341644,-4.97206975219878));
#46822=CARTESIAN_POINT('Ctrl Pts',(3.91975475474618,-0.838118779766908,
-4.98772905643859));
#46823=CARTESIAN_POINT('Ctrl Pts',(3.85683682656876,-1.0909152128301,-4.99542255647908));
#46824=CARTESIAN_POINT('Ctrl Pts',(3.72674843469839,-1.45838615776341,-5.00699162303596));
#46825=CARTESIAN_POINT('Ctrl Pts',(3.67711659488106,-1.57948047247824,-5.01087475438419));
#46826=CARTESIAN_POINT('Ctrl Pts',(3.5273237750208,-1.89927756380344,-5.02142463741197));
#46827=CARTESIAN_POINT('Ctrl Pts',(3.41652238300875,-2.09200988761366,-5.02812865740639));
#46828=CARTESIAN_POINT('Ctrl Pts',(3.14470166249094,-2.48482176617446,-5.04237602217406));
#46829=CARTESIAN_POINT('Ctrl Pts',(2.97934589921149,-2.68083227463917,-5.04991664274165));
#46830=CARTESIAN_POINT('Ctrl Pts',(2.61316026267878,-3.0392638165989,-5.06518203670961));
#46831=CARTESIAN_POINT('Ctrl Pts',(2.41298178294807,-3.20053828557141,-5.07292901109072));
#46832=CARTESIAN_POINT('Ctrl Pts',(1.98803127630066,-3.47983381113735,-5.08809851764534));
#46833=CARTESIAN_POINT('Ctrl Pts',(1.76500032892612,-3.59806928254064,-5.09552353347747));
#46834=CARTESIAN_POINT('Ctrl Pts',(1.29476897682159,-3.79336432465765,-5.11068617323473));
#46835=CARTESIAN_POINT('Ctrl Pts',(1.04821759264496,-3.86879850787193,-5.11845440852111));
#46836=CARTESIAN_POINT('Ctrl Pts',(0.443462743860844,-3.99128966747531,
-5.13686839940374));
#46837=CARTESIAN_POINT('Ctrl Pts',(0.0815921899009596,-4.01521472860259,
-5.14744800540222));
#46838=CARTESIAN_POINT('Ctrl Pts',(-0.46156966433257,-3.97754005871251,
-5.16380287393384));
#46839=CARTESIAN_POINT('Ctrl Pts',(-0.644462573517245,-3.95198255439727,
-5.16934980978426));
#46840=CARTESIAN_POINT('Ctrl Pts',(-1.0095357189814,-3.87487188232507,-5.18046212852935));
#46841=CARTESIAN_POINT('Ctrl Pts',(-1.19104591981548,-3.8229612527995,-5.18603683717925));
#46842=CARTESIAN_POINT('Ctrl Pts',(-1.36801744281564,-3.75860162536828,
-5.1916329185624));
#46843=CARTESIAN_POINT('Ctrl Pts',(-1.3680167762483,-3.75859993758318,-5.19163396445895));
#46844=CARTESIAN_POINT('Ctrl Pts',(-1.52459617763929,-3.70157102288258,
-5.19663239427401));
#46845=CARTESIAN_POINT('Ctrl Pts',(-1.67763499677768,-3.63478957023376,
-5.20164763837071));
#46846=CARTESIAN_POINT('Ctrl Pts',(-1.9724037483695,-3.48366095352311,-5.21156248080557));
#46847=CARTESIAN_POINT('Ctrl Pts',(-2.11391003538115,-3.39971150035342,
-5.21643325110857));
#46848=CARTESIAN_POINT('Ctrl Pts',(-2.51519738783286,-3.12668384635704,
-5.23079642370571));
#46849=CARTESIAN_POINT('Ctrl Pts',(-2.75776227640788,-2.91461075882842,
-5.24042285890803));
#46850=CARTESIAN_POINT('Ctrl Pts',(-3.11317232084341,-2.52027193308931,
-5.25633917223062));
#46851=CARTESIAN_POINT('Ctrl Pts',(-3.24179690154522,-2.35266091526733,
-5.26258710786489));
#46852=CARTESIAN_POINT('Ctrl Pts',(-3.49709704348102,-1.95866745942865,
-5.27648832154417));
#46853=CARTESIAN_POINT('Ctrl Pts',(-3.61609130191531,-1.72870855025888,
-5.28422785733577));
#46854=CARTESIAN_POINT('Ctrl Pts',(-3.80627593895292,-1.25493784223009,
-5.29955595510452));
#46855=CARTESIAN_POINT('Ctrl Pts',(-3.8781817538229,-1.01169864197555,-5.30707268198896));
#46856=CARTESIAN_POINT('Ctrl Pts',(-3.97577832395145,-0.509299016663343,
-5.32222423663731));
#46857=CARTESIAN_POINT('Ctrl Pts',(-4.00018647090875,-0.251353389346759,
-5.32996516501829));
#46858=CARTESIAN_POINT('Ctrl Pts',(-3.99941282800716,0.259916502965717,
-5.34531669247299));
#46859=CARTESIAN_POINT('Ctrl Pts',(-3.97504126814118,0.512996707439322,
-5.35285546694779));
#46860=CARTESIAN_POINT('Ctrl Pts',(-3.85237700186971,1.14468907468732,-5.37190443323698));
#46861=CARTESIAN_POINT('Ctrl Pts',(-3.72197755324421,1.51518481176753,-5.38367582700348));
#46862=CARTESIAN_POINT('Ctrl Pts',(-3.42171503308643,2.08767016397984,-5.40294896079497));
#46863=CARTESIAN_POINT('Ctrl Pts',(-3.28008651051313,2.30373402361474,-5.41050564496186));
#46864=CARTESIAN_POINT('Ctrl Pts',(-2.95281280124014,2.71086590418969,-5.42613976962702));
#46865=CARTESIAN_POINT('Ctrl Pts',(-2.76702159128311,2.90033262756753,-5.43411158232797));
#46866=CARTESIAN_POINT('Ctrl Pts',(-2.46652560831014,3.15151482798791,-5.44577942231872));
#46867=CARTESIAN_POINT('Ctrl Pts',(-2.36491747442529,3.22846771183613,-5.4495401120054));
#46868=CARTESIAN_POINT('Ctrl Pts',(-1.94381052700404,3.51674079037441,-5.46465273838207));
#46869=CARTESIAN_POINT('Ctrl Pts',(-1.59724890420419,3.68683278071615,-5.4762334902682));
#46870=CARTESIAN_POINT('Ctrl Pts',(-1.11260713984251,3.84421077592591,-5.49142073137437));
#46871=CARTESIAN_POINT('Ctrl Pts',(-0.989346965118392,3.87777061807205,
-5.49519140977438));
#46872=CARTESIAN_POINT('Ctrl Pts',(-0.48788725002256,3.98875297609574,-5.51039798290914));
#46873=CARTESIAN_POINT('Ctrl Pts',(-0.0998840500225523,4.01698241598383,
-5.52206340540215));
#46874=CARTESIAN_POINT('Ctrl Pts',(0.541553511551181,3.9715669702806,-5.54123186334516));
#46875=CARTESIAN_POINT('Ctrl Pts',(0.796495603625449,3.92833974663983,-5.54879644134867));
#46876=CARTESIAN_POINT('Ctrl Pts',(1.3008289479688,3.79153197552046,-5.56443837277499));
#46877=CARTESIAN_POINT('Ctrl Pts',(1.54882785835396,3.69722503234154,-5.57240883341697));
#46878=CARTESIAN_POINT('Ctrl Pts',(1.89921194033021,3.52260745940935,-5.58406949732348));
#46879=CARTESIAN_POINT('Ctrl Pts',(2.01032628479411,3.46040397279558,-5.58782611686486));
#46880=CARTESIAN_POINT('Ctrl Pts',(2.44205040257394,3.19081613267549,-5.60290025125967));
#46881=CARTESIAN_POINT('Ctrl Pts',(2.73594967962277,2.94238494043527,-5.61444615201412));
#46882=CARTESIAN_POINT('Ctrl Pts',(3.07387903455474,2.56263769339478,-5.62959619280945));
#46883=CARTESIAN_POINT('Ctrl Pts',(3.15408797273173,2.46325642878526,-5.63336560536742));
#46884=CARTESIAN_POINT('Ctrl Pts',(3.38181256332884,2.15160932363914,-5.64479408180919));
#46885=CARTESIAN_POINT('Ctrl Pts',(3.51351655055612,1.9286688339332,-5.65253364414412));
#46886=CARTESIAN_POINT('Ctrl Pts',(3.72998420409793,1.4662368945807,-5.66786396860653));
#46887=CARTESIAN_POINT('Ctrl Pts',(3.81542441089416,1.22735248319645,-5.67538288269108));
#46888=CARTESIAN_POINT('Ctrl Pts',(3.94102102926835,0.731136667957038,-5.69053657193643));
#46889=CARTESIAN_POINT('Ctrl Pts',(3.97983677196199,0.474949937533666,-5.69827764011206));
#46890=CARTESIAN_POINT('Ctrl Pts',(4.00769347520972,-0.0356116245477114,
-5.71363073144215));
#46891=CARTESIAN_POINT('Ctrl Pts',(3.9975257069734,-0.289698829082997,-5.72117093343997));
#46892=CARTESIAN_POINT('Ctrl Pts',(3.92812752775653,-0.797572025267891,
-5.73634483642131));
#46893=CARTESIAN_POINT('Ctrl Pts',(3.86816682449722,-1.04978870033432,-5.74408698466635));
#46894=CARTESIAN_POINT('Ctrl Pts',(3.70261992673624,-1.53416648463589,-5.75945760919759));
#46895=CARTESIAN_POINT('Ctrl Pts',(3.59782540191802,-1.76635316566549,-5.76701419549071));
#46896=CARTESIAN_POINT('Ctrl Pts',(3.34287429023877,-2.21169068286263,-5.78220371996438));
#46897=CARTESIAN_POINT('Ctrl Pts',(3.19268979435998,-2.42313361991924,-5.7899466526353));
#46898=CARTESIAN_POINT('Ctrl Pts',(2.85735490357643,-2.81046749263772,-5.80533084590177));
#46899=CARTESIAN_POINT('Ctrl Pts',(2.67289578558032,-2.98666099838215,-5.81290010971133));
#46900=CARTESIAN_POINT('Ctrl Pts',(2.1642681873338,-3.38662787238639,-5.83205224148432));
#46901=CARTESIAN_POINT('Ctrl Pts',(1.82075453294885,-3.58271215277965,-5.84390150196588));
#46902=CARTESIAN_POINT('Ctrl Pts',(1.21643196960817,-3.81925402722105,-5.86325194063489));
#46903=CARTESIAN_POINT('Ctrl Pts',(0.968030972362526,-3.88960136599096,
-5.87080284188523));
#46904=CARTESIAN_POINT('Ctrl Pts',(0.454171773558271,-3.98266811030524,
-5.8864311843829));
#46905=CARTESIAN_POINT('Ctrl Pts',(0.189647694887073,-4.00404421823235,
-5.8944039810315));
#46906=CARTESIAN_POINT('Ctrl Pts',(-0.3334185648329,-3.99446656653653,-5.90999161466257));
#46907=CARTESIAN_POINT('Ctrl Pts',(-0.590853825580882,-3.96451728937445,
-5.91757656825456));
#46908=CARTESIAN_POINT('Ctrl Pts',(-1.10209122846833,-3.85398501839706,
-5.93323826433512));
#46909=CARTESIAN_POINT('Ctrl Pts',(-1.35457594056273,-3.77272824853405,
-5.94120524380203));
#46910=CARTESIAN_POINT('Ctrl Pts',(-1.77075753827486,-3.59168027698949,
-5.95471659289937));
#46911=CARTESIAN_POINT('Ctrl Pts',(-1.93915946751059,-3.50362800106389,
-5.96029162353956));
#46912=CARTESIAN_POINT('Ctrl Pts',(-2.21205485324292,-3.33508683258783,
-5.96984947866373));
#46913=CARTESIAN_POINT('Ctrl Pts',(-2.31990375583759,-3.26092839606414,
-5.9737702070383));
#46914=CARTESIAN_POINT('Ctrl Pts',(-2.6301565877348,-3.02452409995926,-5.98548165134658));
#46915=CARTESIAN_POINT('Ctrl Pts',(-2.82134464511646,-2.84728377151697,
-5.9932720609891));
#46916=CARTESIAN_POINT('Ctrl Pts',(-3.16682767687751,-2.45742090293799,
-6.00869433715144));
#46917=CARTESIAN_POINT('Ctrl Pts',(-3.32004506728904,-2.24581849689792,
-6.01643731867248));
#46918=CARTESIAN_POINT('Ctrl Pts',(-3.58251530840628,-1.79748282676246,
-6.03203711468279));
#46919=CARTESIAN_POINT('Ctrl Pts',(-3.69184159328838,-1.56115840039459,
-6.03981172763717));
#46920=CARTESIAN_POINT('Ctrl Pts',(-3.86307243977381,-1.06969754939593,
-6.055217035039));
#46921=CARTESIAN_POINT('Ctrl Pts',(-3.92434285512731,-0.815931314990128,
-6.06296225403942));
#46922=CARTESIAN_POINT('Ctrl Pts',(-4.03406563442041,-0.037214853224006,
-6.08657768116259));
#46923=CARTESIAN_POINT('Ctrl Pts',(-4.00430017251761,0.491396238184421,
-6.10188288702623));
#46924=CARTESIAN_POINT('Ctrl Pts',(-3.74064529529872,1.51094508957726,-6.13350865285382));
#46925=CARTESIAN_POINT('Ctrl Pts',(-3.51050440416036,1.98791707408525,-6.14881710089216));
#46926=CARTESIAN_POINT('Ctrl Pts',(-2.87658037467787,2.82858535128957,-6.18043719471254));
#46927=CARTESIAN_POINT('Ctrl Pts',(-2.48146635415407,3.18076522952212,-6.19573752053965));
#46928=CARTESIAN_POINT('Ctrl Pts',(-1.80808528881573,3.57693292985488,-6.21919924901615));
#46929=CARTESIAN_POINT('Ctrl Pts',(-1.57602875290289,3.68525790641758,-6.22680560757718));
#46930=CARTESIAN_POINT('Ctrl Pts',(-1.09046514191568,3.85715392422301,-6.24205021209597));
#46931=CARTESIAN_POINT('Ctrl Pts',(-0.838128636157874,3.9195341748809,-6.2498027116221));
#46932=CARTESIAN_POINT('Ctrl Pts',(-0.324784493721326,3.99508605519258,
-6.26538453238125));
#46933=CARTESIAN_POINT('Ctrl Pts',(-0.0639985411799379,4.00792889648622,
-6.27313412863224));
#46934=CARTESIAN_POINT('Ctrl Pts',(0.455831514449376,3.98235304377092,-6.28853920799261));
#46935=CARTESIAN_POINT('Ctrl Pts',(0.713374235138799,3.9441684530238,-6.29631043639614));
#46936=CARTESIAN_POINT('Ctrl Pts',(1.21755827403787,3.81889215063033,-6.3119106595662));
#46937=CARTESIAN_POINT('Ctrl Pts',(1.4638408333804,3.73160747445902,-6.3196580212283));
#46938=CARTESIAN_POINT('Ctrl Pts',(1.93538621191033,3.51017181965194,-6.33508018020164));
#46939=CARTESIAN_POINT('Ctrl Pts',(2.15936014956644,3.3767799996088,-6.34286768747215));
#46940=CARTESIAN_POINT('Ctrl Pts',(2.47370387509418,3.14585174539135,-6.35457938315572));
#46941=CARTESIAN_POINT('Ctrl Pts',(2.57528063181982,3.06331535930681,-6.35850050731362));
#46942=CARTESIAN_POINT('Ctrl Pts',(2.81644751835964,2.84686502890774,-6.36815901024042));
#46943=CARTESIAN_POINT('Ctrl Pts',(2.95056536148859,2.70761623303713,-6.3738297545191));
#46944=CARTESIAN_POINT('Ctrl Pts',(3.242968070882,2.35616404170762,-6.38744184306815));
#46945=CARTESIAN_POINT('Ctrl Pts',(3.39164237499895,2.13648822658386,-6.39540961772807));
#46946=CARTESIAN_POINT('Ctrl Pts',(3.64069060839852,1.67682637413702,-6.41106253356384));
#46947=CARTESIAN_POINT('Ctrl Pts',(3.7413926191674,1.43832135217425,-6.41863869330694));
#46948=CARTESIAN_POINT('Ctrl Pts',(3.89697770694004,0.939097436878513,-6.43422035595438));
#46949=CARTESIAN_POINT('Ctrl Pts',(3.95053109180025,0.679145432974062,-6.44219401913166));
#46950=CARTESIAN_POINT('Ctrl Pts',(4.00503852306483,0.160037776789208,-6.4578136851245));
#46951=CARTESIAN_POINT('Ctrl Pts',(4.00707960659604,-0.0978392793946785,
-6.46535594156364));
#46952=CARTESIAN_POINT('Ctrl Pts',(3.94935809009518,-0.744053604171874,
-6.48470221438685));
#46953=CARTESIAN_POINT('Ctrl Pts',(3.85734458348044,-1.12884509202111,-6.49655343292719));
#46954=CARTESIAN_POINT('Ctrl Pts',(3.6156412195022,-1.72971237807858,-6.51572318010026));
#46955=CARTESIAN_POINT('Ctrl Pts',(3.49789688270283,-1.95656801441268,-6.52330862450278));
#46956=CARTESIAN_POINT('Ctrl Pts',(3.07420677216998,-2.61227115933583,-6.54675135106245));
#46957=CARTESIAN_POINT('Ctrl Pts',(2.70595697537982,-2.99224488648191,-6.56204832520248));
#46958=CARTESIAN_POINT('Ctrl Pts',(1.83958567158901,-3.59042937177047,-6.59366554939926));
#46959=CARTESIAN_POINT('Ctrl Pts',(1.35350869025928,-3.80046903462749,-6.6089719068721));
#46960=CARTESIAN_POINT('Ctrl Pts',(0.323857924712615,-4.02129459570999,
-6.64059730443942));
#46961=CARTESIAN_POINT('Ctrl Pts',(-0.205618287062566,-4.02901476468918,
-6.65590426094551));
#46962=CARTESIAN_POINT('Ctrl Pts',(-0.979034883079649,-3.88684859441061,
-6.67951960433248));
#46963=CARTESIAN_POINT('Ctrl Pts',(-1.22996724620899,-3.81506200049018,
-6.68726999926218));
#46964=CARTESIAN_POINT('Ctrl Pts',(-1.71359054806626,-3.62359490712295,
-6.70266480560325));
#46965=CARTESIAN_POINT('Ctrl Pts',(-1.94493551396776,-3.50464134143606,
-6.71042605173161));
#46966=CARTESIAN_POINT('Ctrl Pts',(-2.38168882276234,-3.22394798047734,
-6.72601655674101));
#46967=CARTESIAN_POINT('Ctrl Pts',(-2.58670753680856,-3.06212275004188,
-6.73376526482012));
#46968=CARTESIAN_POINT('Ctrl Pts',(-2.96175735836674,-2.70092027443588,
-6.74917855593458));
#46969=CARTESIAN_POINT('Ctrl Pts',(-3.13080861264775,-2.5026913412351,-6.75695767350024));
#46970=CARTESIAN_POINT('Ctrl Pts',(-3.35408055590606,-2.18305165860493,
-6.76866529572382));
#46971=CARTESIAN_POINT('Ctrl Pts',(-3.42370238331577,-2.07224527451541,
-6.77258657284991));
#46972=CARTESIAN_POINT('Ctrl Pts',(-3.58435262239504,-1.786325901136,-6.78236449836579));
#46973=CARTESIAN_POINT('Ctrl Pts',(-3.66795560240138,-1.60768666132749,
-6.78814844247439));
#46974=CARTESIAN_POINT('Ctrl Pts',(-3.83192874197579,-1.17672052423941,
-6.80187824847632));
#46975=CARTESIAN_POINT('Ctrl Pts',(-3.90130361899299,-0.920683776449137,
-6.80984649243886));
#46976=CARTESIAN_POINT('Ctrl Pts',(-3.98775544337577,-0.405152609759138,
-6.82549680080856));
#46977=CARTESIAN_POINT('Ctrl Pts',(-4.00563982581271,-0.146956557846932,
-6.83307024502416));
#46978=CARTESIAN_POINT('Ctrl Pts',(-3.9908900606506,0.375680334170695,-6.84865101421972));
#46979=CARTESIAN_POINT('Ctrl Pts',(-3.95723043335599,0.638961096328632,
-6.85662513993275));
#46980=CARTESIAN_POINT('Ctrl Pts',(-3.84042797784801,1.14761618106337,-6.87224211503868));
#46981=CARTESIAN_POINT('Ctrl Pts',(-3.75874590502152,1.39213689705194,-6.87978169477132));
#46982=CARTESIAN_POINT('Ctrl Pts',(-3.494082173173,1.98580787585089,-6.89916494719082));
#46983=CARTESIAN_POINT('Ctrl Pts',(-3.28138689292828,2.32097973033577,-6.91105332540699));
#46984=CARTESIAN_POINT('Ctrl Pts',(-2.85631112735569,2.81183723359036,-6.9302717397664));
#46985=CARTESIAN_POINT('Ctrl Pts',(-2.67089507302673,2.98829611630492,-6.93787084862123));
#46986=CARTESIAN_POINT('Ctrl Pts',(-2.05651220821157,3.47067870185686,-6.96132757815569));
#46987=CARTESIAN_POINT('Ctrl Pts',(-1.58453026772136,3.71011770819878,-6.97662703430569));
#46988=CARTESIAN_POINT('Ctrl Pts',(-0.570552308223067,3.99372362689401,
-7.00824687910573));
#46989=CARTESIAN_POINT('Ctrl Pts',(-0.0425135651029989,4.03406360844439,
-7.02355492652206));
#46990=CARTESIAN_POINT('Ctrl Pts',(1.00294575768625,3.90766901147879,-7.05518045364007));
#46991=CARTESIAN_POINT('Ctrl Pts',(1.50603691010037,3.74259279021727,-7.07048619951904));
#46992=CARTESIAN_POINT('Ctrl Pts',(2.19110922183819,3.35637086647038,-7.09410318036229));
#46993=CARTESIAN_POINT('Ctrl Pts',(2.40507091361469,3.20674516340418,-7.10185290577662));
#46994=CARTESIAN_POINT('Ctrl Pts',(2.80020366411324,2.86805997546332,-7.11725674565276));
#46995=CARTESIAN_POINT('Ctrl Pts',(2.98033225870797,2.68010786110962,-7.12502675988284));
#46996=CARTESIAN_POINT('Ctrl Pts',(3.3020231442549,2.27222704406893,-7.14062577316418));
#46997=CARTESIAN_POINT('Ctrl Pts',(3.44318468809885,2.05236308725259,-7.14837326832889));
#46998=CARTESIAN_POINT('Ctrl Pts',(3.68018495053807,1.5884768372515,-7.16379425838034));
#46999=CARTESIAN_POINT('Ctrl Pts',(3.77546949052777,1.34584612505591,-7.17158073678445));
#47000=CARTESIAN_POINT('Ctrl Pts',(3.88242319580831,0.970762049803752,-7.18329206091474));
#47001=CARTESIAN_POINT('Ctrl Pts',(3.91213631086002,0.843299989361819,-7.18721324150571));
#47002=CARTESIAN_POINT('Ctrl Pts',(3.97026086590606,0.523763264771169,-7.19689389874605));
#47003=CARTESIAN_POINT('Ctrl Pts',(3.99097361089814,0.330812765971013,-7.20258586806465));
#47004=CARTESIAN_POINT('Ctrl Pts',(4.00652839568716,-0.1268409864058,-7.21622055359675));
#47005=CARTESIAN_POINT('Ctrl Pts',(3.9893015001724,-0.39154413335847,-7.22418862353994));
#47006=CARTESIAN_POINT('Ctrl Pts',(3.90728476653639,-0.88888007669014,-7.23927958026253));
#47007=CARTESIAN_POINT('Ctrl Pts',(3.84710144367332,-1.12121155500227,-7.24631748009599));
#47008=CARTESIAN_POINT('Ctrl Pts',(3.68534768752621,-1.57312408692967,-7.26059183626647));
#47009=CARTESIAN_POINT('Ctrl Pts',(3.58396937038137,-1.79191386936569,-7.26782957759934));
#47010=CARTESIAN_POINT('Ctrl Pts',(3.46394390204312,-1.99990900584449,-7.27503265522596));
#47011=CARTESIAN_POINT('',(-1.2107513073724,-3.3265118775804,-4.70724779054699));
#47012=CARTESIAN_POINT('Ctrl Pts',(-1.21071383810565,-3.32640900566591,
-4.70724779141669));
#47013=CARTESIAN_POINT('Ctrl Pts',(-1.39219287918788,-3.26025710940742,
-4.71376120107113));
#47014=CARTESIAN_POINT('Ctrl Pts',(-1.56825188079738,-3.17927104752986,
-4.72027461072506));
#47015=CARTESIAN_POINT('Ctrl Pts',(-1.73659924449935,-3.08457088033829,
-4.72678802037908));
#47016=CARTESIAN_POINT('Ctrl Pts',(-1.87338108397249,-3.00762721586959,
-4.732080150497));
#47017=CARTESIAN_POINT('Ctrl Pts',(-2.00508361696359,-2.92162011815734,
-4.73737228061497));
#47018=CARTESIAN_POINT('Ctrl Pts',(-2.13042518195858,-2.827169705567,-4.74266441073295));
#47019=CARTESIAN_POINT('Ctrl Pts',(-2.15935060962041,-2.80537311656542,
-4.74388569057664));
#47020=CARTESIAN_POINT('Ctrl Pts',(-2.18793730334398,-2.78312691895196,
-4.74510697042032));
#47021=CARTESIAN_POINT('Ctrl Pts',(-2.21617354772985,-2.76044407979828,
-4.74632825026401));
#47022=CARTESIAN_POINT('Ctrl Pts',(-2.36676494282521,-2.63947047062431,
-4.75284166022567));
#47023=CARTESIAN_POINT('Ctrl Pts',(-2.50737055352154,-2.50609287961651,
-4.75935507018733));
#47024=CARTESIAN_POINT('Ctrl Pts',(-2.63627091172052,-2.36224216903429,
-4.76586848014899));
#47025=CARTESIAN_POINT('Ctrl Pts',(-2.76517126991969,-2.21839145845186,
-4.77238189011066));
#47026=CARTESIAN_POINT('Ctrl Pts',(-2.88238227181575,-2.06404968982843,
-4.77889530007233));
#47027=CARTESIAN_POINT('Ctrl Pts',(-2.98616562034842,-1.90113425254753,
-4.785408710034));
#47028=CARTESIAN_POINT('Ctrl Pts',(-3.0036792827206,-1.87364192353623,-4.78650786191697));
#47029=CARTESIAN_POINT('Ctrl Pts',(-3.02081015796238,-1.84590601958711,
-4.78760701379993));
#47030=CARTESIAN_POINT('Ctrl Pts',(-3.03754976626217,-1.81793603228567,
-4.7887061656829));
#47031=CARTESIAN_POINT('Ctrl Pts',(-3.12000657762367,-1.6801600505903,-4.7941204237616));
#47032=CARTESIAN_POINT('Ctrl Pts',(-3.1929686605663,-1.53670385765163,-4.7995346818403));
#47033=CARTESIAN_POINT('Ctrl Pts',(-3.25592170098541,-1.38899996899466,
-4.804948939919));
#47034=CARTESIAN_POINT('Ctrl Pts',(-3.3316548770961,-1.21131062250045,-4.81146234988067));
#47035=CARTESIAN_POINT('Ctrl Pts',(-3.39291563048331,-1.0274545075206,-4.81797575984233));
#47036=CARTESIAN_POINT('Ctrl Pts',(-3.4388318118105,-0.839831766260492,
-4.824489169804));
#47037=CARTESIAN_POINT('Ctrl Pts',(-3.46293778073547,-0.741329934450789,
-4.82790870630711));
#47038=CARTESIAN_POINT('Ctrl Pts',(-3.48281390249413,-0.641787444045981,
-4.83132824281022));
#47039=CARTESIAN_POINT('Ctrl Pts',(-3.49832847032117,-0.541569860445466,
-4.83474777931332));
#47040=CARTESIAN_POINT('Ctrl Pts',(-3.51236549246657,-0.450896600574981,
-4.83784165277189));
#47041=CARTESIAN_POINT('Ctrl Pts',(-3.52283219794054,-0.359670757793759,
-4.84093552623045));
#47042=CARTESIAN_POINT('Ctrl Pts',(-3.52973959895587,-0.268179901742102,
-4.84402939968901));
#47043=CARTESIAN_POINT('Ctrl Pts',(-3.54428147831359,-0.0755678052264873,
-4.85054280965067));
#47044=CARTESIAN_POINT('Ctrl Pts',(-3.54305196908429,0.118222685023444,
-4.85705621961233));
#47045=CARTESIAN_POINT('Ctrl Pts',(-3.52615816121155,0.3106374510054,-4.86356962957399));
#47046=CARTESIAN_POINT('Ctrl Pts',(-3.51127051610728,0.480202700612879,
-4.86930956320283));
#47047=CARTESIAN_POINT('Ctrl Pts',(-3.48421326830643,0.648717483567016,
-4.87504949683167));
#47048=CARTESIAN_POINT('Ctrl Pts',(-3.44505320963117,0.814376069645967,
-4.8807894304605));
#47049=CARTESIAN_POINT('Ctrl Pts',(-3.43977625339156,0.836699149309945,
-4.88156290679333));
#47050=CARTESIAN_POINT('Ctrl Pts',(-3.4342795483969,0.85897036558526,-4.88233638312617));
#47051=CARTESIAN_POINT('Ctrl Pts',(-3.42856490437154,0.881185686590716,
-4.883109859459));
#47052=CARTESIAN_POINT('Ctrl Pts',(-3.38044213998663,1.06825992144005,-4.88962326942067));
#47053=CARTESIAN_POINT('Ctrl Pts',(-3.31687241555554,1.25134319073251,-4.89613667938233));
#47054=CARTESIAN_POINT('Ctrl Pts',(-3.23893637138191,1.42807546042492,-4.90265008934417));
#47055=CARTESIAN_POINT('Ctrl Pts',(-3.16100032720827,1.60480773011733,-4.909163499306));
#47056=CARTESIAN_POINT('Ctrl Pts',(-3.06868910928958,1.77521130597631,-4.915676909268));
#47057=CARTESIAN_POINT('Ctrl Pts',(-2.96305546573071,1.93693229393157,-4.92219031922984));
#47058=CARTESIAN_POINT('Ctrl Pts',(-2.93796716681119,1.97534150098615,-4.92373727312258));
#47059=CARTESIAN_POINT('Ctrl Pts',(-2.91212788447957,2.01326000353812,-4.92528422701531));
#47060=CARTESIAN_POINT('Ctrl Pts',(-2.88555239687917,2.05065535009337,-4.92683118090804));
#47061=CARTESIAN_POINT('Ctrl Pts',(-2.80023247086108,2.1707121576857,-4.93179763697708));
#47062=CARTESIAN_POINT('Ctrl Pts',(-2.70732368293247,2.28537607124037,-4.93676409304604));
#47063=CARTESIAN_POINT('Ctrl Pts',(-2.60768233598873,2.39383487273625,-4.94173054911501));
#47064=CARTESIAN_POINT('Ctrl Pts',(-2.47700465903675,2.53607646881263,-4.94824395907667));
#47065=CARTESIAN_POINT('Ctrl Pts',(-2.3347360735518,2.66766424466987,-4.95475736903833));
#47066=CARTESIAN_POINT('Ctrl Pts',(-2.18272371894347,2.78683825766546,-4.96127077899999));
#47067=CARTESIAN_POINT('Ctrl Pts',(-2.09246668450921,2.85759759181515,-4.9651381032626));
#47068=CARTESIAN_POINT('Ctrl Pts',(-1.99876997137404,2.92398232168098,-4.96900542752521));
#47069=CARTESIAN_POINT('Ctrl Pts',(-1.90204061354772,2.98560571817767,-4.97287275178782));
#47070=CARTESIAN_POINT('Ctrl Pts',(-1.83585682521188,3.02776944098037,-4.97551883748687));
#47071=CARTESIAN_POINT('Ctrl Pts',(-1.7682533936754,3.06770422962763,-4.97816492318592));
#47072=CARTESIAN_POINT('Ctrl Pts',(-1.69939760621079,3.10534408721984,-4.98081100888498));
#47073=CARTESIAN_POINT('Ctrl Pts',(-1.52990726349332,3.19799559260592,-4.98732441884667));
#47074=CARTESIAN_POINT('Ctrl Pts',(-1.35283221159455,3.27674344861159,-4.99383782880837));
#47075=CARTESIAN_POINT('Ctrl Pts',(-1.1705592811959,3.34065903690989,-5.00035123877007));
#47076=CARTESIAN_POINT('Ctrl Pts',(-0.997400068785245,3.40137882073238,
-5.00653897567983));
#47077=CARTESIAN_POINT('Ctrl Pts',(-0.819528440494076,3.44871677050005,
-5.01272671258958));
#47078=CARTESIAN_POINT('Ctrl Pts',(-0.639037774186981,3.4818430066795,-5.01891444949934));
#47079=CARTESIAN_POINT('Ctrl Pts',(-0.629538187021195,3.48358650718565,
-5.01924012255123));
#47080=CARTESIAN_POINT('Ctrl Pts',(-0.62003134595265,3.48529064171064,-5.01956579560311));
#47081=CARTESIAN_POINT('Ctrl Pts',(-0.61051757907874,3.48695541282214,-5.019891468655));
#47082=CARTESIAN_POINT('Ctrl Pts',(-0.420243733667227,3.52025057396201,
-5.02640487861664));
#47083=CARTESIAN_POINT('Ctrl Pts',(-0.227230723008247,3.53779512210829,
-5.03291828857827));
#47084=CARTESIAN_POINT('Ctrl Pts',(-0.0340855960367684,3.53962915369353,
-5.03943169853991));
#47085=CARTESIAN_POINT('Ctrl Pts',(0.159059530937512,3.54146318527879,-5.04594510850163));
#47086=CARTESIAN_POINT('Ctrl Pts',(0.352360719567761,3.52758887010852,-5.05245851846337));
#47087=CARTESIAN_POINT('Ctrl Pts',(0.543247550769443,3.4980247813142,-5.05897192842508));
#47088=CARTESIAN_POINT('Ctrl Pts',(0.601707228720348,3.48897068837889,-5.06096668021768));
#47089=CARTESIAN_POINT('Ctrl Pts',(0.659939301890289,3.47844500445235,-5.06296143201029));
#47090=CARTESIAN_POINT('Ctrl Pts',(0.717867025561981,3.466448749601,-5.06495618380289));
#47091=CARTESIAN_POINT('Ctrl Pts',(0.849089156932971,3.43927395262494,-5.0694748419719));
#47092=CARTESIAN_POINT('Ctrl Pts',(0.978749296819402,3.40455233357054,-5.07399350014091));
#47093=CARTESIAN_POINT('Ctrl Pts',(1.10602473720318,3.36262936004284,-5.07851215830992));
#47094=CARTESIAN_POINT('Ctrl Pts',(1.28948564313355,3.30219958129296,-5.08502556827163));
#47095=CARTESIAN_POINT('Ctrl Pts',(1.46801104029239,3.22680554536042,-5.09153897823337));
#47096=CARTESIAN_POINT('Ctrl Pts',(1.63924880370262,3.13743299108219,-5.09805238819509));
#47097=CARTESIAN_POINT('Ctrl Pts',(1.75269332737295,3.07822393200914,-5.10236750348195));
#47098=CARTESIAN_POINT('Ctrl Pts',(1.86294511722153,3.01287435802278,-5.1066826187688));
#47099=CARTESIAN_POINT('Ctrl Pts',(1.96928647887088,2.941685021231,-5.11099773405565));
#47100=CARTESIAN_POINT('Ctrl Pts',(2.02346107989141,2.90541828684098,-5.11319602873044));
#47101=CARTESIAN_POINT('Ctrl Pts',(2.07662086897177,2.86763609085749,-5.11539432340522));
#47102=CARTESIAN_POINT('Ctrl Pts',(2.12869278492199,2.82841085585619,-5.11759261808));
#47103=CARTESIAN_POINT('Ctrl Pts',(2.28297862292286,2.71218893195501,-5.12410602804164));
#47104=CARTESIAN_POINT('Ctrl Pts',(2.42770829556085,2.58330600898348,-5.13061943800327));
#47105=CARTESIAN_POINT('Ctrl Pts',(2.56106883516398,2.44357975449348,-5.1371328479649));
#47106=CARTESIAN_POINT('Ctrl Pts',(2.69442937476905,2.30385350000145,-5.14364625792664));
#47107=CARTESIAN_POINT('Ctrl Pts',(2.81643557043219,2.1532649176556,-5.15015966788837));
#47108=CARTESIAN_POINT('Ctrl Pts',(2.92522794721502,1.99364991391056,-5.15667307785009));
#47109=CARTESIAN_POINT('Ctrl Pts',(2.92726781554804,1.99065711605796,-5.15679520496151));
#47110=CARTESIAN_POINT('Ctrl Pts',(2.92930303206135,1.98766115426643,-5.15691733207293));
#47111=CARTESIAN_POINT('Ctrl Pts',(2.9313335845635,1.984662040754,-5.15703945918435));
#47112=CARTESIAN_POINT('Ctrl Pts',(3.03759856727369,1.82770931719371,-5.16343074203457));
#47113=CARTESIAN_POINT('Ctrl Pts',(3.13108925869377,1.66212467796123,-5.16982202488478));
#47114=CARTESIAN_POINT('Ctrl Pts',(3.21084406279643,1.49018936490803,-5.176213307735));
#47115=CARTESIAN_POINT('Ctrl Pts',(3.29212285262701,1.31496864521171,-5.18272671769664));
#47116=CARTESIAN_POINT('Ctrl Pts',(3.35914855060852,1.13313177099434,-5.18924012765827));
#47117=CARTESIAN_POINT('Ctrl Pts',(3.41090884185987,0.947034149938319,-5.19575353761991));
#47118=CARTESIAN_POINT('Ctrl Pts',(3.43031907907144,0.877247081862021,-5.19819608246181));
#47119=CARTESIAN_POINT('Ctrl Pts',(3.4475820095095,0.806861453565564,-5.20063862730372));
#47120=CARTESIAN_POINT('Ctrl Pts',(3.46264250659767,0.736007385494901,-5.20308117214562));
#47121=CARTESIAN_POINT('Ctrl Pts',(3.48774307025223,0.617918517950802,-5.20715203726545));
#47122=CARTESIAN_POINT('Ctrl Pts',(3.50672549247776,0.498528446452136,-5.21122290238527));
#47123=CARTESIAN_POINT('Ctrl Pts',(3.51957889593106,0.378491351196591,-5.21529376750508));
#47124=CARTESIAN_POINT('Ctrl Pts',(3.54014442282263,0.186431238913331,-5.2218071774667));
#47125=CARTESIAN_POINT('Ctrl Pts',(3.54502560134987,-0.00730000610566984,
-5.2283205874283));
#47126=CARTESIAN_POINT('Ctrl Pts',(3.53418198158554,-0.200151998238902,
-5.23483399739009));
#47127=CARTESIAN_POINT('Ctrl Pts',(3.52625261802275,-0.341174423652751,
-5.23959690836843));
#47128=CARTESIAN_POINT('Ctrl Pts',(3.50991175822703,-0.481737410954006,
-5.24435981934687));
#47129=CARTESIAN_POINT('Ctrl Pts',(3.48514125710933,-0.620798210365567,
-5.24912273032526));
#47130=CARTESIAN_POINT('Ctrl Pts',(3.47603742602251,-0.671906826320724,
-5.25087322930883));
#47131=CARTESIAN_POINT('Ctrl Pts',(3.46579506342518,-0.722812536677146,
-5.25262372829238));
#47132=CARTESIAN_POINT('Ctrl Pts',(3.45443274215295,-0.7734670235766,-5.25437422727593));
#47133=CARTESIAN_POINT('Ctrl Pts',(3.41215482182319,-0.961946675768368,
-5.26088763723773));
#47134=CARTESIAN_POINT('Ctrl Pts',(3.35437640811406,-1.1469330851341,-5.26740104719937));
#47135=CARTESIAN_POINT('Ctrl Pts',(3.28203684521707,-1.32602898115537,-5.273914457161));
#47136=CARTESIAN_POINT('Ctrl Pts',(3.20969728232009,-1.50512487717664,-5.28042786712264));
#47137=CARTESIAN_POINT('Ctrl Pts',(3.12278631763227,-1.67835197646303,-5.28694127708427));
#47138=CARTESIAN_POINT('Ctrl Pts',(3.02223197295951,-1.8432806479056,-5.29345468704591));
#47139=CARTESIAN_POINT('Ctrl Pts',(3.01343337877785,-1.85771205267151,-5.294024616184));
#47140=CARTESIAN_POINT('Ctrl Pts',(3.00453044323614,-1.8720797233967,-5.2945945453221));
#47141=CARTESIAN_POINT('Ctrl Pts',(2.9955238080915,-1.8863820172901,-5.2951644744602));
#47142=CARTESIAN_POINT('Ctrl Pts',(2.90159851161271,-2.03553285694236,-5.30110795528383));
#47143=CARTESIAN_POINT('Ctrl Pts',(2.79639484911094,-2.17757303830368,-5.30705143610746));
#47144=CARTESIAN_POINT('Ctrl Pts',(2.68128796199762,-2.31104848987915,-5.31299491693108));
#47145=CARTESIAN_POINT('Ctrl Pts',(2.55514330578951,-2.45732309927445,-5.3195083268927));
#47146=CARTESIAN_POINT('Ctrl Pts',(2.41709243724114,-2.5933320851481,-5.3260217368543));
#47147=CARTESIAN_POINT('Ctrl Pts',(2.26888276917332,-2.71720685314313,-5.33253514681592));
#47148=CARTESIAN_POINT('Ctrl Pts',(2.20311454325284,-2.77217643666326,-5.33542548064808));
#47149=CARTESIAN_POINT('Ctrl Pts',(2.13534527838208,-2.82475626413618,-5.33831581448023));
#47150=CARTESIAN_POINT('Ctrl Pts',(2.06573588820082,-2.874775685197,-5.34120614831239));
#47151=CARTESIAN_POINT('Ctrl Pts',(1.97847948994207,-2.93747576795006,-5.34482922444196));
#47152=CARTESIAN_POINT('Ctrl Pts',(1.8883316623885,-2.99615253300867,-5.34845230057153));
#47153=CARTESIAN_POINT('Ctrl Pts',(1.79571220403399,-3.05061307565962,-5.3520753767011));
#47154=CARTESIAN_POINT('Ctrl Pts',(1.62920493752531,-3.14851988974053,-5.35858878666273));
#47155=CARTESIAN_POINT('Ctrl Pts',(1.45470238311939,-3.23280915686397,-5.36510219662437));
#47156=CARTESIAN_POINT('Ctrl Pts',(1.2745261419347,-3.30242008610374,-5.371615606586));
#47157=CARTESIAN_POINT('Ctrl Pts',(1.13038560964148,-3.3581086515221,-5.37682631790255));
#47158=CARTESIAN_POINT('Ctrl Pts',(0.982599582851898,-3.40440558395331,
-5.3820370292191));
#47159=CARTESIAN_POINT('Ctrl Pts',(0.83240308038325,-3.440741942048,-5.38724774053564));
#47160=CARTESIAN_POINT('Ctrl Pts',(0.794853354755298,-3.44982617672956,
-5.38855043918073));
#47161=CARTESIAN_POINT('Ctrl Pts',(0.757152994147713,-3.45828791657969,
-5.38985313782582));
#47162=CARTESIAN_POINT('Ctrl Pts',(0.719323216056953,-3.46612616198879,
-5.39115583647091));
#47163=CARTESIAN_POINT('Ctrl Pts',(0.530176743543513,-3.5053168880425,-5.39766924643264));
#47164=CARTESIAN_POINT('Ctrl Pts',(0.33781692832025,-3.52891744226118,-5.40418265639437));
#47165=CARTESIAN_POINT('Ctrl Pts',(0.144825265577312,-3.53682450849308,
-5.4106960663561));
#47166=CARTESIAN_POINT('Ctrl Pts',(-0.0481663971628301,-3.54473157472486,
-5.41720947631773));
#47167=CARTESIAN_POINT('Ctrl Pts',(-0.24181388703863,-3.53694580387158,
-5.42372288627936));
#47168=CARTESIAN_POINT('Ctrl Pts',(-0.433530449310566,-3.51334032191244,
-5.430236296241));
#47169=CARTESIAN_POINT('Ctrl Pts',(-0.463486537026677,-3.5096519192008,
-5.4312540292831));
#47170=CARTESIAN_POINT('Ctrl Pts',(-0.493394854987601,-3.50557733750051,
-5.4322717623252));
#47171=CARTESIAN_POINT('Ctrl Pts',(-0.52324531539875,-3.50111615630133,
-5.4332894953673));
#47172=CARTESIAN_POINT('Ctrl Pts',(-0.684435410967214,-3.4770261351111,
-5.43878517228683));
#47173=CARTESIAN_POINT('Ctrl Pts',(-0.843938087347221,-3.44166213854163,
-5.44428084920637));
#47174=CARTESIAN_POINT('Ctrl Pts',(-1.00025566879186,-3.39555923162819,
-5.44977652612591));
#47175=CARTESIAN_POINT('Ctrl Pts',(-1.1855213798375,-3.34091862273664,-5.45628993608763));
#47176=CARTESIAN_POINT('Ctrl Pts',(-1.36633644531483,-3.2711909851405,-5.46280334604936));
#47177=CARTESIAN_POINT('Ctrl Pts',(-1.54029195487117,-3.18722583254678,
-5.46931675601108));
#47178=CARTESIAN_POINT('Ctrl Pts',(-1.62944410370728,-3.1441937158856,-5.47265487675137));
#47179=CARTESIAN_POINT('Ctrl Pts',(-1.71679583817647,-3.09742028661071,
-5.47599299749165));
#47180=CARTESIAN_POINT('Ctrl Pts',(-1.80200661175619,-3.04702677559417,
-5.47933111823193));
#47181=CARTESIAN_POINT('Ctrl Pts',(-1.88306085512836,-2.99909142968991,
-5.48250640745326));
#47182=CARTESIAN_POINT('Ctrl Pts',(-1.96217788986922,-2.94788060262952,
-5.48568169667459));
#47183=CARTESIAN_POINT('Ctrl Pts',(-2.03912504838554,-2.89360083987272,
-5.48885698589592));
#47184=CARTESIAN_POINT('Ctrl Pts',(-2.19696528084021,-2.78225780217885,
-5.49537039585763));
#47185=CARTESIAN_POINT('Ctrl Pts',(-2.34568157844476,-2.65800144637073,
-5.50188380581937));
#47186=CARTESIAN_POINT('Ctrl Pts',(-2.48336853770675,-2.52253489439242,
-5.50839721578109));
#47187=CARTESIAN_POINT('Ctrl Pts',(-2.60298386808918,-2.40484853936279,
-5.51405573049203));
#47188=CARTESIAN_POINT('Ctrl Pts',(-2.71428549057575,-2.27868697184984,
-5.51971424520297));
#47189=CARTESIAN_POINT('Ctrl Pts',(-2.81597612222633,-2.14519893694035,
-5.52537275991391));
#47190=CARTESIAN_POINT('Ctrl Pts',(-2.83133966592628,-2.12503140307353,
-5.52622765516461));
#47191=CARTESIAN_POINT('Ctrl Pts',(-2.84648385104755,-2.10469665766999,
-5.52708255041531));
#47192=CARTESIAN_POINT('Ctrl Pts',(-2.86140601976011,-2.08420004970933,
-5.527937445666));
#47193=CARTESIAN_POINT('Ctrl Pts',(-2.97509737816046,-1.92803727963656,
-5.53445085562764));
#47194=CARTESIAN_POINT('Ctrl Pts',(-3.07588539103572,-1.76250130618686,
-5.54096426558927));
#47195=CARTESIAN_POINT('Ctrl Pts',(-3.16263326328894,-1.58992343651983,
-5.54747767555091));
#47196=CARTESIAN_POINT('Ctrl Pts',(-3.24938113554341,-1.4173455668503,-5.55399108551264));
#47197=CARTESIAN_POINT('Ctrl Pts',(-3.32210027300758,-1.23770469083994,
-5.56050449547437));
#47198=CARTESIAN_POINT('Ctrl Pts',(-3.37963916765126,-1.05330980373386,
-5.56701790543609));
#47199=CARTESIAN_POINT('Ctrl Pts',(-3.39258558113939,-1.01182043435414,
-5.56848344103779));
#47200=CARTESIAN_POINT('Ctrl Pts',(-3.40476309979245,-0.970091329658437,
-5.56994897663948));
#47201=CARTESIAN_POINT('Ctrl Pts',(-3.41615839043217,-0.928149692388579,
-5.57141451224117));
#47202=CARTESIAN_POINT('Ctrl Pts',(-3.45540820147598,-0.783686388225696,
-5.57646238660112));
#47203=CARTESIAN_POINT('Ctrl Pts',(-3.48537682874472,-0.636701514870851,
-5.58151026096109));
#47204=CARTESIAN_POINT('Ctrl Pts',(-3.50597617628425,-0.488430196162447,
-5.58655813532117));
#47205=CARTESIAN_POINT('Ctrl Pts',(-3.53255607623814,-0.297111669702389,
-5.59307154528297));
#47206=CARTESIAN_POINT('Ctrl Pts',(-3.54354418974018,-0.103630424635091,
-5.59958495524494));
#47207=CARTESIAN_POINT('Ctrl Pts',(-3.53875253925765,0.089468803271073,
-5.60609836520674));
#47208=CARTESIAN_POINT('Ctrl Pts',(-3.53596740081211,0.201707391082333,
-5.60988427333219));
#47209=CARTESIAN_POINT('Ctrl Pts',(-3.52784953284791,0.313821101074286,
-5.61367018145759));
#47210=CARTESIAN_POINT('Ctrl Pts',(-3.51436099043,0.425284409474744,-5.61745608958296));
#47211=CARTESIAN_POINT('Ctrl Pts',(-3.50464336839674,0.505586510921572,
-5.62018359141934));
#47212=CARTESIAN_POINT('Ctrl Pts',(-3.49213834393737,0.585551019147991,
-5.62291109325571));
#47213=CARTESIAN_POINT('Ctrl Pts',(-3.47690638446997,0.66499043379555,-5.62563859509208));
#47214=CARTESIAN_POINT('Ctrl Pts',(-3.44053170812434,0.854695704681691,
-5.6321520050537));
#47215=CARTESIAN_POINT('Ctrl Pts',(-3.38860921956519,1.04140602837934,-5.6386654150153));
#47216=CARTESIAN_POINT('Ctrl Pts',(-3.32193574191479,1.22268842298407,-5.64517882497692));
#47217=CARTESIAN_POINT('Ctrl Pts',(-3.25942939273935,1.3926405697123,-5.65128514328716));
#47218=CARTESIAN_POINT('Ctrl Pts',(-3.18394820657006,1.55784068731747,-5.65739146159741));
#47219=CARTESIAN_POINT('Ctrl Pts',(-3.09615376327333,1.71622605567233,-5.66349777990766));
#47220=CARTESIAN_POINT('Ctrl Pts',(-3.09030074626759,1.7267851778631,-5.66390487155914));
#47221=CARTESIAN_POINT('Ctrl Pts',(-3.08439300690686,1.73731401277661,-5.66431196321062));
#47222=CARTESIAN_POINT('Ctrl Pts',(-3.0784309562568,1.74781206796055,-5.6647190548621));
#47223=CARTESIAN_POINT('Ctrl Pts',(-2.98303897276905,1.91577949486414,-5.67123246482373));
#47224=CARTESIAN_POINT('Ctrl Pts',(-2.87375899624301,2.0758403789111,-5.67774587478537));
#47225=CARTESIAN_POINT('Ctrl Pts',(-2.75227553257105,2.22600746165049,-5.684259284747));
#47226=CARTESIAN_POINT('Ctrl Pts',(-2.63079206889909,2.37617454438987,-5.69077269470864));
#47227=CARTESIAN_POINT('Ctrl Pts',(-2.49709140537515,2.51646756267748,-5.69728610467027));
#47228=CARTESIAN_POINT('Ctrl Pts',(-2.35282015491859,2.64491088381421,-5.70379951463191));
#47229=CARTESIAN_POINT('Ctrl Pts',(-2.31044002818164,2.6826415072826,-5.70571284898501));
#47230=CARTESIAN_POINT('Ctrl Pts',(-2.26714849820321,2.71934870346318,-5.70762618333811));
#47231=CARTESIAN_POINT('Ctrl Pts',(-2.222989224079,2.754980745782,-5.70953951769122));
#47232=CARTESIAN_POINT('Ctrl Pts',(-2.11682063965784,2.84064799389807,-5.71413959329984));
#47233=CARTESIAN_POINT('Ctrl Pts',(-2.00563588372431,2.92009993133965,-5.71873966890847));
#47234=CARTESIAN_POINT('Ctrl Pts',(-1.89026706688281,2.99289754536391,-5.7233397445171));
#47235=CARTESIAN_POINT('Ctrl Pts',(-1.72691227343801,3.09597426512039,-5.72985315447873));
#47236=CARTESIAN_POINT('Ctrl Pts',(-1.55515506607057,3.18572418961666,-5.73636656444037));
#47237=CARTESIAN_POINT('Ctrl Pts',(-1.37724999191978,3.26095501036923,-5.742879974402));
#47238=CARTESIAN_POINT('Ctrl Pts',(-1.26161218703416,3.30985483525111,-5.74711367281605));
#47239=CARTESIAN_POINT('Ctrl Pts',(-1.14336967917686,3.35262137178841,-5.7513473712301));
#47240=CARTESIAN_POINT('Ctrl Pts',(-1.02317256118377,3.3889110212635,-5.75558106964415));
#47241=CARTESIAN_POINT('Ctrl Pts',(-0.958450247245203,3.40845183992259,
-5.75786078119174));
#47242=CARTESIAN_POINT('Ctrl Pts',(-0.89316126230264,3.42611482909649,-5.76014049273932));
#47243=CARTESIAN_POINT('Ctrl Pts',(-0.827419800164984,3.44188829366148,
-5.76242020428691));
#47244=CARTESIAN_POINT('Ctrl Pts',(-0.639588539302361,3.48695497823277,
-5.76893361424864));
#47245=CARTESIAN_POINT('Ctrl Pts',(-0.448071840368298,3.51659792381025,
-5.77544702421037));
#47246=CARTESIAN_POINT('Ctrl Pts',(-0.255423787889024,3.53056979807231,
-5.78196043417208));
#47247=CARTESIAN_POINT('Ctrl Pts',(-0.0627757354125469,3.54454167233417,
-5.7884738441337));
#47248=CARTESIAN_POINT('Ctrl Pts',(0.131027743644164,3.54284160663298,-5.7949872540953));
#47249=CARTESIAN_POINT('Ctrl Pts',(0.323385332326859,3.52519811655209,-5.80150066405692));
#47250=CARTESIAN_POINT('Ctrl Pts',(0.515742921012346,3.50755462647096,-5.80801407401864));
#47251=CARTESIAN_POINT('Ctrl Pts',(0.706621482692652,3.47396442994213,-5.81452748398037));
#47252=CARTESIAN_POINT('Ctrl Pts',(0.893511611909647,3.42517311385951,-5.8210408939421));
#47253=CARTESIAN_POINT('Ctrl Pts',(1.08040174112393,3.3763817977776,-5.82755430390373));
#47254=CARTESIAN_POINT('Ctrl Pts',(1.26332731289825,3.31238606054051,-5.83406771386537));
#47255=CARTESIAN_POINT('Ctrl Pts',(1.43982452056484,3.23389875855054,-5.840581123827));
#47256=CARTESIAN_POINT('Ctrl Pts',(1.50380522324394,3.20544690484081,-5.84294225209465));
#47257=CARTESIAN_POINT('Ctrl Pts',(1.56694025449916,3.17509076695823,-5.8453033803623));
#47258=CARTESIAN_POINT('Ctrl Pts',(1.62910723813456,3.14286646338266,-5.84766450862994));
#47259=CARTESIAN_POINT('Ctrl Pts',(1.73843413564225,3.08619678233581,-5.85181679032393));
#47260=CARTESIAN_POINT('Ctrl Pts',(1.84476690245898,3.02374911182526,-5.85596907201792));
#47261=CARTESIAN_POINT('Ctrl Pts',(1.94756203567169,2.95595504167199,-5.8601213537119));
#47262=CARTESIAN_POINT('Ctrl Pts',(2.10880996970625,2.84961096281966,-5.86663476367363));
#47263=CARTESIAN_POINT('Ctrl Pts',(2.26136901605629,2.73010640649609,-5.87314817363537));
#47264=CARTESIAN_POINT('Ctrl Pts',(2.40324259782627,2.59902847899996,-5.87966158359708));
#47265=CARTESIAN_POINT('Ctrl Pts',(2.50521379478413,2.50481662507491,-5.88434307680947));
#47266=CARTESIAN_POINT('Ctrl Pts',(2.60167081814559,2.40461726441304,-5.88902457002185));
#47267=CARTESIAN_POINT('Ctrl Pts',(2.69183711822383,2.2990460910885,-5.89370606323423));
#47268=CARTESIAN_POINT('Ctrl Pts',(2.72712012469975,2.25773499826505,-5.89553797998346));
#47269=CARTESIAN_POINT('Ctrl Pts',(2.76143995124405,2.2156014429839,-5.89736989673269));
#47270=CARTESIAN_POINT('Ctrl Pts',(2.79476729971627,2.17269706292566,-5.89920181348192));
#47271=CARTESIAN_POINT('Ctrl Pts',(2.91326323225658,2.02014983795509,-5.90571522344363));
#47272=CARTESIAN_POINT('Ctrl Pts',(3.01920517514468,1.85787088053258,-5.91222863340537));
#47273=CARTESIAN_POINT('Ctrl Pts',(3.11133748932251,1.68810632525813,-5.91874204336726));
#47274=CARTESIAN_POINT('Ctrl Pts',(3.203469803499,1.51834176998613,-5.92525545332906));
#47275=CARTESIAN_POINT('Ctrl Pts',(3.28180255010409,1.34106980168587,-5.93176886329103));
#47276=CARTESIAN_POINT('Ctrl Pts',(3.34504642056238,1.15855163970423,-5.93828227325283));
#47277=CARTESIAN_POINT('Ctrl Pts',(3.34978975557038,1.14486264848577,-5.938770783606));
#47278=CARTESIAN_POINT('Ctrl Pts',(3.35444815655005,1.1311443095087,-5.93925929395917));
#47279=CARTESIAN_POINT('Ctrl Pts',(3.35902108122167,1.11739759079248,-5.93974780431234));
#47280=CARTESIAN_POINT('Ctrl Pts',(3.41541991061322,0.94785645481421,-5.94577270392095));
#47281=CARTESIAN_POINT('Ctrl Pts',(3.45881608303693,0.773998449359656,-5.95179760352943));
#47282=CARTESIAN_POINT('Ctrl Pts',(3.48894891305953,0.597889911087293,-5.95782250313791));
#47283=CARTESIAN_POINT('Ctrl Pts',(3.52152497042123,0.407502156590185,-5.96433591309964));
#47284=CARTESIAN_POINT('Ctrl Pts',(3.53860724556339,0.214461276056274,-5.97084932306137));
#47285=CARTESIAN_POINT('Ctrl Pts',(3.53986050381078,0.021304435887652,-5.97736273302309));
#47286=CARTESIAN_POINT('Ctrl Pts',(3.54040097332149,-0.061994742963288,
-5.98017165089967));
#47287=CARTESIAN_POINT('Ctrl Pts',(3.53799699077534,-0.145315513407627,
-5.98298056877624));
#47288=CARTESIAN_POINT('Ctrl Pts',(3.53262128868333,-0.22844437121557,-5.98578948665281));
#47289=CARTESIAN_POINT('Ctrl Pts',(3.5255316382462,-0.338077407609597,-5.98949397873787));
#47290=CARTESIAN_POINT('Ctrl Pts',(3.51327303496331,-0.447376576378206,
-5.99319847082294));
#47291=CARTESIAN_POINT('Ctrl Pts',(3.49597098000898,-0.555864346356779,
-5.996902962908));
#47292=CARTESIAN_POINT('Ctrl Pts',(3.46554970375613,-0.746612579979145,
-6.00341637286964));
#47293=CARTESIAN_POINT('Ctrl Pts',(3.41953925747835,-0.934864572484402,
-6.00992978283127));
#47294=CARTESIAN_POINT('Ctrl Pts',(3.35859301744289,-1.11815333279855,-6.01644319279291));
#47295=CARTESIAN_POINT('Ctrl Pts',(3.31059801777636,-1.2624927372481,-6.02157248557216));
#47296=CARTESIAN_POINT('Ctrl Pts',(3.25333356013243,-1.40376624524555,-6.02670177835142));
#47297=CARTESIAN_POINT('Ctrl Pts',(3.18712845076366,-1.54071809177819,-6.03183107113067));
#47298=CARTESIAN_POINT('Ctrl Pts',(3.16926329207835,-1.57767394751018,-6.03321518831314));
#47299=CARTESIAN_POINT('Ctrl Pts',(3.15074717578934,-1.61431513677177,-6.03459930549561));
#47300=CARTESIAN_POINT('Ctrl Pts',(3.13159534362019,-1.65062121645643,-6.03598342267808));
#47301=CARTESIAN_POINT('Ctrl Pts',(3.04147021836802,-1.82147118788974,-6.0424968326397));
#47302=CARTESIAN_POINT('Ctrl Pts',(2.93727842881738,-1.98488223342344,-6.04901024260131));
#47303=CARTESIAN_POINT('Ctrl Pts',(2.82057762917812,-2.13879529781198,-6.05552365256292));
#47304=CARTESIAN_POINT('Ctrl Pts',(2.70387682953718,-2.29270836220275,-6.06203706252464));
#47305=CARTESIAN_POINT('Ctrl Pts',(2.57465211340251,-2.43714224335224,-6.06855047248637));
#47306=CARTESIAN_POINT('Ctrl Pts',(2.43444850641693,-2.57001604546182,-6.0750638824481));
#47307=CARTESIAN_POINT('Ctrl Pts',(2.41429399083976,-2.58911688867116,-6.07600019660831));
#47308=CARTESIAN_POINT('Ctrl Pts',(2.39391298941519,-2.60797845638822,-6.07693651076853));
#47309=CARTESIAN_POINT('Ctrl Pts',(2.37331023111434,-2.62659447705366,-6.07787282492875));
#47310=CARTESIAN_POINT('Ctrl Pts',(2.25059121040597,-2.73747962127514,-6.08344992073017));
#47311=CARTESIAN_POINT('Ctrl Pts',(2.12000384287054,-2.839652015463,-6.08902701653158));
#47312=CARTESIAN_POINT('Ctrl Pts',(1.98297254939446,-2.93225806317012,-6.094604112333));
#47313=CARTESIAN_POINT('Ctrl Pts',(1.82293567289756,-3.04041133417721,-6.10111752229464));
#47314=CARTESIAN_POINT('Ctrl Pts',(1.65409266030275,-3.13553304456699,-6.10763093225627));
#47315=CARTESIAN_POINT('Ctrl Pts',(1.47862930850234,-3.2163003073892,-6.11414434221791));
#47316=CARTESIAN_POINT('Ctrl Pts',(1.390897632601,-3.25668393880083,-6.11740104719877));
#47317=CARTESIAN_POINT('Ctrl Pts',(1.30150905535828,-3.29347875878619,-6.12065775217963));
#47318=CARTESIAN_POINT('Ctrl Pts',(1.21075130737302,-3.32651187758184,-6.12391445716049));
#47319=CARTESIAN_POINT('Ctrl Pts',(1.1199935593875,-3.35954499637758,-6.12717116214136));
#47320=CARTESIAN_POINT('Ctrl Pts',(1.02786668212491,-3.3888163988914,-6.13042786712223));
#47321=CARTESIAN_POINT('Ctrl Pts',(0.934702221409373,-3.414273576702,-6.1336845721031));
#47322=CARTESIAN_POINT('Ctrl Pts',(0.748373299981275,-3.46518793232237,
-6.14019798206473));
#47323=CARTESIAN_POINT('Ctrl Pts',(0.557888991572958,-3.50085067113629,
-6.14671139202637));
#47324=CARTESIAN_POINT('Ctrl Pts',(0.365774049088018,-3.52087018018125,
-6.153224801988));
#47325=CARTESIAN_POINT('Ctrl Pts',(0.20127596813921,-3.53801184952169,-6.15880189778942));
#47326=CARTESIAN_POINT('Ctrl Pts',(0.0355650918612497,-3.54368319654726,
-6.16437899359083));
#47327=CARTESIAN_POINT('Ctrl Pts',(-0.1297187288212,-3.53762251397617,-6.16995608939225));
#47328=CARTESIAN_POINT('Ctrl Pts',(-0.157467504755981,-3.53660501255357,
-6.17089240355247));
#47329=CARTESIAN_POINT('Ctrl Pts',(-0.185204239670332,-3.53525686860412,
-6.17182871771269));
#47330=CARTESIAN_POINT('Ctrl Pts',(-0.212921279681585,-3.53357984669696,
-6.17276503187291));
#47331=CARTESIAN_POINT('Ctrl Pts',(-0.405733107366116,-3.52191375035853,
-6.17927844183464));
#47332=CARTESIAN_POINT('Ctrl Pts',(-0.597565292296506,-3.49433502470254,
-6.18579185179637));
#47333=CARTESIAN_POINT('Ctrl Pts',(-0.785896702128393,-3.45144460505232,
-6.19230526175808));
#47334=CARTESIAN_POINT('Ctrl Pts',(-0.97422811195755,-3.40855418540273,
-6.1988186717197));
#47335=CARTESIAN_POINT('Ctrl Pts',(-1.15908224871662,-3.35034725338159,
-6.2053320816813));
#47336=CARTESIAN_POINT('Ctrl Pts',(-1.33794234485403,-3.27739989599169,
-6.21184549164292));
#47337=CARTESIAN_POINT('Ctrl Pts',(-1.37595059764031,-3.26189838581898,
-6.21322960882539));
#47338=CARTESIAN_POINT('Ctrl Pts',(-1.41368726809313,-3.24573153652599,
-6.21461372600786));
#47339=CARTESIAN_POINT('Ctrl Pts',(-1.4511275397993,-3.22890521124983,-6.21599784319033));
#47340=CARTESIAN_POINT('Ctrl Pts',(-1.58987454601214,-3.16654983423889,
-6.22112713596958));
#47341=CARTESIAN_POINT('Ctrl Pts',(-1.72455052609608,-3.09513693232657,
-6.22625642874884));
#47342=CARTESIAN_POINT('Ctrl Pts',(-1.85409640965779,-3.01541712473751,
-6.2313857215281));
#47343=CARTESIAN_POINT('Ctrl Pts',(-2.01859968229062,-2.91418527636456,
-6.23789913148973));
#47344=CARTESIAN_POINT('Ctrl Pts',(-2.17485177726832,-2.79955082838338,
-6.24441254145137));
#47345=CARTESIAN_POINT('Ctrl Pts',(-2.32076642803647,-2.67298362342837,
-6.250925951413));
#47346=CARTESIAN_POINT('Ctrl Pts',(-2.40375516543355,-2.60099871663665,
-6.25463044349806));
#47347=CARTESIAN_POINT('Ctrl Pts',(-2.48340195179236,-2.52515037406617,
-6.25833493558313));
#47348=CARTESIAN_POINT('Ctrl Pts',(-2.55930369651983,-2.44572373521217,
-6.26203942766823));
#47349=CARTESIAN_POINT('Ctrl Pts',(-2.61685592304164,-2.38549877032363,
-6.26484834554482));
#47350=CARTESIAN_POINT('Ctrl Pts',(-2.67225503938364,-2.32321660732287,
-6.26765726342143));
#47351=CARTESIAN_POINT('Ctrl Pts',(-2.72538469578074,-2.25905832714279,
-6.27046618129807));
#47352=CARTESIAN_POINT('Ctrl Pts',(-2.84858346785115,-2.11028602420789,
-6.27697959125997));
#47353=CARTESIAN_POINT('Ctrl Pts',(-2.95958197207277,-1.95142785557342,
-6.28349300122203));
#47354=CARTESIAN_POINT('Ctrl Pts',(-3.05700615397888,-1.7846428881584,-6.29000641118393));
#47355=CARTESIAN_POINT('Ctrl Pts',(-3.14712345334602,-1.63036691124576,
-6.29603131079256));
#47356=CARTESIAN_POINT('Ctrl Pts',(-3.22563382835918,-1.46928943033375,
-6.30205621040104));
#47357=CARTESIAN_POINT('Ctrl Pts',(-3.29140876004433,-1.30316091650401,
-6.30808111000952));
#47358=CARTESIAN_POINT('Ctrl Pts',(-3.29674191697551,-1.28969089970129,
-6.30856962036268));
#47359=CARTESIAN_POINT('Ctrl Pts',(-3.3019913531112,-1.2761876799283,-6.30905813071584));
#47360=CARTESIAN_POINT('Ctrl Pts',(-3.30715686163083,-1.26265234730167,
-6.309546641069));
#47361=CARTESIAN_POINT('Ctrl Pts',(-3.37602965916945,-1.08218294722828,
-6.31606005103064));
#47362=CARTESIAN_POINT('Ctrl Pts',(-3.42997151868652,-0.896033422041063,
-6.32257346099227));
#47363=CARTESIAN_POINT('Ctrl Pts',(-3.46851662407281,-0.70676471783212,
-6.32908687095391));
#47364=CARTESIAN_POINT('Ctrl Pts',(-3.50706172945967,-0.517496013620443,
-6.33560028091564));
#47365=CARTESIAN_POINT('Ctrl Pts',(-3.53021639596121,-0.325084951817086,
-6.34211369087737));
#47366=CARTESIAN_POINT('Ctrl Pts',(-3.53749871140976,-0.132059280579995,
-6.34862710083908));
#47367=CARTESIAN_POINT('Ctrl Pts',(-3.53954688521147,-0.077770211989136,
-6.35045901758832));
#47368=CARTESIAN_POINT('Ctrl Pts',(-3.5403393000852,-0.0234336768277718,
-6.35229093433755));
#47369=CARTESIAN_POINT('Ctrl Pts',(-3.53986520764733,0.0308919356641406,
-6.35412285108679));
#47370=CARTESIAN_POINT('Ctrl Pts',(-3.53865365666893,0.16972192684437,-6.35880434429916));
#47371=CARTESIAN_POINT('Ctrl Pts',(-3.52917019745509,0.308480469767329,
-6.36348583751154));
#47372=CARTESIAN_POINT('Ctrl Pts',(-3.51161394105595,0.446196758891979,
-6.36816733072392));
#47373=CARTESIAN_POINT('Ctrl Pts',(-3.48718773981356,0.637802857369739,
-6.37468074068564));
#47374=CARTESIAN_POINT('Ctrl Pts',(-3.4471367782153,0.827411723408661,-6.38119415064737));
#47375=CARTESIAN_POINT('Ctrl Pts',(-3.39197035063338,1.01252418815714,-6.38770756060909));
#47376=CARTESIAN_POINT('Ctrl Pts',(-3.35680189836082,1.13053289683955,-6.39185984230308));
#47377=CARTESIAN_POINT('Ctrl Pts',(-3.31548686207736,1.2467199728331,-6.39601212399706));
#47378=CARTESIAN_POINT('Ctrl Pts',(-3.26816416858,1.3604054422155,-6.40016440569104));
#47379=CARTESIAN_POINT('Ctrl Pts',(-3.2412548792897,1.42505085771546,-6.40252553395869));
#47380=CARTESIAN_POINT('Ctrl Pts',(-3.21240318873926,1.48888742428309,-6.40488666222635));
#47381=CARTESIAN_POINT('Ctrl Pts',(-3.1816796260222,1.55180881165512,-6.407247790494));
#47382=CARTESIAN_POINT('Ctrl Pts',(-3.0969255861,1.72538379143208,-6.41376120045564));
#47383=CARTESIAN_POINT('Ctrl Pts',(-2.9979321353066,1.89198966135704,-6.42027461041727));
#47384=CARTESIAN_POINT('Ctrl Pts',(-2.88612844378586,2.04949663734564,-6.42678802037891));
#47385=CARTESIAN_POINT('Ctrl Pts',(-2.7743247522635,2.20700361333651,-6.43330143034064));
#47386=CARTESIAN_POINT('Ctrl Pts',(-2.64969465291328,2.3554295711336,-6.43981484030237));
#47387=CARTESIAN_POINT('Ctrl Pts',(-2.51368120782473,2.4925903433037,-6.44632825026408));
#47388=CARTESIAN_POINT('Ctrl Pts',(-2.37766776273814,2.62975111547182,-6.4528416602257));
#47389=CARTESIAN_POINT('Ctrl Pts',(-2.23029846571805,2.75562791640694,-6.4593550701873));
#47390=CARTESIAN_POINT('Ctrl Pts',(-2.07374054798118,2.86875662093084,-6.46586848014892));
#47391=CARTESIAN_POINT('Ctrl Pts',(-1.91718263024204,2.98188532545637,-6.47238189011064));
#47392=CARTESIAN_POINT('Ctrl Pts',(-1.7514182091273,3.08228207284204,-6.47889530007237));
#47393=CARTESIAN_POINT('Ctrl Pts',(-1.57856280904735,3.16849459675079,-6.4854087100341));
#47394=CARTESIAN_POINT('Ctrl Pts',(-1.51806293971028,3.19866921917673,-6.48768842158167));
#47395=CARTESIAN_POINT('Ctrl Pts',(-1.45669512500733,3.22710553504123,-6.48996813312925));
#47396=CARTESIAN_POINT('Ctrl Pts',(-1.39455435995192,3.25373910096334,-6.49224784467683));
#47397=CARTESIAN_POINT('Ctrl Pts',(-1.27915148859172,3.30320083480635,-6.49648154309089));
#47398=CARTESIAN_POINT('Ctrl Pts',(-1.16108267271159,3.34644458612958,-6.50071524150494));
#47399=CARTESIAN_POINT('Ctrl Pts',(-1.04106677331438,3.38331569520124,-6.504948939919));
#47400=CARTESIAN_POINT('Ctrl Pts',(-0.856426140412246,3.44004072037697,
-6.51146234988064));
#47401=CARTESIAN_POINT('Ctrl Pts',(-0.667162346706343,3.48169169421644,
-6.51797575984227));
#47402=CARTESIAN_POINT('Ctrl Pts',(-0.475768876624549,3.5077327830413,-6.52448916980391));
#47403=CARTESIAN_POINT('Ctrl Pts',(-0.340597831264554,3.5261242213556,-6.52908924541253));
#47404=CARTESIAN_POINT('Ctrl Pts',(-0.204354645869283,3.53672868968354,
-6.53368932102115));
#47405=CARTESIAN_POINT('Ctrl Pts',(-0.0679589460948733,3.53934762091083,
-6.53828939662977));
#47406=CARTESIAN_POINT('Ctrl Pts',(-0.0112271442293264,3.54043692715533,
-6.54020273098288));
#47407=CARTESIAN_POINT('Ctrl Pts',(0.045531022636131,3.54014484257323,-6.54211606533599));
#47408=CARTESIAN_POINT('Ctrl Pts',(0.102248860493038,3.53848292849331,-6.5440293996891));
#47409=CARTESIAN_POINT('Ctrl Pts',(0.295328825580803,3.53282540830823,-6.55054280965073));
#47410=CARTESIAN_POINT('Ctrl Pts',(0.487928089795479,3.51129585116066,-6.55705621961237));
#47411=CARTESIAN_POINT('Ctrl Pts',(0.677515362239871,3.47434925711893,-6.563569629574));
#47412=CARTESIAN_POINT('Ctrl Pts',(0.867102634684262,3.43740266307719,-6.57008303953564));
#47413=CARTESIAN_POINT('Ctrl Pts',(1.053701106507,3.38503272719013,-6.57659644949727));
#47414=CARTESIAN_POINT('Ctrl Pts',(1.23474298622044,3.31767899823506,-6.58310985945891));
#47415=CARTESIAN_POINT('Ctrl Pts',(1.24605820178868,3.31346935368399,-6.58351695111039));
#47416=CARTESIAN_POINT('Ctrl Pts',(1.25735159732433,3.30920121986826,-6.58392404276187));
#47417=CARTESIAN_POINT('Ctrl Pts',(1.26862254139057,3.30487470980033,-6.58433113441336));
#47418=CARTESIAN_POINT('Ctrl Pts',(1.43768513914876,3.2399776588513,-6.5904374527236));
#47419=CARTESIAN_POINT('Ctrl Pts',(1.60169567108907,3.16194539799143,-6.59654377103386));
#47420=CARTESIAN_POINT('Ctrl Pts',(1.75882144669102,3.07193280717094,-6.60265008934425));
#47421=CARTESIAN_POINT('Ctrl Pts',(1.92642237085479,2.97591932147712,-6.60916349930603));
#47422=CARTESIAN_POINT('Ctrl Pts',(2.08621238736183,2.86626604784555,-6.61567690926797));
#47423=CARTESIAN_POINT('Ctrl Pts',(2.23601720366442,2.74432457051421,-6.62219031922976));
#47424=CARTESIAN_POINT('Ctrl Pts',(2.29874823302859,2.6932613631756,-6.6249178210662));
#47425=CARTESIAN_POINT('Ctrl Pts',(2.3597278326295,2.64004307078317,-6.62764532290262));
#47426=CARTESIAN_POINT('Ctrl Pts',(2.41878915883033,2.5847744592375,-6.63037282473902));
#47427=CARTESIAN_POINT('Ctrl Pts',(2.50076921536961,2.50805887916477,-6.6341587328644));
#47428=CARTESIAN_POINT('Ctrl Pts',(2.57905316667217,2.42739285957258,-6.63794464098975));
#47429=CARTESIAN_POINT('Ctrl Pts',(2.65333228007531,2.34320336556039,-6.64173054911509));
#47430=CARTESIAN_POINT('Ctrl Pts',(2.78112468843889,2.19836078861232,-6.64824395907673));
#47431=CARTESIAN_POINT('Ctrl Pts',(2.89707465218622,2.04308253276765,-6.65475736903837));
#47432=CARTESIAN_POINT('Ctrl Pts',(2.9996904458398,1.87943880835007,-6.661270779));
#47433=CARTESIAN_POINT('Ctrl Pts',(3.07921739666291,1.75261538321336,-6.66631865335995));
#47434=CARTESIAN_POINT('Ctrl Pts',(3.15074015167961,1.62075497546953,-6.6713665277199));
#47435=CARTESIAN_POINT('Ctrl Pts',(3.21353227400634,1.48486037185928,-6.67641440207985));
#47436=CARTESIAN_POINT('Ctrl Pts',(3.23176253970101,1.44540646206153,-6.67787993768153));
#47437=CARTESIAN_POINT('Ctrl Pts',(3.2492569706675,1.40561255518628,-6.67934547328322));
#47438=CARTESIAN_POINT('Ctrl Pts',(3.26600829512753,1.36550806014452,-6.68081100888491));
#47439=CARTESIAN_POINT('Ctrl Pts',(3.34045769334387,1.18726809298532,-6.68732441884663));
#47440=CARTESIAN_POINT('Ctrl Pts',(3.4002225314738,1.00291223761149,-6.69383782880837));
#47441=CARTESIAN_POINT('Ctrl Pts',(3.44470072231061,0.814949462094048,-6.70035123877009));
#47442=CARTESIAN_POINT('Ctrl Pts',(3.48917891314677,0.626986686579336,-6.70686464873173));
#47443=CARTESIAN_POINT('Ctrl Pts',(3.51837528864164,0.435393488100818,-6.71337805869337));
#47444=CARTESIAN_POINT('Ctrl Pts',(3.53166214900558,0.242686469356258,-6.719891468655));
#47445=CARTESIAN_POINT('Ctrl Pts',(3.53340607022177,0.217393371567027,-6.7207463639057));
#47446=CARTESIAN_POINT('Ctrl Pts',(3.53487587375559,0.192081558293536,-6.7216012591564));
#47447=CARTESIAN_POINT('Ctrl Pts',(3.53607015736517,0.16675683551214,-6.7224561544071));
#47448=CARTESIAN_POINT('Ctrl Pts',(3.54397506895323,-0.000866409899313997,
-6.72811466911803));
#47449=CARTESIAN_POINT('Ctrl Pts',(3.53980817195322,-0.169055081500192,
-6.73377318382897));
#47450=CARTESIAN_POINT('Ctrl Pts',(3.52382484364409,-0.336095312099889,
-6.73943169853991));
#47451=CARTESIAN_POINT('Ctrl Pts',(3.50542673475007,-0.52837218290042,-6.74594510850164));
#47452=CARTESIAN_POINT('Ctrl Pts',(3.47137388730705,-0.719151067248053,
-6.75245851846337));
#47453=CARTESIAN_POINT('Ctrl Pts',(3.42203117938897,-0.905902528285193,
-6.75897192842508));
#47454=CARTESIAN_POINT('Ctrl Pts',(3.39797659515054,-0.99694391901358,-6.76214721764641));
#47455=CARTESIAN_POINT('Ctrl Pts',(3.37028711544748,-1.08702913815711,-6.76532250686773));
#47456=CARTESIAN_POINT('Ctrl Pts',(3.33900820913433,-1.17585040686805,-6.76849779608906));
#47457=CARTESIAN_POINT('Ctrl Pts',(3.30612529402972,-1.2692265054204,-6.77183591682935));
#47458=CARTESIAN_POINT('Ctrl Pts',(3.2692753640432,-1.3612056436035,-6.77517403756963));
#47459=CARTESIAN_POINT('Ctrl Pts',(3.2286413672435,-1.45147605409633,-6.77851215830992));
#47460=CARTESIAN_POINT('Ctrl Pts',(3.14935547553055,-1.62761353883595,-6.78502556827164));
#47461=CARTESIAN_POINT('Ctrl Pts',(3.05566316088876,-1.79725369188204,-6.79153897823337));
#47462=CARTESIAN_POINT('Ctrl Pts',(2.94886369882296,-1.95819733025196,-6.79805238819509));
#47463=CARTESIAN_POINT('Ctrl Pts',(2.85875186152997,-2.09399321043342,-6.80354806511463));
#47464=CARTESIAN_POINT('Ctrl Pts',(2.75929726145042,-2.22360994758072,-6.80904374203417));
#47465=CARTESIAN_POINT('Ctrl Pts',(2.65130325159267,-2.34567497068367,-6.81453941895371));
#47466=CARTESIAN_POINT('Ctrl Pts',(2.63130406426958,-2.36827993984675,-6.8155571519958));
#47467=CARTESIAN_POINT('Ctrl Pts',(2.61101205412421,-2.39062594672813,-6.8165748850379));
#47468=CARTESIAN_POINT('Ctrl Pts',(2.5904352191543,-2.41270682914795,-6.81759261808));
#47469=CARTESIAN_POINT('Ctrl Pts',(2.45874512329616,-2.55402270822995,-6.82410602804164));
#47470=CARTESIAN_POINT('Ctrl Pts',(2.3154071367893,-2.68446116186662,-6.83061943800327));
#47471=CARTESIAN_POINT('Ctrl Pts',(2.1624843817763,-2.80245664730059,-6.83713284796491));
#47472=CARTESIAN_POINT('Ctrl Pts',(2.00956162676109,-2.92045213273626,-6.84364625792664));
#47473=CARTESIAN_POINT('Ctrl Pts',(1.84703531539659,-3.02601956514964,-6.85015966788837));
#47474=CARTESIAN_POINT('Ctrl Pts',(1.67694939807015,-3.11757873618206,-6.8566730778501));
#47475=CARTESIAN_POINT('Ctrl Pts',(1.64293177974845,-3.13589080447667,-6.85797577649519));
#47476=CARTESIAN_POINT('Ctrl Pts',(1.60861252646917,-3.15364206036475,-6.85927847514029));
#47477=CARTESIAN_POINT('Ctrl Pts',(1.57400853431423,-3.17081963124785,-6.86058117378538));
#47478=CARTESIAN_POINT('Ctrl Pts',(1.43559477745792,-3.2395288168513,-6.86579188510192));
#47479=CARTESIAN_POINT('Ctrl Pts',(1.29262501833188,-3.29905833593406,-6.87100259641846));
#47480=CARTESIAN_POINT('Ctrl Pts',(1.14641104468838,-3.34905016806174,-6.876213307735));
#47481=CARTESIAN_POINT('Ctrl Pts',(0.963642993532519,-3.41154015793072,
-6.88272671769664));
#47482=CARTESIAN_POINT('Ctrl Pts',(0.775786184883246,-3.45913891306697,
-6.88924012765827));
#47483=CARTESIAN_POINT('Ctrl Pts',(0.585300931640267,-3.49116675003133,
-6.89575353761991));
#47484=CARTESIAN_POINT('Ctrl Pts',(0.479343748210392,-3.50898219421044,
-6.89937661374947));
#47485=CARTESIAN_POINT('Ctrl Pts',(0.372569808297704,-3.52197909098866,
-6.90299968987904));
#47486=CARTESIAN_POINT('Ctrl Pts',(0.265424692965157,-3.53003537267917,
-6.9066227660086));
#47487=CARTESIAN_POINT('Ctrl Pts',(0.1799489423262,-3.53646232665386,-6.90951309984076));
#47488=CARTESIAN_POINT('Ctrl Pts',(0.0942370119385343,-3.53974508577457,
-6.91240343367292));
#47489=CARTESIAN_POINT('Ctrl Pts',(0.00852186074184726,-3.53991094251116,
-6.91529376750508));
#47490=CARTESIAN_POINT('Ctrl Pts',(-0.184638497918042,-3.54028470311567,
-6.9218071774667));
#47491=CARTESIAN_POINT('Ctrl Pts',(-0.377816489562962,-3.52483316308227,
-6.9283205874283));
#47492=CARTESIAN_POINT('Ctrl Pts',(-0.568472409011395,-3.49386453342436,
-6.93483399739009));
#47493=CARTESIAN_POINT('Ctrl Pts',(-0.742445766719096,-3.46560568627825,
-6.94077747821385));
#47494=CARTESIAN_POINT('Ctrl Pts',(-0.914338116430782,-3.42442020539666,
-6.94672095903777));
#47495=CARTESIAN_POINT('Ctrl Pts',(-1.08216137956925,-3.37053805030733,
-6.95266443986157));
#47496=CARTESIAN_POINT('Ctrl Pts',(-1.09825419967799,-3.36537121102231,
-6.95323436899969));
#47497=CARTESIAN_POINT('Ctrl Pts',(-1.11430960469959,-3.3600876333587,-6.95380429813781));
#47498=CARTESIAN_POINT('Ctrl Pts',(-1.13032604705382,-3.35468816325393,
-6.95437422727593));
#47499=CARTESIAN_POINT('Ctrl Pts',(-1.31336925050718,-3.29298055784017,
-6.96088763723773));
#47500=CARTESIAN_POINT('Ctrl Pts',(-1.49129514513555,-3.21614619228149,
-6.96740104719937));
#47501=CARTESIAN_POINT('Ctrl Pts',(-1.66183108821857,-3.12544975106934,
-6.973914457161));
#47502=CARTESIAN_POINT('Ctrl Pts',(-1.83236703130161,-3.0347533098572,-6.98042786712264));
#47503=CARTESIAN_POINT('Ctrl Pts',(-1.99553483595644,-2.93018474734963,
-6.98694127708427));
#47504=CARTESIAN_POINT('Ctrl Pts',(-2.14907398699859,-2.81297668049842,
-6.99345468704591));
#47505=CARTESIAN_POINT('Ctrl Pts',(-2.19033810662407,-2.78147665162115,
-6.99520518602941));
#47506=CARTESIAN_POINT('Ctrl Pts',(-2.23090577145553,-2.74906427885111,
-6.99695568501291));
#47507=CARTESIAN_POINT('Ctrl Pts',(-2.27073169575485,-2.71576463742649,
-6.99870618399641));
#47508=CARTESIAN_POINT('Ctrl Pts',(-2.37909355934424,-2.62516005598574,
-7.00346909497464));
#47509=CARTESIAN_POINT('Ctrl Pts',(-2.48196353080434,-2.52798626286371,
-7.00823200595286));
#47510=CARTESIAN_POINT('Ctrl Pts',(-2.57868524344307,-2.42505371417111,
-7.01299491693108));
#47511=CARTESIAN_POINT('Ctrl Pts',(-2.71095480915343,-2.28429066168171,
-7.0195083268927));
#47512=CARTESIAN_POINT('Ctrl Pts',(-2.83174365337413,-2.13274635689841,
-7.0260217368543));
#47513=CARTESIAN_POINT('Ctrl Pts',(-2.93944340626971,-1.97240050926644,
-7.03253514681592));
#47514=CARTESIAN_POINT('Ctrl Pts',(-3.00675548551217,-1.8721847509957,-7.03660601193573));
#47515=CARTESIAN_POINT('Ctrl Pts',(-3.0689565651283,-1.76852498435215,-7.04067687705556));
#47516=CARTESIAN_POINT('Ctrl Pts',(-3.12563447872083,-1.66192933226244,
-7.04474774217538));
#47517=CARTESIAN_POINT('Ctrl Pts',(-3.15964158566754,-1.59797126622053,
-7.04719028701728));
#47518=CARTESIAN_POINT('Ctrl Pts',(-3.19166042350247,-1.53295634899612,
-7.04963283185919));
#47519=CARTESIAN_POINT('Ctrl Pts',(-3.22164958182273,-1.467019693314,-7.0520753767011));
#47520=CARTESIAN_POINT('Ctrl Pts',(-3.30162014334238,-1.29118977093615,
-7.05858878666273));
#47521=CARTESIAN_POINT('Ctrl Pts',(-3.36715796958855,-1.10881135569454,
-7.06510219662437));
#47522=CARTESIAN_POINT('Ctrl Pts',(-3.41752451187652,-0.92233949801837,
-7.071615606586));
#47523=CARTESIAN_POINT('Ctrl Pts',(-3.46694667627976,-0.739364006987898,
-7.07800688943621));
#47524=CARTESIAN_POINT('Ctrl Pts',(-3.50176440608703,-0.552424156172237,
-7.08439817228643));
#47525=CARTESIAN_POINT('Ctrl Pts',(-3.52124797259483,-0.363885580226897,
-7.09078945513664));
#47526=CARTESIAN_POINT('Ctrl Pts',(-3.52162027213994,-0.360282911997128,
-7.09091158224806));
#47527=CARTESIAN_POINT('Ctrl Pts',(-3.52198697295808,-0.35667966015706,
-7.09103370935948));
#47528=CARTESIAN_POINT('Ctrl Pts',(-3.52234807653483,-0.353075841902743,
-7.09115583647091));
#47529=CARTESIAN_POINT('Ctrl Pts',(-3.54160682757397,-0.160873263421083,
-7.09766924643264));
#47530=CARTESIAN_POINT('Ctrl Pts',(-3.54494113425226,0.0329083541594109,
-7.10418265639437));
#47531=CARTESIAN_POINT('Ctrl Pts',(-3.53259533909181,0.22566737745008,-7.11069606635609));
#47532=CARTESIAN_POINT('Ctrl Pts',(-3.52024954393154,0.418426400737956,
-7.11720947631773));
#47533=CARTESIAN_POINT('Ctrl Pts',(-3.49222452843905,0.610186888018826,
-7.12372288627936));
#47534=CARTESIAN_POINT('Ctrl Pts',(-3.44874073224416,0.798391072008908,
-7.130236296241));
#47535=CARTESIAN_POINT('Ctrl Pts',(-3.43406482543378,0.861910527697223,
-7.13243459091578));
#47536=CARTESIAN_POINT('Ctrl Pts',(-3.4176279918563,0.925023822733724,-7.13463288559057));
#47537=CARTESIAN_POINT('Ctrl Pts',(-3.399439647296,0.987628515379085,-7.13683118026536));
#47538=CARTESIAN_POINT('Ctrl Pts',(-3.36373706176239,1.11051762090298,-7.14114629555221));
#47539=CARTESIAN_POINT('Ctrl Pts',(-3.32128518726173,1.23144678337572,-7.14546141083906));
#47540=CARTESIAN_POINT('Ctrl Pts',(-3.27244048985516,1.34972428826295,-7.14977652612591));
#47541=CARTESIAN_POINT('Ctrl Pts',(-3.19871232327865,1.52825714946575,-7.15628993608764));
#47542=CARTESIAN_POINT('Ctrl Pts',(-3.11041628697104,1.7007662450445,-7.16280334604937));
#47543=CARTESIAN_POINT('Ctrl Pts',(-3.00872059248994,1.86498453844867,-7.16931675601108));
#47544=CARTESIAN_POINT('Ctrl Pts',(-2.9381695165832,1.97891047545466,-7.17383541418009));
#47545=CARTESIAN_POINT('Ctrl Pts',(-2.86116271344563,2.08885271017646,-7.1783540723491));
#47546=CARTESIAN_POINT('Ctrl Pts',(-2.77810835168668,2.19401777255465,-7.18287273051811));
#47547=CARTESIAN_POINT('Ctrl Pts',(-2.74144418484653,2.24044265995526,-7.18486748231071));
#47548=CARTESIAN_POINT('Ctrl Pts',(-2.70360160799484,2.2859366567572,-7.18686223410332));
#47549=CARTESIAN_POINT('Ctrl Pts',(-2.66463875530979,2.33044965099088,-7.18885698589592));
#47550=CARTESIAN_POINT('Ctrl Pts',(-2.53741438897186,2.47579674687627,-7.19537039585764));
#47551=CARTESIAN_POINT('Ctrl Pts',(-2.39825532545772,2.61067669790369,-7.20188380581937));
#47552=CARTESIAN_POINT('Ctrl Pts',(-2.24911868144474,2.73342304268973,-7.20839721578109));
#47553=CARTESIAN_POINT('Ctrl Pts',(-2.09998203743392,2.85616938747399,-7.21491062574273));
#47554=CARTESIAN_POINT('Ctrl Pts',(-1.94084807500285,2.96679585561946,-7.22142403570437));
#47555=CARTESIAN_POINT('Ctrl Pts',(-1.7736881360114,3.06359595272342,-7.227937445666));
#47556=CARTESIAN_POINT('Ctrl Pts',(-1.76533007352107,3.0684359955324,-7.22826311871789));
#47557=CARTESIAN_POINT('Ctrl Pts',(-1.75695201419097,3.07324143239533,-7.22858879176977));
#47558=CARTESIAN_POINT('Ctrl Pts',(-1.74855420770786,3.07801205044834,-7.22891446482166));
#47559=CARTESIAN_POINT('Ctrl Pts',(-1.58899720157694,3.16865304526785,-7.23510220173141));
#47560=CARTESIAN_POINT('Ctrl Pts',(-1.42231138155771,3.24672375067996,-7.24128993864116));
#47561=CARTESIAN_POINT('Ctrl Pts',(-1.25063380441199,3.31151429393604,-7.24747767555091));
#47562=CARTESIAN_POINT('Ctrl Pts',(-1.0699204907246,3.37971489393329,-7.25399108551264));
#47563=CARTESIAN_POINT('Ctrl Pts',(-0.883654985072044,3.43321218577804,
-7.26050449547437));
#47564=CARTESIAN_POINT('Ctrl Pts',(-0.69426261018899,3.47118330719089,-7.2670179054361));
#47565=CARTESIAN_POINT('Ctrl Pts',(-0.61732158273511,3.48660915047991,-7.26966399113513));
#47566=CARTESIAN_POINT('Ctrl Pts',(-0.539864762333473,3.49947197571339,
-7.27231007683416));
#47567=CARTESIAN_POINT('Ctrl Pts',(-0.462062720458959,3.5097148092635,-7.2749561625332));
#47568=CARTESIAN_POINT('Ctrl Pts',(-0.34835297767497,3.52468498151477,-7.27882348679582));
#47569=CARTESIAN_POINT('Ctrl Pts',(-0.233905849409282,3.53405841436472,
-7.28269081105846));
#47570=CARTESIAN_POINT('Ctrl Pts',(-0.119281726467647,3.53786972306194,
-7.28655813532117));
#47571=CARTESIAN_POINT('Ctrl Pts',(0.0737700720151849,3.54428879070397,
-7.29307154528297));
#47572=CARTESIAN_POINT('Ctrl Pts',(0.267337123262925,3.53493519022353,-7.29958495524494));
#47573=CARTESIAN_POINT('Ctrl Pts',(0.45887316707087,3.50996979757638,-7.30609836520674));
#47574=CARTESIAN_POINT('Ctrl Pts',(0.604918840965994,3.49093375861096,-7.31106482127587));
#47575=CARTESIAN_POINT('Ctrl Pts',(0.749795644587637,3.46281672251746,-7.3160312773449));
#47576=CARTESIAN_POINT('Ctrl Pts',(0.892325528180709,3.42569046350633,-7.3209977334139));
#47577=CARTESIAN_POINT('Ctrl Pts',(0.936720798206521,3.4141263602299,-7.32254468730663));
#47578=CARTESIAN_POINT('Ctrl Pts',(0.98088838046976,3.40168827258433,-7.32409164119935));
#47579=CARTESIAN_POINT('Ctrl Pts',(1.02479609483758,3.38839156064891,-7.32563859509208));
#47580=CARTESIAN_POINT('Ctrl Pts',(1.2096684077747,3.33240609373605,-7.3321520050537));
#47581=CARTESIAN_POINT('Ctrl Pts',(1.38991621050558,3.26120588847558,-7.3386654150153));
#47582=CARTESIAN_POINT('Ctrl Pts',(1.56321999725237,3.17591743890142,-7.34517882497692));
#47583=CARTESIAN_POINT('Ctrl Pts',(1.73652378400167,3.09062898932603,-7.35169223493864));
#47584=CARTESIAN_POINT('Ctrl Pts',(1.90290467519647,2.99124089947101,-7.35820564490037));
#47585=CARTESIAN_POINT('Ctrl Pts',(2.06001785169516,2.87886643810324,-7.3647190548621));
#47586=CARTESIAN_POINT('Ctrl Pts',(2.07867525608196,2.86552181726869,-7.3654925311949));
#47587=CARTESIAN_POINT('Ctrl Pts',(2.09720163827227,2.85199428966467,-7.3662660075277));
#47588=CARTESIAN_POINT('Ctrl Pts',(2.11559302029352,2.83828578062299,-7.3670394838605));
#47589=CARTESIAN_POINT('Ctrl Pts',(2.25207465220354,2.73655554181339,-7.37277941748934));
#47590=CARTESIAN_POINT('Ctrl Pts',(2.38112092105923,2.62485779238668,-7.37851935111817));
#47591=CARTESIAN_POINT('Ctrl Pts',(2.50151996034344,2.50453286898932,-7.384259284747));
#47592=CARTESIAN_POINT('Ctrl Pts',(2.63814319548082,2.36799373711636,-7.39077269470864));
#47593=CARTESIAN_POINT('Ctrl Pts',(2.76365118020096,2.22033192223027,-7.39728610467027));
#47594=CARTESIAN_POINT('Ctrl Pts',(2.87632012344211,2.06343515614491,-7.40379951463191));
#47595=CARTESIAN_POINT('Ctrl Pts',(2.92983793594804,1.98890910248192,-7.40689338809049));
#47596=CARTESIAN_POINT('Ctrl Pts',(2.98045881580538,1.91229818395693,-7.40998726154908));
#47597=CARTESIAN_POINT('Ctrl Pts',(3.02798948096801,1.83381561318099,-7.41308113500767));
#47598=CARTESIAN_POINT('Ctrl Pts',(3.08052325350839,1.74707191819124,-7.41650067151081));
#47599=CARTESIAN_POINT('Ctrl Pts',(3.12928194035441,1.65804182176638,-7.41992020801395));
#47600=CARTESIAN_POINT('Ctrl Pts',(3.17413145383252,1.5670900227261,-7.4233397445171));
#47601=CARTESIAN_POINT('Ctrl Pts',(3.25955919165442,1.39384831194062,-7.42985315447873));
#47602=CARTESIAN_POINT('Ctrl Pts',(3.33081116461456,1.21362870349055,-7.43636656444037));
#47603=CARTESIAN_POINT('Ctrl Pts',(3.38701269619474,1.02883041976208,-7.442879974402));
#47604=CARTESIAN_POINT('Ctrl Pts',(3.43373009893555,0.87521724225577,-7.44829423248071));
#47605=CARTESIAN_POINT('Ctrl Pts',(3.47004976409285,0.718424299931465,-7.45370849055942));
#47606=CARTESIAN_POINT('Ctrl Pts',(3.49544487589833,0.559879558080886,-7.45912274863812));
#47607=CARTESIAN_POINT('Ctrl Pts',(3.50060035326059,0.527693291929511,-7.46022190052105));
#47608=CARTESIAN_POINT('Ctrl Pts',(3.50530563687768,0.495434842487014,-7.46132105240398));
#47609=CARTESIAN_POINT('Ctrl Pts',(3.50956112158859,0.463116931447565,-7.46242020428691));
#47610=CARTESIAN_POINT('Ctrl Pts',(3.53477848866818,0.271605815489876,-7.46893361424864));
#47611=CARTESIAN_POINT('Ctrl Pts',(3.54419862852173,0.0780313815552228,
-7.47544702421037));
#47612=CARTESIAN_POINT('Ctrl Pts',(3.53792067981413,-0.115020209061044,
-7.48196043417208));
#47613=CARTESIAN_POINT('Ctrl Pts',(3.53164273110663,-0.308071799674505,
-7.4884738441337));
#47614=CARTESIAN_POINT('Ctrl Pts',(3.50966604727128,-0.500624506508935,
-7.4949872540953));
#47615=CARTESIAN_POINT('Ctrl Pts',(3.47206668295341,-0.690093950472241,
-7.50150066405692));
#47616=CARTESIAN_POINT('Ctrl Pts',(3.46501671280743,-0.725619921396251,
-7.50272194390064));
#47617=CARTESIAN_POINT('Ctrl Pts',(3.45741761512174,-0.761036669986838,
-7.50394322374436));
#47618=CARTESIAN_POINT('Ctrl Pts',(3.44927002934,-0.796326732377223,-7.50516450358807));
#47619=CARTESIAN_POINT('Ctrl Pts',(3.41396437492646,-0.949247951050361,
-7.51045663370608));
#47620=CARTESIAN_POINT('Ctrl Pts',(3.36835867813816,-1.09978996669337,-7.51574876382412));
#47621=CARTESIAN_POINT('Ctrl Pts',(3.31303614425419,-1.24665390493681,-7.52104089394225));
#47622=CARTESIAN_POINT('Ctrl Pts',(3.24494668166318,-1.42741002594109,-7.52755430304353));
#47623=CARTESIAN_POINT('Ctrl Pts',(3.16213450723209,-1.60261747901651,-7.53406771214497));
#47624=CARTESIAN_POINT('Ctrl Pts',(3.06563512605655,-1.76994523770567,-7.54058112124546));
#47625=CARTESIAN_POINT('',(-1.368080573303,-3.758770483144,-4.441666666667));
#47626=CARTESIAN_POINT('Ctrl Pts',(-3.361449115544,-1.040542320116,-2.023855154456));
#47627=CARTESIAN_POINT('Ctrl Pts',(-3.495234334804,-0.6083521071266,-2.039202376679));
#47628=CARTESIAN_POINT('Ctrl Pts',(-3.593966410624,0.3080871692045,-2.069896821123));
#47629=CARTESIAN_POINT('Ctrl Pts',(-3.214002747139,1.6376218606,-2.11593848779));
#47630=CARTESIAN_POINT('Ctrl Pts',(-2.361752530656,2.726480536661,-2.161980154456));
#47631=CARTESIAN_POINT('Ctrl Pts',(-1.162463196152,3.414713247338,-2.208021821123));
#47632=CARTESIAN_POINT('Ctrl Pts',(0.2076425386167,3.6011758161,-2.25406348779));
#47633=CARTESIAN_POINT('Ctrl Pts',(1.5472364757,3.258472506991,-2.300105154456));
#47634=CARTESIAN_POINT('Ctrl Pts',(2.659475311144,2.436960122203,-2.346146821123));
#47635=CARTESIAN_POINT('Ctrl Pts',(3.380923545207,1.257354198423,-2.39218848779));
#47636=CARTESIAN_POINT('Ctrl Pts',(3.605569620214,-0.1070108088044,-2.438230154456));
#47637=CARTESIAN_POINT('Ctrl Pts',(3.300403421044,-1.455651350858,-2.484271821123));
#47638=CARTESIAN_POINT('Ctrl Pts',(2.510266906159,-2.590394498517,-2.53031348779));
#47639=CARTESIAN_POINT('Ctrl Pts',(1.351264898242,-3.344497985119,-2.576355154456));
#47640=CARTESIAN_POINT('Ctrl Pts',(-0.006295673909096,-3.607151779769,-2.622396821123));
#47641=CARTESIAN_POINT('Ctrl Pts',(-1.362931142503,-3.339760814575,-2.66843848779));
#47642=CARTESIAN_POINT('Ctrl Pts',(-2.519293776961,-2.581616250171,-2.714480154456));
#47643=CARTESIAN_POINT('Ctrl Pts',(-3.305464485361,-1.444121924838,-2.760521821123));
#47644=CARTESIAN_POINT('Ctrl Pts',(-3.605921191072,-0.09442436949411,-2.80656348779));
#47645=CARTESIAN_POINT('Ctrl Pts',(-3.376513963031,1.269148161262,-2.852605154456));
#47646=CARTESIAN_POINT('Ctrl Pts',(-2.650952527502,2.446228585948,-2.898646821123));
#47647=CARTESIAN_POINT('Ctrl Pts',(-1.535852868594,3.263853483815,-2.94468848779));
#47648=CARTESIAN_POINT('Ctrl Pts',(-0.1950707836154,3.601878813503,-2.990730154456));
#47649=CARTESIAN_POINT('Ctrl Pts',(1.174375536461,3.410634207467,-3.036771821123));
#47650=CARTESIAN_POINT('Ctrl Pts',(2.371255899469,2.718221671795,-3.08281348779));
#47651=CARTESIAN_POINT('Ctrl Pts',(3.219697427502,1.626386200482,-3.128855154456));
#47652=CARTESIAN_POINT('Ctrl Pts',(3.595027799181,0.2955650874075,-3.174896821123));
#47653=CARTESIAN_POINT('Ctrl Pts',(3.442094941941,-1.078687168943,-3.22093848779));
#47654=CARTESIAN_POINT('Ctrl Pts',(2.783371228594,-2.294434178968,-3.266980154456));
#47655=CARTESIAN_POINT('Ctrl Pts',(1.715651325333,-3.173030747985,-3.313021821123));
#47656=CARTESIAN_POINT('Ctrl Pts',(0.3958289184352,-3.585373490323,-3.35906348779));
#47657=CARTESIAN_POINT('Ctrl Pts',(-0.9821576736188,-3.470871634321,-3.405105154456));
#47658=CARTESIAN_POINT('Ctrl Pts',(-2.215823327712,-2.846350396235,-3.451146821123));
#47659=CARTESIAN_POINT('Ctrl Pts',(-3.123889834539,-1.80357863689,-3.49718848779));
#47660=CARTESIAN_POINT('Ctrl Pts',(-3.572923415067,-0.4957840939792,-3.543230154456));
#47661=CARTESIAN_POINT('Ctrl Pts',(-3.496941845406,0.8848623212845,-3.589271821123));
#47662=CARTESIAN_POINT('Ctrl Pts',(-2.907110065457,2.135484644079,-3.63531348779));
#47663=CARTESIAN_POINT('Ctrl Pts',(-1.890099572078,3.072313005768,-3.681355154456));
#47664=CARTESIAN_POINT('Ctrl Pts',(-0.5953526720002,3.557687281609,-3.727396821123));
#47665=CARTESIAN_POINT('Ctrl Pts',(0.7868769799293,3.520285246431,-3.77343848779));
#47666=CARTESIAN_POINT('Ctrl Pts',(2.053480773757,2.965602857698,-3.819480154456));
#47667=CARTESIAN_POINT('Ctrl Pts',(3.018340479732,1.975146664475,-3.865521821123));
#47668=CARTESIAN_POINT('Ctrl Pts',(3.539676970626,0.6944570119162,-3.91156348779));
#47669=CARTESIAN_POINT('Ctrl Pts',(3.540883634913,-0.688278055575,-3.957605154456));
#47670=CARTESIAN_POINT('Ctrl Pts',(3.021783162039,-1.969875660898,-4.003646821123));
#47671=CARTESIAN_POINT('Ctrl Pts',(2.058653596917,-2.962014342585,-4.04968848779));
#47672=CARTESIAN_POINT('Ctrl Pts',(0.7930198351441,-3.518906526017,-4.095730154456));
#47673=CARTESIAN_POINT('Ctrl Pts',(-0.5891424326969,-3.558720948849,-4.141771821123));
#47674=CARTESIAN_POINT('Ctrl Pts',(-1.884734498254,-3.075607170766,-4.18781348779));
#47675=CARTESIAN_POINT('Ctrl Pts',(-2.903378515752,-2.140555253211,-4.233855154456));
#47676=CARTESIAN_POINT('Ctrl Pts',(-3.495392143951,-0.890964285359,-4.279896821123));
#47677=CARTESIAN_POINT('Ctrl Pts',(-3.573783279237,0.4895474142708,-4.32593848779));
#47678=CARTESIAN_POINT('Ctrl Pts',(-3.127032913541,1.798123676345,-4.371980154456));
#47679=CARTESIAN_POINT('Ctrl Pts',(-2.220787768898,2.842478721679,-4.418021821123));
#47680=CARTESIAN_POINT('Ctrl Pts',(-0.9882139884594,3.469152160271,-4.46406348779));
#47681=CARTESIAN_POINT('Ctrl Pts',(0.3895706616256,3.58605888079,-4.510105154456));
#47682=CARTESIAN_POINT('Ctrl Pts',(1.710110731203,3.176020290621,-4.556146821123));
#47683=CARTESIAN_POINT('Ctrl Pts',(2.779362449993,2.299288579191,-4.60218848779));
#47684=CARTESIAN_POINT('Ctrl Pts',(3.440207029409,1.084693119086,-4.648230154456));
#47685=CARTESIAN_POINT('Ctrl Pts',(3.595538206437,-0.2892901598772,-4.694271821123));
#47686=CARTESIAN_POINT('Ctrl Pts',(3.222531009545,-1.620764194701,-4.74031348779));
#47687=CARTESIAN_POINT('Ctrl Pts',(2.375996820758,-2.714079282501,-4.786355154456));
#47688=CARTESIAN_POINT('Ctrl Pts',(1.180325142345,-3.408577957331,-4.832396821123));
#47689=CARTESIAN_POINT('Ctrl Pts',(-0.1887792404969,-3.602218957155,-4.87843848779));
#47690=CARTESIAN_POINT('Ctrl Pts',(-1.530171890201,-3.26650979655,-4.924480154456));
#47691=CARTESIAN_POINT('Ctrl Pts',(-2.27446554662,-2.722785672557,-4.955174598901));
#47692=CARTESIAN_POINT('Ctrl Pts',(-2.581860640706,-2.390829167532,-4.970521821123));
#47693=CARTESIAN_POINT('Ctrl Pts',(-3.521415988649,-1.090060339149,-2.120535787988));
#47694=CARTESIAN_POINT('Ctrl Pts',(-3.66156786778,-0.6373027712535,-2.13588301021));
#47695=CARTESIAN_POINT('Ctrl Pts',(-3.764998471199,0.3227486260367,-2.166577454654));
#47696=CARTESIAN_POINT('Ctrl Pts',(-3.366952844534,1.715554097372,-2.212619121321));
#47697=CARTESIAN_POINT('Ctrl Pts',(-2.474145178704,2.856230103303,-2.258660787988));
#47698=CARTESIAN_POINT('Ctrl Pts',(-1.217783266811,3.577214889324,-2.304702454654));
#47699=CARTESIAN_POINT('Ctrl Pts',(0.2175239696557,3.772550962651,-2.350744121321));
#47700=CARTESIAN_POINT('Ctrl Pts',(1.620867392743,3.413538860853,-2.396785787988));
#47701=CARTESIAN_POINT('Ctrl Pts',(2.78603618861,2.552931799069,-2.442827454654));
#47702=CARTESIAN_POINT('Ctrl Pts',(3.541817180406,1.317190005122,-2.488869121321));
#47703=CARTESIAN_POINT('Ctrl Pts',(3.777153862034,-0.1121033102479,-2.534910787988));
#47704=CARTESIAN_POINT('Ctrl Pts',(3.457465211094,-1.524923854152,-2.580952454654));
#47705=CARTESIAN_POINT('Ctrl Pts',(2.629727154949,-2.71366791239,-2.626994121321));
#47706=CARTESIAN_POINT('Ctrl Pts',(1.415569789697,-3.50365817657,-2.673035787988));
#47707=CARTESIAN_POINT('Ctrl Pts',(-0.006595276620518,-3.778811314449,-2.719077454654));
#47708=CARTESIAN_POINT('Ctrl Pts',(-1.427791214939,-3.498695570408,-2.765119121321));
#47709=CARTESIAN_POINT('Ctrl Pts',(-2.639183602474,-2.704471918932,-2.811160787988));
#47710=CARTESIAN_POINT('Ctrl Pts',(-3.462767124701,-1.512845758149,-2.857202454654));
#47711=CARTESIAN_POINT('Ctrl Pts',(-3.77752216368,-0.09891789910402,-2.903244121321));
#47712=CARTESIAN_POINT('Ctrl Pts',(-3.537197752104,1.329545226898,-2.949285787988));
#47713=CARTESIAN_POINT('Ctrl Pts',(-2.77710781708,2.562641336623,-2.995327454654));
#47714=CARTESIAN_POINT('Ctrl Pts',(-1.608942054981,3.419175911177,-3.041369121321));
#47715=CARTESIAN_POINT('Ctrl Pts',(-0.2043539416274,3.773287414762,-3.087410787988));
#47716=CARTESIAN_POINT('Ctrl Pts',(1.230262499482,3.572941733393,-3.133452454654));
#47717=CARTESIAN_POINT('Ctrl Pts',(2.484100800144,2.84757821009,-3.179494121321));
#47718=CARTESIAN_POINT('Ctrl Pts',(3.372918527128,1.703783747197,-3.225535787988));
#47719=CARTESIAN_POINT('Ctrl Pts',(3.76611036982,0.3096306350943,-3.271577454654));
#47720=CARTESIAN_POINT('Ctrl Pts',(3.605899642196,-1.130020450377,-3.317619121321));
#47721=CARTESIAN_POINT('Ctrl Pts',(2.915828147269,-2.403623236585,-3.363660787988));
#47722=CARTESIAN_POINT('Ctrl Pts',(1.797296880098,-3.324031042672,-3.409702454654));
#47723=CARTESIAN_POINT('Ctrl Pts',(0.4146658879059,-3.7559966253,-3.455744121321));
#47724=CARTESIAN_POINT('Ctrl Pts',(-1.028897245317,-3.636045778925,-3.501785787988));
#47725=CARTESIAN_POINT('Ctrl Pts',(-2.321271399928,-2.981804409369,-3.547827454654));
#47726=CARTESIAN_POINT('Ctrl Pts',(-3.272551578798,-1.889408534956,-3.593869121321));
#47727=CARTESIAN_POINT('Ctrl Pts',(-3.742954067594,-0.5193777967315,-3.639910787988));
#47728=CARTESIAN_POINT('Ctrl Pts',(-3.66335663653,0.9269717371343,-3.685952454654));
#47729=CARTESIAN_POINT('Ctrl Pts',(-3.045455550085,2.237109505659,-3.731994121321));
#47730=CARTESIAN_POINT('Ctrl Pts',(-1.980046885873,3.218520277643,-3.778035787988));
#47731=CARTESIAN_POINT('Ctrl Pts',(-0.6236847103744,3.726992866897,-3.824077454654));
#47732=CARTESIAN_POINT('Ctrl Pts',(0.8243234042752,3.687810918827,-3.870119121321));
#47733=CARTESIAN_POINT('Ctrl Pts',(2.151203180692,3.106731936173,-3.916160787988));
#47734=CARTESIAN_POINT('Ctrl Pts',(3.161979271192,2.06914125579,-3.962202454654));
#47735=CARTESIAN_POINT('Ctrl Pts',(3.708125469273,0.7275052934411,-4.008244121321));
#47736=CARTESIAN_POINT('Ctrl Pts',(3.709389557102,-0.7210322888216,-4.054285787988));
#47737=CARTESIAN_POINT('Ctrl Pts',(3.16558578615,-2.063619412194,-4.100327454654));
#47738=CARTESIAN_POINT('Ctrl Pts',(2.156622171596,-3.102972648419,-4.146369121321));
#47739=CARTESIAN_POINT('Ctrl Pts',(0.8307585897638,-3.686366586951,-4.192410787987));
#47740=CARTESIAN_POINT('Ctrl Pts',(-0.6171789340784,-3.72807572498,-4.238452454654));
#47741=CARTESIAN_POINT('Ctrl Pts',(-1.974426495353,-3.221971207554,-4.284494121321));
#47742=CARTESIAN_POINT('Ctrl Pts',(-3.041546420915,-2.242421418306,-4.330535787987));
#47743=CARTESIAN_POINT('Ctrl Pts',(-3.661733186854,-0.9333640855279,-4.376577454654));
#47744=CARTESIAN_POINT('Ctrl Pts',(-3.743854851551,0.5128443217669,-4.422619121321));
#47745=CARTESIAN_POINT('Ctrl Pts',(-3.275844232732,1.883693980126,-4.468660787987));
#47746=CARTESIAN_POINT('Ctrl Pts',(-2.326472092238,2.977748486993,-4.514702454654));
#47747=CARTESIAN_POINT('Ctrl Pts',(-1.03524177209,3.634244477402,-4.560744121321));
#47748=CARTESIAN_POINT('Ctrl Pts',(0.4081098090146,3.756714632584,-4.606785787988));
#47749=CARTESIAN_POINT('Ctrl Pts',(1.791492616494,3.327162853648,-4.652827454654));
#47750=CARTESIAN_POINT('Ctrl Pts',(2.911628596249,2.40870865123,-4.698869121321));
#47751=CARTESIAN_POINT('Ctrl Pts',(3.603921886428,1.136312215665,-4.744910787988));
#47752=CARTESIAN_POINT('Ctrl Pts',(3.766645066676,-0.303057092145,-4.790952454654));
#47753=CARTESIAN_POINT('Ctrl Pts',(3.375886955555,-1.697894197672,-4.836994121321));
#47754=CARTESIAN_POINT('Ctrl Pts',(2.489067335545,-2.843238690024,-4.883035787988));
#47755=CARTESIAN_POINT('Ctrl Pts',(1.236495239162,-3.570787629061,-4.929077454654));
#47756=CARTESIAN_POINT('Ctrl Pts',(-0.1977629923763,-3.773643745397,-4.975119121321));
#47757=CARTESIAN_POINT('Ctrl Pts',(-1.602990726415,-3.421958634286,-5.021160787987));
#47758=CARTESIAN_POINT('Ctrl Pts',(-2.382704323698,-2.852359405552,-5.051855232432));
#47759=CARTESIAN_POINT('Ctrl Pts',(-2.704727939686,-2.504605533888,-5.067202454654));
#47760=CARTESIAN_POINT('Ctrl Pts',(-3.681382861754,-1.139578358183,-2.217216421519));
#47761=CARTESIAN_POINT('Ctrl Pts',(-3.827901400756,-0.6662534353805,-2.232563643741));
#47762=CARTESIAN_POINT('Ctrl Pts',(-3.936030531775,0.337410082869,-2.263258088185));
#47763=CARTESIAN_POINT('Ctrl Pts',(-3.519902941929,1.793486334144,-2.309299754852));
#47764=CARTESIAN_POINT('Ctrl Pts',(-2.586537826753,2.985979669946,-2.355341421519));
#47765=CARTESIAN_POINT('Ctrl Pts',(-1.27310333747,3.739716531309,-2.401383088185));
#47766=CARTESIAN_POINT('Ctrl Pts',(0.2274054006946,3.943926109203,-2.447424754852));
#47767=CARTESIAN_POINT('Ctrl Pts',(1.694498309787,3.568605214716,-2.493466421519));
#47768=CARTESIAN_POINT('Ctrl Pts',(2.912597066077,2.668903475936,-2.539508088185));
#47769=CARTESIAN_POINT('Ctrl Pts',(3.702710815604,1.377025811821,-2.585549754852));
#47770=CARTESIAN_POINT('Ctrl Pts',(3.948738103854,-0.1171958116913,-2.631591421519));
#47771=CARTESIAN_POINT('Ctrl Pts',(3.614527001144,-1.594196357445,-2.677633088185));
#47772=CARTESIAN_POINT('Ctrl Pts',(2.749187403738,-2.836941326264,-2.723674754852));
#47773=CARTESIAN_POINT('Ctrl Pts',(1.479874681153,-3.662818368022,-2.769716421519));
#47774=CARTESIAN_POINT('Ctrl Pts',(-0.006894879331943,-3.950470849129,-2.815758088185));
#47775=CARTESIAN_POINT('Ctrl Pts',(-1.492651287375,-3.657630326242,-2.861799754852));
#47776=CARTESIAN_POINT('Ctrl Pts',(-2.759073427987,-2.827327587693,-2.907841421519));
#47777=CARTESIAN_POINT('Ctrl Pts',(-3.620069764041,-1.581569591459,-2.953883088185));
#47778=CARTESIAN_POINT('Ctrl Pts',(-3.949123136288,-0.1034114287139,-2.999924754852));
#47779=CARTESIAN_POINT('Ctrl Pts',(-3.697881541177,1.389942292534,-3.045966421519));
#47780=CARTESIAN_POINT('Ctrl Pts',(-2.903263106658,2.679054087298,-3.092008088185));
#47781=CARTESIAN_POINT('Ctrl Pts',(-1.682031241369,3.574498338538,-3.138049754852));
#47782=CARTESIAN_POINT('Ctrl Pts',(-0.2136370996395,3.944696016021,-3.184091421519));
#47783=CARTESIAN_POINT('Ctrl Pts',(1.286149462504,3.73524925932,-3.230133088185));
#47784=CARTESIAN_POINT('Ctrl Pts',(2.59694570082,2.976934748386,-3.276174754852));
#47785=CARTESIAN_POINT('Ctrl Pts',(3.526139626754,1.781181293913,-3.322216421519));
#47786=CARTESIAN_POINT('Ctrl Pts',(3.93719294046,0.3236961827811,-3.368258088185));
#47787=CARTESIAN_POINT('Ctrl Pts',(3.76970434245,-1.181353731811,-3.414299754852));
#47788=CARTESIAN_POINT('Ctrl Pts',(3.048285065944,-2.512812294202,-3.460341421519));
#47789=CARTESIAN_POINT('Ctrl Pts',(1.878942434863,-3.475031337359,-3.506383088185));
#47790=CARTESIAN_POINT('Ctrl Pts',(0.4335028573765,-3.926619760277,-3.552424754852));
#47791=CARTESIAN_POINT('Ctrl Pts',(-1.075636817015,-3.801219923529,-3.598466421519));
#47792=CARTESIAN_POINT('Ctrl Pts',(-2.426719472144,-3.117258422503,-3.644508088185));
#47793=CARTESIAN_POINT('Ctrl Pts',(-3.421213323057,-1.975238433022,-3.690549754852));
#47794=CARTESIAN_POINT('Ctrl Pts',(-3.912984720121,-0.5429714994837,-3.736591421519));
#47795=CARTESIAN_POINT('Ctrl Pts',(-3.829771427655,0.969081152984,-3.782633088185));
#47796=CARTESIAN_POINT('Ctrl Pts',(-3.183801034714,2.33873436724,-3.828674754852));
#47797=CARTESIAN_POINT('Ctrl Pts',(-2.069994199668,3.364727549519,-3.874716421519));
#47798=CARTESIAN_POINT('Ctrl Pts',(-0.6520167487486,3.896298452185,-3.920758088185));
#47799=CARTESIAN_POINT('Ctrl Pts',(0.861769828621,3.855336591224,-3.966799754852));
#47800=CARTESIAN_POINT('Ctrl Pts',(2.248925587626,3.247861014648,-4.012841421519));
#47801=CARTESIAN_POINT('Ctrl Pts',(3.305618062651,2.163135847104,-4.058883088185));
#47802=CARTESIAN_POINT('Ctrl Pts',(3.87657396792,0.760553574966,-4.104924754852));
#47803=CARTESIAN_POINT('Ctrl Pts',(3.87789547929,-0.7537865220682,-4.150966421519));
#47804=CARTESIAN_POINT('Ctrl Pts',(3.309388410261,-2.157363163489,-4.197008088185));
#47805=CARTESIAN_POINT('Ctrl Pts',(2.254590746275,-3.243930954253,-4.243049754852));
#47806=CARTESIAN_POINT('Ctrl Pts',(0.8684973443836,-3.853826647885,-4.289091421519));
#47807=CARTESIAN_POINT('Ctrl Pts',(-0.64521543546,-3.897430501112,-4.335133088185));
#47808=CARTESIAN_POINT('Ctrl Pts',(-2.064118492452,-3.368335244341,-4.381174754852));
#47809=CARTESIAN_POINT('Ctrl Pts',(-3.179714326077,-2.344287583402,-4.427216421519));
#47810=CARTESIAN_POINT('Ctrl Pts',(-3.828074229756,-0.9757638856968,-4.473258088185));
#47811=CARTESIAN_POINT('Ctrl Pts',(-3.913926423865,0.5361412292629,-4.519299754852));
#47812=CARTESIAN_POINT('Ctrl Pts',(-3.424655551922,1.969264283907,-4.565341421519));
#47813=CARTESIAN_POINT('Ctrl Pts',(-2.432156415579,3.113018252307,-4.611383088185));
#47814=CARTESIAN_POINT('Ctrl Pts',(-1.082269555721,3.799336794534,-4.657424754852));
#47815=CARTESIAN_POINT('Ctrl Pts',(0.4266489564036,3.927370384378,-4.703466421519));
#47816=CARTESIAN_POINT('Ctrl Pts',(1.872874501785,3.478305416675,-4.749508088185));
#47817=CARTESIAN_POINT('Ctrl Pts',(3.043894742506,2.51812872327,-4.795549754852));
#47818=CARTESIAN_POINT('Ctrl Pts',(3.767636743447,1.187931312243,-4.841591421519));
#47819=CARTESIAN_POINT('Ctrl Pts',(3.937751926915,-0.3168240244129,-4.887633088185));
#47820=CARTESIAN_POINT('Ctrl Pts',(3.529242901566,-1.775024200642,-4.933674754852));
#47821=CARTESIAN_POINT('Ctrl Pts',(2.602137850332,-2.972398097546,-4.979716421519));
#47822=CARTESIAN_POINT('Ctrl Pts',(1.29266533598,-3.73299730079,-5.025758088185));
#47823=CARTESIAN_POINT('Ctrl Pts',(-0.2067467442558,-3.945068533638,-5.071799754852));
#47824=CARTESIAN_POINT('Ctrl Pts',(-1.67580956263,-3.577407472023,-5.117841421519));
#47825=CARTESIAN_POINT('Ctrl Pts',(-2.490943100776,-2.981933138547,-5.148535865963));
#47826=CARTESIAN_POINT('Ctrl Pts',(-2.827595238666,-2.618381900244,-5.163883088185));
#47827=CARTESIAN_POINT('Ctrl Pts',(-3.841349734859,-1.189096377216,-2.31389705505));
#47828=CARTESIAN_POINT('Ctrl Pts',(-3.994234933732,-0.6952040995074,-2.329244277272));
#47829=CARTESIAN_POINT('Ctrl Pts',(-4.10706259235,0.3520715397013,-2.359938721716));
#47830=CARTESIAN_POINT('Ctrl Pts',(-3.672853039324,1.871418570915,-2.405980388383));
#47831=CARTESIAN_POINT('Ctrl Pts',(-2.698930474802,3.115729236588,-2.45202205505));
#47832=CARTESIAN_POINT('Ctrl Pts',(-1.328423408128,3.902218173295,-2.498063721716));
#47833=CARTESIAN_POINT('Ctrl Pts',(0.2372868317335,4.115301255755,-2.544105388383));
#47834=CARTESIAN_POINT('Ctrl Pts',(1.76812922683,3.723671568578,-2.59014705505));
#47835=CARTESIAN_POINT('Ctrl Pts',(3.039157943544,2.784875152802,-2.636188721716));
#47836=CARTESIAN_POINT('Ctrl Pts',(3.863604450802,1.43686161852,-2.682230388383));
#47837=CARTESIAN_POINT('Ctrl Pts',(4.120322345675,-0.1222883131347,-2.72827205505));
#47838=CARTESIAN_POINT('Ctrl Pts',(3.771588791194,-1.663468860739,-2.774313721716));
#47839=CARTESIAN_POINT('Ctrl Pts',(2.868647652528,-2.960214740138,-2.820355388383));
#47840=CARTESIAN_POINT('Ctrl Pts',(1.544179572608,-3.821978559474,-2.86639705505));
#47841=CARTESIAN_POINT('Ctrl Pts',(-0.007194482043365,-4.122130383809,-2.912438721716));
#47842=CARTESIAN_POINT('Ctrl Pts',(-1.557511359811,-3.816565082075,-2.958480388383));
#47843=CARTESIAN_POINT('Ctrl Pts',(-2.8789632535,-2.950183256454,-3.00452205505));
#47844=CARTESIAN_POINT('Ctrl Pts',(-3.777372403381,-1.65029342477,-3.050563721716));
#47845=CARTESIAN_POINT('Ctrl Pts',(-4.120724108895,-0.1079049583238,-3.096605388383));
#47846=CARTESIAN_POINT('Ctrl Pts',(-3.85856533025,1.45033935817,-3.14264705505));
#47847=CARTESIAN_POINT('Ctrl Pts',(-3.029418396237,2.795466837973,-3.188688721716));
#47848=CARTESIAN_POINT('Ctrl Pts',(-1.755120427756,3.7298207659,-3.234730388383));
#47849=CARTESIAN_POINT('Ctrl Pts',(-0.2229202576515,4.11610461728,-3.28077205505));
#47850=CARTESIAN_POINT('Ctrl Pts',(1.342036425525,3.897556785247,-3.326813721716));
#47851=CARTESIAN_POINT('Ctrl Pts',(2.709790601495,3.106291286681,-3.372855388383));
#47852=CARTESIAN_POINT('Ctrl Pts',(3.679360726381,1.858578840628,-3.41889705505));
#47853=CARTESIAN_POINT('Ctrl Pts',(4.108275511099,0.337761730468,-3.464938721716));
#47854=CARTESIAN_POINT('Ctrl Pts',(3.933509042705,-1.232687013245,-3.510980388383));
#47855=CARTESIAN_POINT('Ctrl Pts',(3.180741984619,-2.622001351819,-3.55702205505));
#47856=CARTESIAN_POINT('Ctrl Pts',(1.960587989627,-3.626031632045,-3.603063721716));
#47857=CARTESIAN_POINT('Ctrl Pts',(0.4523398268471,-4.097242895254,-3.649105388383));
#47858=CARTESIAN_POINT('Ctrl Pts',(-1.122376388713,-3.966394068133,-3.69514705505));
#47859=CARTESIAN_POINT('Ctrl Pts',(-2.532167544361,-3.252712435637,-3.741188721716));
#47860=CARTESIAN_POINT('Ctrl Pts',(-3.569875067316,-2.061068331088,-3.787230388383));
#47861=CARTESIAN_POINT('Ctrl Pts',(-4.083015372648,-0.566565202236,-3.83327205505));
#47862=CARTESIAN_POINT('Ctrl Pts',(-3.99618621878,1.011190568834,-3.879313721716));
#47863=CARTESIAN_POINT('Ctrl Pts',(-3.322146519342,2.44035922882,-3.925355388383));
#47864=CARTESIAN_POINT('Ctrl Pts',(-2.159941513463,3.510934821395,-3.97139705505));
#47865=CARTESIAN_POINT('Ctrl Pts',(-0.6803487871228,4.065604037474,-4.017438721716));
#47866=CARTESIAN_POINT('Ctrl Pts',(0.8992162529668,4.022862263621,-4.063480388383));
#47867=CARTESIAN_POINT('Ctrl Pts',(2.346647994561,3.388990093123,-4.10952205505));
#47868=CARTESIAN_POINT('Ctrl Pts',(3.44925685411,2.257130438418,-4.155563721716));
#47869=CARTESIAN_POINT('Ctrl Pts',(4.045022466568,0.7936018564908,-4.201605388383));
#47870=CARTESIAN_POINT('Ctrl Pts',(4.046401401479,-0.7865407553148,-4.24764705505));
#47871=CARTESIAN_POINT('Ctrl Pts',(3.453191034373,-2.251106914784,-4.293688721716));
#47872=CARTESIAN_POINT('Ctrl Pts',(2.352559320954,-3.384889260088,-4.339730388383));
#47873=CARTESIAN_POINT('Ctrl Pts',(0.9062360990033,-4.021286708819,-4.38577205505));
#47874=CARTESIAN_POINT('Ctrl Pts',(-0.6732519368415,-4.066785277243,-4.431813721716));
#47875=CARTESIAN_POINT('Ctrl Pts',(-2.15381048955,-3.514699281129,-4.477855388383));
#47876=CARTESIAN_POINT('Ctrl Pts',(-3.31788223124,-2.446153748497,-4.52389705505));
#47877=CARTESIAN_POINT('Ctrl Pts',(-3.994415272659,-1.018163685866,-4.569938721716));
#47878=CARTESIAN_POINT('Ctrl Pts',(-4.083997996179,0.559438136759,-4.615980388383));
#47879=CARTESIAN_POINT('Ctrl Pts',(-3.573466871112,2.054834587688,-4.66202205505));
#47880=CARTESIAN_POINT('Ctrl Pts',(-2.537840738919,3.248288017621,-4.708063721716));
#47881=CARTESIAN_POINT('Ctrl Pts',(-1.129297339352,3.964429111665,-4.754105388383));
#47882=CARTESIAN_POINT('Ctrl Pts',(0.4451881037926,4.098026136172,-4.80014705505));
#47883=CARTESIAN_POINT('Ctrl Pts',(1.954256387077,3.629447979702,-4.846188721716));
#47884=CARTESIAN_POINT('Ctrl Pts',(3.176160888763,2.627548795309,-4.892230388383));
#47885=CARTESIAN_POINT('Ctrl Pts',(3.931351600467,1.239550408822,-4.93827205505));
#47886=CARTESIAN_POINT('Ctrl Pts',(4.108858787154,-0.3305909566808,-4.984313721716));
#47887=CARTESIAN_POINT('Ctrl Pts',(3.682598847576,-1.852154203613,-5.030355388383));
#47888=CARTESIAN_POINT('Ctrl Pts',(2.715208365118,-3.101557505068,-5.07639705505));
#47889=CARTESIAN_POINT('Ctrl Pts',(1.348835432798,-3.89520697252,-5.122438721716));
#47890=CARTESIAN_POINT('Ctrl Pts',(-0.2157304961352,-4.116493321879,-5.168480388383));
#47891=CARTESIAN_POINT('Ctrl Pts',(-1.748628398844,-3.732856309759,-5.21452205505));
#47892=CARTESIAN_POINT('Ctrl Pts',(-2.599181877855,-3.111506871542,-5.245216499494));
#47893=CARTESIAN_POINT('Ctrl Pts',(-2.950462537646,-2.7321582666,-5.260563721716));
#47894=CARTESIAN_POINT('',(-3.93909072274296,0.694567964780147,-2.35825152239436));
#47895=CARTESIAN_POINT('Ctrl Pts',(-1.36801982010901,-3.75859882970906,
-4.44169936887435));
#47896=CARTESIAN_POINT('Ctrl Pts',(-1.16576578312669,-3.83216333246039,
-4.43524390841633));
#47897=CARTESIAN_POINT('Ctrl Pts',(-0.957575527497493,-3.88947208452673,
-4.42876047910253));
#47898=CARTESIAN_POINT('Ctrl Pts',(-0.536796172629159,-3.96949863700133,
-4.41599000469032));
#47899=CARTESIAN_POINT('Ctrl Pts',(-0.324896257588679,-3.99243262327782,
-4.40974678199487));
#47900=CARTESIAN_POINT('Ctrl Pts',(0.308796827379884,-4.00997416051721,
-4.39084393819084));
#47901=CARTESIAN_POINT('Ctrl Pts',(0.731667503869158,-3.95512345077563,
-4.37811939203431));
#47902=CARTESIAN_POINT('Ctrl Pts',(1.5146514617827,-3.72296528639292,-4.35394723701022));
#47903=CARTESIAN_POINT('Ctrl Pts',(1.87461764815377,-3.55500354569365,-4.34205069592721));
#47904=CARTESIAN_POINT('Ctrl Pts',(2.41773986304984,-3.19701093090743,-4.32265348722271));
#47905=CARTESIAN_POINT('Ctrl Pts',(2.61842108636455,-3.03478219072031,-4.31510650260857));
#47906=CARTESIAN_POINT('Ctrl Pts',(2.99084947506056,-2.66884817888097,-4.29948206288811));
#47907=CARTESIAN_POINT('Ctrl Pts',(3.16094151410186,-2.46511362780033,-4.29150861837212));
#47908=CARTESIAN_POINT('Ctrl Pts',(3.45486522391036,-2.03243284581852,-4.27592206267503));
#47909=CARTESIAN_POINT('Ctrl Pts',(3.57889457870004,-1.80498630056301,-4.26834080484933));
#47910=CARTESIAN_POINT('Ctrl Pts',(3.78358421801442,-1.32374735077988,-4.25268267517954));
#47911=CARTESIAN_POINT('Ctrl Pts',(3.86291241695182,-1.07063456334499,-4.24471507975128));
#47912=CARTESIAN_POINT('Ctrl Pts',(3.9562346792498,-0.621236099015068,-4.23104966239667));
#47913=CARTESIAN_POINT('Ctrl Pts',(3.98179879462672,-0.42778244620501,-4.22532655594778));
#47914=CARTESIAN_POINT('Ctrl Pts',(4.0006808351246,-0.102475082871344,-4.21561255270373));
#47915=CARTESIAN_POINT('Ctrl Pts',(4.00184602497239,0.0283802363947507,
-4.2116916302295));
#47916=CARTESIAN_POINT('Ctrl Pts',(3.98631881005115,0.417925330358341,-4.19998549294754));
#47917=CARTESIAN_POINT('Ctrl Pts',(3.95094450054871,0.676006772840593,-4.19220583507454));
#47918=CARTESIAN_POINT('Ctrl Pts',(3.83009212472557,1.18237705257788,-4.17679517875193));
#47919=CARTESIAN_POINT('Ctrl Pts',(3.74482524678116,1.42917791521534,-4.16905051371582));
#47920=CARTESIAN_POINT('Ctrl Pts',(3.41725214324585,2.14415260468746,-4.14543441353372));
#47921=CARTESIAN_POINT('Ctrl Pts',(3.10715307845772,2.57323464944538,-4.13013006234986));
#47922=CARTESIAN_POINT('Ctrl Pts',(2.33529076991263,3.28964516038514,-4.09850418891609));
#47923=CARTESIAN_POINT('Ctrl Pts',(1.88427861435023,3.56721619917969,-4.08319599107816));
#47924=CARTESIAN_POINT('Ctrl Pts',(0.897021813530376,3.93331136940216,-4.05157410615685));
#47925=CARTESIAN_POINT('Ctrl Pts',(0.374300849531254,4.01683103674258,-4.03627217052875));
#47926=CARTESIAN_POINT('Ctrl Pts',(-0.406700731577845,3.98726923128037,
-4.0128015836215));
#47927=CARTESIAN_POINT('Ctrl Pts',(-0.66077444767884,3.95328764135642,-4.00518628092756));
#47928=CARTESIAN_POINT('Ctrl Pts',(-1.29629263820266,3.80479144684892,-3.98587135179335));
#47929=CARTESIAN_POINT('Ctrl Pts',(-1.66787074979849,3.65684562290541,-3.97389855805407));
#47930=CARTESIAN_POINT('Ctrl Pts',(-2.23256055970333,3.32895355733969,-3.95442486435378));
#47931=CARTESIAN_POINT('Ctrl Pts',(-2.44198852664714,3.17846702206362,-3.946883162998));
#47932=CARTESIAN_POINT('Ctrl Pts',(-2.83449224071045,2.83436117767312,-3.93126411001548));
#47933=CARTESIAN_POINT('Ctrl Pts',(-3.0158923819255,2.6405924163579,-3.92328975695283));
#47934=CARTESIAN_POINT('Ctrl Pts',(-3.25419004520932,2.32939589011373,-3.9116087917026));
#47935=CARTESIAN_POINT('Ctrl Pts',(-3.32684711275221,2.22440626126068,-3.90784050717486));
#47936=CARTESIAN_POINT('Ctrl Pts',(-3.53098322623027,1.8968969600739,-3.8964136633248));
#47937=CARTESIAN_POINT('Ctrl Pts',(-3.64591334087103,1.66489092518052,-3.88867432414806));
#47938=CARTESIAN_POINT('Ctrl Pts',(-3.82773226754075,1.18788211445012,-3.87334723842088));
#47939=CARTESIAN_POINT('Ctrl Pts',(-3.89534807804564,0.943441021874519,
-3.86583135445027));
#47940=CARTESIAN_POINT('Ctrl Pts',(-3.98410455565061,0.439436441188183,
-3.85068053490909));
#47941=CARTESIAN_POINT('Ctrl Pts',(-4.00398113926887,0.181108493150542,
-3.84293962576666));
#47942=CARTESIAN_POINT('Ctrl Pts',(-3.99423618289338,-0.330039477952322,
-3.82758902240187));
#47943=CARTESIAN_POINT('Ctrl Pts',(-3.96543189641876,-0.58262904558535,
-3.82005114587486));
#47944=CARTESIAN_POINT('Ctrl Pts',(-3.85892978523262,-1.08395434249013,
-3.80487945555321));
#47945=CARTESIAN_POINT('Ctrl Pts',(-3.78060972657924,-1.33107125885623,
-3.79713742203396));
#47946=CARTESIAN_POINT('Ctrl Pts',(-3.57995899763623,-1.80192518325927,
-3.78176871778775));
#47947=CARTESIAN_POINT('Ctrl Pts',(-3.45842129682671,-2.0257467495555,-3.77421392571749));
#47948=CARTESIAN_POINT('Ctrl Pts',(-3.17149943533642,-2.45111546943147,
-3.75902611469025));
#47949=CARTESIAN_POINT('Ctrl Pts',(-3.00620636341425,-2.65095450340893,
-3.75128326582865));
#47950=CARTESIAN_POINT('Ctrl Pts',(-2.6433796264621,-3.01259572402451,-3.73590056199311));
#47951=CARTESIAN_POINT('Ctrl Pts',(-2.44651657896266,-3.17475265057089,
-3.72833268979306));
#47952=CARTESIAN_POINT('Ctrl Pts',(-1.91004887642632,-3.53622917907652,
-3.70918533237558));
#47953=CARTESIAN_POINT('Ctrl Pts',(-1.5531977730994,-3.70654199789545,-3.69733967918743));
#47954=CARTESIAN_POINT('Ctrl Pts',(-0.93327777387392,-3.8981283944329,-3.6779928280832));
#47955=CARTESIAN_POINT('Ctrl Pts',(-0.680381380773941,-3.95008448602936,
-3.67044165819892));
#47956=CARTESIAN_POINT('Ctrl Pts',(-0.161076721039697,-4.0052428935594,
-3.65481304613054));
#47957=CARTESIAN_POINT('Ctrl Pts',(0.104301390506375,-4.00717576675699,
-3.64684029502901));
#47958=CARTESIAN_POINT('Ctrl Pts',(0.625265129427227,-3.95929015152296,
-3.63125258223983));
#47959=CARTESIAN_POINT('Ctrl Pts',(0.87982060422287,-3.91055295484658,-3.62366736051567));
#47960=CARTESIAN_POINT('Ctrl Pts',(1.38158822702633,-3.76284716596401,-3.60800540595417));
#47961=CARTESIAN_POINT('Ctrl Pts',(1.62743767511326,-3.66330469915853,-3.60003846977951));
#47962=CARTESIAN_POINT('Ctrl Pts',(2.02885592414387,-3.45243856135319,-3.58653982988137));
#47963=CARTESIAN_POINT('Ctrl Pts',(2.19000915014392,-3.35252857713794,-3.58097703367505));
#47964=CARTESIAN_POINT('Ctrl Pts',(2.44953544757942,-3.16477022048459,-3.5714321033113));
#47965=CARTESIAN_POINT('Ctrl Pts',(2.55168647331349,-3.08293791440222,-3.56751139854109));
#47966=CARTESIAN_POINT('Ctrl Pts',(2.8438699920888,-2.82451366131099,-3.55579962007338));
#47967=CARTESIAN_POINT('Ctrl Pts',(3.02162263004526,-2.63378253177322,-3.54800841374717));
#47968=CARTESIAN_POINT('Ctrl Pts',(3.33774443191726,-2.21972629663611,-3.53258525939748));
#47969=CARTESIAN_POINT('Ctrl Pts',(3.47511454605587,-1.99749597997082,-3.52484244301243));
#47970=CARTESIAN_POINT('Ctrl Pts',(3.70417329294106,-1.53116578729521,-3.50924166680827));
#47971=CARTESIAN_POINT('Ctrl Pts',(3.79596336309501,-1.28747036077039,-3.5014660396352));
#47972=CARTESIAN_POINT('Ctrl Pts',(3.93086443146694,-0.784789241119805,
-3.48605966099206));
#47973=CARTESIAN_POINT('Ctrl Pts',(3.97344498876691,-0.527215712248708,
-3.47831454476549));
#47974=CARTESIAN_POINT('Ctrl Pts',(4.02601313000844,0.257441192337123,-3.45469896792346));
#47975=CARTESIAN_POINT('Ctrl Pts',(3.95773352554131,0.782460838811398,-3.43939392117451));
#47976=CARTESIAN_POINT('Ctrl Pts',(3.70638867520848,1.52560960247683,-3.41583418645671));
#47977=CARTESIAN_POINT('Ctrl Pts',(3.60030600780396,1.76184934909529,-3.4081188962284));
#47978=CARTESIAN_POINT('Ctrl Pts',(3.21249126105984,2.43978950749078,-3.38500568355129));
#47979=CARTESIAN_POINT('Ctrl Pts',(2.8656607839029,2.83911477915266,-3.36926436353717));
#47980=CARTESIAN_POINT('Ctrl Pts',(2.0402068906059,3.47995424644701,-3.33833955282941));
#47981=CARTESIAN_POINT('Ctrl Pts',(1.56730987495655,3.71703270463164,-3.32259648616218));
#47982=CARTESIAN_POINT('Ctrl Pts',(0.813701158858086,3.92485852491073,-3.29946126283233));
#47983=CARTESIAN_POINT('Ctrl Pts',(0.557869758702243,3.96911471734924,-3.2917213834433));
#47984=CARTESIAN_POINT('Ctrl Pts',(0.040895471393891,4.0080431421574,-3.27615229447875));
#47985=CARTESIAN_POINT('Ctrl Pts',(-0.220021179035145,4.00238598974046,
-3.26840176631272));
#47986=CARTESIAN_POINT('Ctrl Pts',(-0.736359771982586,3.94012535110111,
-3.25300910270255));
#47987=CARTESIAN_POINT('Ctrl Pts',(-0.990294423548421,3.88388772859838,
-3.24524995137463));
#47988=CARTESIAN_POINT('Ctrl Pts',(-1.48398117232706,3.72344751635879,-3.22966151377038));
#47989=CARTESIAN_POINT('Ctrl Pts',(-1.72338094316868,3.61905993450343,-3.22191257145241));
#47990=CARTESIAN_POINT('Ctrl Pts',(-2.17787908259835,3.36508644455266,-3.20650121339441));
#47991=CARTESIAN_POINT('Ctrl Pts',(-2.39173715943083,3.21636544996632,-3.19872394421881));
#47992=CARTESIAN_POINT('Ctrl Pts',(-2.78788754242832,2.87995408720518,-3.18311797697578));
#47993=CARTESIAN_POINT('Ctrl Pts',(-2.96976345003142,2.69226206636054,-3.17537166592776));
#47994=CARTESIAN_POINT('Ctrl Pts',(-3.2938413076201,2.2842181674067,-3.15994447507618));
#47995=CARTESIAN_POINT('Ctrl Pts',(-3.43523185049853,2.06511106675781,-3.15215229730507));
#47996=CARTESIAN_POINT('Ctrl Pts',(-3.61420770737158,1.71846211251952,-3.14043876845689));
#47997=CARTESIAN_POINT('Ctrl Pts',(-3.66851681395888,1.59936773833699,-3.1365177963949));
#47998=CARTESIAN_POINT('Ctrl Pts',(-3.78741883704035,1.30058477932089,-3.12693529515567));
#47999=CARTESIAN_POINT('Ctrl Pts',(-3.84508629152518,1.11864882035746,-3.12133642896898));
#48000=CARTESIAN_POINT('Ctrl Pts',(-3.95104286114496,0.676470454311608,
-3.10779894402269));
#48001=CARTESIAN_POINT('Ctrl Pts',(-3.98706500780911,0.413676356601029,
-3.09983141354669));
#48002=CARTESIAN_POINT('Ctrl Pts',(-4.00681406888649,-0.108778943815362,
-3.08417712951966));
#48003=CARTESIAN_POINT('Ctrl Pts',(-3.99148210100408,-0.36725844207694,
-3.07659954287649));
#48004=CARTESIAN_POINT('Ctrl Pts',(-3.9098912479272,-0.883792825718099,
-3.0610174220215));
#48005=CARTESIAN_POINT('Ctrl Pts',(-3.84278805097487,-1.14057416481873,
-3.05304400200963));
#48006=CARTESIAN_POINT('Ctrl Pts',(-3.66176050597667,-1.63017617463855,
-3.037422922239));
#48007=CARTESIAN_POINT('Ctrl Pts',(-3.54936799047195,-1.86232897513618,
-3.02987925632651));
#48008=CARTESIAN_POINT('Ctrl Pts',(-3.2117528499792,-2.41560879945962,-3.01055241293434));
#48009=CARTESIAN_POINT('Ctrl Pts',(-2.95935888672256,-2.71938297014093,
-2.9987207473539));
#48010=CARTESIAN_POINT('Ctrl Pts',(-2.47742066852805,-3.15072353736212,
-2.97957666314663));
#48011=CARTESIAN_POINT('Ctrl Pts',(-2.27163322531345,-3.3019753608914,-2.97199852589408));
#48012=CARTESIAN_POINT('Ctrl Pts',(-1.83154094554953,-3.56516244550671,
-2.95660050003261));
#48013=CARTESIAN_POINT('Ctrl Pts',(-1.59707594248354,-3.67638616105042,
-2.94885314655851));
#48014=CARTESIAN_POINT('Ctrl Pts',(-1.11367518200821,-3.85023145239489,
-2.93364721253502));
#48015=CARTESIAN_POINT('Ctrl Pts',(-0.866403969682855,-3.91313184871958,
-2.92607812745012));
#48016=CARTESIAN_POINT('Ctrl Pts',(-0.360022481771758,-3.99189874134353,
-2.91068981694937));
#48017=CARTESIAN_POINT('Ctrl Pts',(-0.101032384666768,-4.00701925018241,
-2.90294304494526));
#48018=CARTESIAN_POINT('Ctrl Pts',(0.411881876223697,-3.9868228340172,-2.88774824810053));
#48019=CARTESIAN_POINT('Ctrl Pts',(0.664378073671907,-3.95243301126028,
-2.88019081295765));
#48020=CARTESIAN_POINT('Ctrl Pts',(1.1629544280647,-3.83566694225597,-2.86481501077947));
#48021=CARTESIAN_POINT('Ctrl Pts',(1.40862781016742,-3.75261330799575,-2.85706902662035));
#48022=CARTESIAN_POINT('Ctrl Pts',(1.87609365122038,-3.54181851853787,-2.84188859914504));
#48023=CARTESIAN_POINT('Ctrl Pts',(2.09694446312091,-3.41552013962223,-2.83434623395034));
#48024=CARTESIAN_POINT('Ctrl Pts',(2.51504445396781,-3.12078029921391,-2.81898661662597));
#48025=CARTESIAN_POINT('Ctrl Pts',(2.71162733856537,-2.95183390214576,-2.81124171364893));
#48026=CARTESIAN_POINT('Ctrl Pts',(3.06566136120269,-2.58179553922187,-2.79607991691089));
#48027=CARTESIAN_POINT('Ctrl Pts',(3.22284597780397,-2.38243455028453,-2.78855715517691));
#48028=CARTESIAN_POINT('Ctrl Pts',(3.49992739201803,-1.95323289660394,-2.77321859195396));
#48029=CARTESIAN_POINT('Ctrl Pts',(3.61895804909156,-1.72315656774654,-2.76547519260078));
#48030=CARTESIAN_POINT('Ctrl Pts',(3.76217493501356,-1.364537735472,-2.75404121352314));
#48031=CARTESIAN_POINT('Ctrl Pts',(3.80381657658998,-1.24372274051385,-2.75026968632714));
#48032=CARTESIAN_POINT('Ctrl Pts',(3.94531393268906,-0.758491646702463,
-2.7352066494307));
#48033=CARTESIAN_POINT('Ctrl Pts',(3.99971098138022,-0.380629373148319,
-2.72374973626902));
#48034=CARTESIAN_POINT('Ctrl Pts',(4.0000134136939,0.125170532368751,-2.70876711063907));
#48035=CARTESIAN_POINT('Ctrl Pts',(3.99401009623935,0.252250110774488,-2.70501503313205));
#48036=CARTESIAN_POINT('Ctrl Pts',(3.9568297462809,0.641754190918649,-2.69336498465536));
#48037=CARTESIAN_POINT('Ctrl Pts',(3.90565723780332,0.902033904090278,-2.6853970084711));
#48038=CARTESIAN_POINT('Ctrl Pts',(3.75487916969687,1.40258446379034,-2.66974521500997));
#48039=CARTESIAN_POINT('Ctrl Pts',(3.65656300521899,1.64204648993718,-2.66217022491873));
#48040=CARTESIAN_POINT('Ctrl Pts',(3.41187927734039,2.10414329315607,-2.64658894383737));
#48041=CARTESIAN_POINT('Ctrl Pts',(3.2651135487979,2.32528966893541,-2.6386150815753));
#48042=CARTESIAN_POINT('Ctrl Pts',(2.93511444117701,2.72965813373484,-2.62299657363307));
#48043=CARTESIAN_POINT('Ctrl Pts',(2.75356053688138,2.91275559104162,-2.61545546965109));
#48044=CARTESIAN_POINT('Ctrl Pts',(2.25387975142308,3.32738646981954,-2.59609326195907));
#48045=CARTESIAN_POINT('Ctrl Pts',(1.91544238363832,3.53340209283841,-2.5842260236807));
#48046=CARTESIAN_POINT('Ctrl Pts',(1.3179570910716,3.78521221421753,-2.56503529692822));
#48047=CARTESIAN_POINT('Ctrl Pts',(1.07381676479304,3.86140191952328,-2.55744394020935));
#48048=CARTESIAN_POINT('Ctrl Pts',(0.309698104580703,4.02229514523478,-2.53399511988193));
#48049=CARTESIAN_POINT('Ctrl Pts',(-0.219451971089868,4.02834519965438,
-2.5186969990541));
#48050=CARTESIAN_POINT('Ctrl Pts',(-1.25427613962423,3.83433141908602,-2.48707849671069));
#48051=CARTESIAN_POINT('Ctrl Pts',(-1.74569708460653,3.63704011328204,-2.47177159325893));
#48052=CARTESIAN_POINT('Ctrl Pts',(-2.62748994927562,3.06137544257374,-2.44014611995675));
#48053=CARTESIAN_POINT('Ctrl Pts',(-3.00575665316205,2.69084249663867,-2.42483886577149));
#48054=CARTESIAN_POINT('Ctrl Pts',(-3.38241896388994,2.13955135107824,-2.40478833402707));
#48055=CARTESIAN_POINT('Ctrl Pts',(-3.4560224092977,2.01859946390072,-2.4005448130044));
#48056=CARTESIAN_POINT('Ctrl Pts',(-3.62315488767914,1.70795073884791,-2.39002940232023));
#48057=CARTESIAN_POINT('Ctrl Pts',(-3.70821877218224,1.51441198273768,-2.38383620017788));
#48058=CARTESIAN_POINT('Ctrl Pts',(-3.84786718848642,1.11277137122209,-2.37115638012773));
#48059=CARTESIAN_POINT('Ctrl Pts',(-3.90187360705131,0.90513993314234,-2.36471469938033));
#48060=CARTESIAN_POINT('Ctrl Pts',(-3.93905195666665,0.694559625484905,
-2.35830063501608));
#48061=CARTESIAN_POINT('',(-3.4862157938408,0.614712896413036,-2.09242018782987));
#48062=CARTESIAN_POINT('',(-3.486219445663,0.6147145489409,-2.092752209506));
#48063=CARTESIAN_POINT('',(-1.21075130737245,-3.32651187758048,-4.92608554278596));
#48064=CARTESIAN_POINT('Ctrl Pts',(-3.48611163489721,0.614695485491625,
-2.092752209506));
#48065=CARTESIAN_POINT('Ctrl Pts',(-3.45247823923436,0.804904617636082,
-2.099265619468));
#48066=CARTESIAN_POINT('Ctrl Pts',(-3.40329486078118,0.992351978567723,
-2.1057790294295));
#48067=CARTESIAN_POINT('Ctrl Pts',(-3.33926661181778,1.17458628760328,-2.11229243939108));
#48068=CARTESIAN_POINT('Ctrl Pts',(-3.28724381166632,1.32265123070542,-2.11758456950899));
#48069=CARTESIAN_POINT('Ctrl Pts',(-3.22541325987337,1.46728788207019,-2.12287669962695));
#48070=CARTESIAN_POINT('Ctrl Pts',(-3.15416309562667,1.60712636907785,-2.12816882974492));
#48071=CARTESIAN_POINT('Ctrl Pts',(-3.13772049359028,1.63939729245812,-2.12939010958862));
#48072=CARTESIAN_POINT('Ctrl Pts',(-3.12077629297601,1.67141270174591,-2.13061138943231));
#48073=CARTESIAN_POINT('Ctrl Pts',(-3.10334122949876,1.70315880781664,-2.13183266927601));
#48074=CARTESIAN_POINT('Ctrl Pts',(-3.010355402605,1.87246922802227,-2.13834607923767));
#48075=CARTESIAN_POINT('Ctrl Pts',(-2.90342002496954,2.03409949917319,-2.14485948919933));
#48076=CARTESIAN_POINT('Ctrl Pts',(-2.78413804221371,2.18602098504228,-2.15137289916099));
#48077=CARTESIAN_POINT('Ctrl Pts',(-2.66485605945771,2.33794247091159,-2.15788630912266));
#48078=CARTESIAN_POINT('Ctrl Pts',(-2.53321256598554,2.48017394117643,-2.16439971908433));
#48079=CARTESIAN_POINT('Ctrl Pts',(-2.39079396961086,2.61067055624253,-2.170913129046));
#48080=CARTESIAN_POINT('Ctrl Pts',(-2.36676052640752,2.63269213956278,-2.17201228092896));
#48081=CARTESIAN_POINT('Ctrl Pts',(-2.34242073842935,2.65437904749335,-2.17311143281192));
#48082=CARTESIAN_POINT('Ctrl Pts',(-2.3177824805595,2.6757212808535,-2.17421058469488));
#48083=CARTESIAN_POINT('Ctrl Pts',(-2.19641810063612,2.78084993611871,-2.17962484277359));
#48084=CARTESIAN_POINT('Ctrl Pts',(-2.06781106235418,2.87761446755544,-2.18503910085229));
#48085=CARTESIAN_POINT('Ctrl Pts',(-1.93328280840194,2.96525962093555,-2.190453358931));
#48086=CARTESIAN_POINT('Ctrl Pts',(-1.7714438903673,3.07069767113915,-2.19696676889267));
#48087=CARTESIAN_POINT('Ctrl Pts',(-1.6010187810845,3.16295401534946,-2.20348017885433));
#48088=CARTESIAN_POINT('Ctrl Pts',(-1.42421971206299,3.24075297381787,-2.20999358881617));
#48089=CARTESIAN_POINT('Ctrl Pts',(-1.33140030198562,3.28159738249964,-2.21341312531936));
#48090=CARTESIAN_POINT('Ctrl Pts',(-1.23682153800335,3.31845691336659,-2.2168326618226));
#48091=CARTESIAN_POINT('Ctrl Pts',(-1.14082056111593,3.35113838080967,-2.22025219832584));
#48092=CARTESIAN_POINT('Ctrl Pts',(-1.05396233511999,3.38070739538729,-2.22334607178452));
#48093=CARTESIAN_POINT('Ctrl Pts',(-0.965939942205691,3.40685628944164,
-2.2264399452432));
#48094=CARTESIAN_POINT('Ctrl Pts',(-0.877038495435007,3.42954597194126,
-2.22953381870184));
#48095=CARTESIAN_POINT('Ctrl Pts',(-0.689877780312868,3.47731366703263,
-2.23604722866367));
#48096=CARTESIAN_POINT('Ctrl Pts',(-0.498817901017613,3.50975420229228,
-2.24256063862533));
#48097=CARTESIAN_POINT('Ctrl Pts',(-0.306392768733605,3.52652952279029,
-2.24907404858699));
#48098=CARTESIAN_POINT('Ctrl Pts',(-0.136818383836607,3.54131275105748,
-2.25481398221583));
#48099=CARTESIAN_POINT('Ctrl Pts',(0.0338347226870868,3.54392884861796,
-2.26055391584467));
#48100=CARTESIAN_POINT('Ctrl Pts',(0.203776655436933,3.53413003081367,-2.2662938494735));
#48101=CARTESIAN_POINT('Ctrl Pts',(0.226676931195759,3.53280960550016,-2.26706732580633));
#48102=CARTESIAN_POINT('Ctrl Pts',(0.249564290458189,3.53126376392604,-2.26784080213917));
#48103=CARTESIAN_POINT('Ctrl Pts',(0.27243444834103,3.52949358819305,-2.268614278472));
#48104=CARTESIAN_POINT('Ctrl Pts',(0.46502303554917,3.51458701670047,-2.27512768843367));
#48105=CARTESIAN_POINT('Ctrl Pts',(0.656363625397378,3.4837751352979,-2.28164109839533));
#48106=CARTESIAN_POINT('Ctrl Pts',(0.843944386843304,3.43771235132368,-2.288154508357));
#48107=CARTESIAN_POINT('Ctrl Pts',(1.03152514828923,3.39164956734945,-2.29466791831867));
#48108=CARTESIAN_POINT('Ctrl Pts',(1.21536958570617,3.33033103466894,-2.30118132828033));
#48109=CARTESIAN_POINT('Ctrl Pts',(1.39297675817359,3.25438475836223,-2.307694738242));
#48110=CARTESIAN_POINT('Ctrl Pts',(1.43515898045606,3.23634729588709,-2.3092416921347));
#48111=CARTESIAN_POINT('Ctrl Pts',(1.47698836004088,3.2174850491827,-2.3107886460274));
#48112=CARTESIAN_POINT('Ctrl Pts',(1.5184303722474,3.19780693673633,-2.3123355999201));
#48113=CARTESIAN_POINT('Ctrl Pts',(1.65147889683793,3.13463085796226,-2.31730205598907));
#48114=CARTESIAN_POINT('Ctrl Pts',(1.78053424961026,3.06304474292021,-2.32226851205804));
#48115=CARTESIAN_POINT('Ctrl Pts',(1.90464785652295,2.98375084516111,-2.32723496812701));
#48116=CARTESIAN_POINT('Ctrl Pts',(2.06742042360426,2.87975844970031,-2.33374837808867));
#48117=CARTESIAN_POINT('Ctrl Pts',(2.22171376607907,2.76250122118534,-2.34026178805033));
#48118=CARTESIAN_POINT('Ctrl Pts',(2.36547392639545,2.63349262599518,-2.34677519801199));
#48119=CARTESIAN_POINT('Ctrl Pts',(2.45083123681511,2.55689402814848,-2.35064252227459));
#48120=CARTESIAN_POINT('Ctrl Pts',(2.53247769695781,2.47614836598736,-2.35450984653719));
#48121=CARTESIAN_POINT('Ctrl Pts',(2.609961772308,2.3915893349595,-2.3583771707998));
#48122=CARTESIAN_POINT('Ctrl Pts',(2.66297762765571,2.3337326807108,-2.36102325649886));
#48123=CARTESIAN_POINT('Ctrl Pts',(2.71404492982089,2.27409090047738,-2.36366934219792));
#48124=CARTESIAN_POINT('Ctrl Pts',(2.7630696354151,2.21281727982083,-2.36631542789698));
#48125=CARTESIAN_POINT('Ctrl Pts',(2.88374524539246,2.06199064132035,-2.37282883785867));
#48126=CARTESIAN_POINT('Ctrl Pts',(2.99204550459216,1.90128017903614,-2.37934224782037));
#48127=CARTESIAN_POINT('Ctrl Pts',(3.08664143368824,1.73287520944786,-2.38585565778207));
#48128=CARTESIAN_POINT('Ctrl Pts',(3.17650752923906,1.57289055436952,-2.39204339469183));
#48129=CARTESIAN_POINT('Ctrl Pts',(3.2540133932933,1.40594134449907,-2.39823113160158));
#48130=CARTESIAN_POINT('Ctrl Pts',(3.317978242801,1.23394504751905,-2.40441886851134));
#48131=CARTESIAN_POINT('Ctrl Pts',(3.32134484161676,1.22489253611342,-2.40474454156322));
#48132=CARTESIAN_POINT('Ctrl Pts',(3.32467393213607,1.21582604517722,-2.40507021461511));
#48133=CARTESIAN_POINT('Ctrl Pts',(3.32796545991406,1.20674589826919,-2.405395887667));
#48134=CARTESIAN_POINT('Ctrl Pts',(3.39379549925573,1.02514438416957,-2.41190929762864));
#48135=CARTESIAN_POINT('Ctrl Pts',(3.4445898638602,0.838110253654046,-2.41842270759027));
#48136=CARTESIAN_POINT('Ctrl Pts',(3.47993533170847,0.648217911398604,-2.42493611755191));
#48137=CARTESIAN_POINT('Ctrl Pts',(3.51528079955726,0.458325569140407,-2.43144952751364));
#48138=CARTESIAN_POINT('Ctrl Pts',(3.53518366555639,0.265551810365206,-2.43796293747537));
#48139=CARTESIAN_POINT('Ctrl Pts',(3.53921587207989,0.0724312289064312,
-2.44447634743708));
#48140=CARTESIAN_POINT('Ctrl Pts',(3.5404507477039,0.0132874580830817,-2.44647109922969));
#48141=CARTESIAN_POINT('Ctrl Pts',(3.54019686595504,-0.0458877048812477,
-2.44846585102229));
#48142=CARTESIAN_POINT('Ctrl Pts',(3.53844190482233,-0.105018504061302,
-2.4504606028149));
#48143=CARTESIAN_POINT('Ctrl Pts',(3.53446643805599,-0.238965930375457,
-2.4549792609839));
#48144=CARTESIAN_POINT('Ctrl Pts',(3.52278756542149,-0.372685587266579,
-2.45949791915291));
#48145=CARTESIAN_POINT('Ctrl Pts',(3.50360264434659,-0.505307275679988,
-2.46401657732192));
#48146=CARTESIAN_POINT('Ctrl Pts',(3.47594858170895,-0.69647451917164,-2.47052998728364));
#48147=CARTESIAN_POINT('Ctrl Pts',(3.43270056047567,-0.885379751350099,
-2.47704339724537));
#48148=CARTESIAN_POINT('Ctrl Pts',(3.37442090167997,-1.06953540954889,-2.4835568072071));
#48149=CARTESIAN_POINT('Ctrl Pts',(3.33581079605796,-1.19153800120563,-2.48787192249395));
#48150=CARTESIAN_POINT('Ctrl Pts',(3.29059905133193,-1.31146265306598,-2.4921870377808));
#48151=CARTESIAN_POINT('Ctrl Pts',(3.23895722418867,-1.42855034908728,-2.49650215306765));
#48152=CARTESIAN_POINT('Ctrl Pts',(3.21264878372798,-1.48819956852543,-2.49870044774243));
#48153=CARTESIAN_POINT('Ctrl Pts',(3.18467168469657,-1.54711255044106,-2.50089874241722));
#48154=CARTESIAN_POINT('Ctrl Pts',(3.15508456246594,-1.60520476755959,-2.503097037092));
#48155=CARTESIAN_POINT('Ctrl Pts',(3.06741976534675,-1.77732838229316,-2.50961044705364));
#48156=CARTESIAN_POINT('Ctrl Pts',(2.96562690748144,-1.94223957070431,-2.51612385701527));
#48157=CARTESIAN_POINT('Ctrl Pts',(2.85118122343503,-2.0978372735158,-2.52263726697691));
#48158=CARTESIAN_POINT('Ctrl Pts',(2.73673553938697,-2.25343497632954,-2.52915067693864));
#48159=CARTESIAN_POINT('Ctrl Pts',(2.60962088951851,-2.39973705663602,-2.53566408690037));
#48160=CARTESIAN_POINT('Ctrl Pts',(2.47132239430563,-2.53459348728904,-2.54217749686209));
#48161=CARTESIAN_POINT('Ctrl Pts',(2.4687292831959,-2.53712205933177,-2.54229962397351));
#48162=CARTESIAN_POINT('Ctrl Pts',(2.46613224843455,-2.5396465996386,-2.54242175108493));
#48163=CARTESIAN_POINT('Ctrl Pts',(2.463531299937,-2.54216709408167,-2.54254387819635));
#48164=CARTESIAN_POINT('Ctrl Pts',(2.32741576151579,-2.67407222735452,-2.54893516104657));
#48165=CARTESIAN_POINT('Ctrl Pts',(2.18058121321383,-2.79489605595183,-2.55532644389679));
#48166=CARTESIAN_POINT('Ctrl Pts',(2.02510726029512,-2.90329545916035,-2.56171772674717));
#48167=CARTESIAN_POINT('Ctrl Pts',(1.8666624507869,-3.01376620020569,-2.56823113670897));
#48168=CARTESIAN_POINT('Ctrl Pts',(1.69922697758555,-3.11134926906942,-2.57474454667094));
#48169=CARTESIAN_POINT('Ctrl Pts',(1.52494467780377,-3.19463871795646,-2.58125795663274));
#48170=CARTESIAN_POINT('Ctrl Pts',(1.45958838442203,-3.22587246724644,-2.58370050147471));
#48171=CARTESIAN_POINT('Ctrl Pts',(1.39326974838671,-3.25509547106922,-2.58614304631666));
#48172=CARTESIAN_POINT('Ctrl Pts',(1.32610734069228,-3.28223084516667,-2.5885855911586));
#48173=CARTESIAN_POINT('Ctrl Pts',(1.21417117552754,-3.32745599151041,-2.59265645627845));
#48174=CARTESIAN_POINT('Ctrl Pts',(1.09989117051022,-3.3668818964363,-2.59672732139827));
#48175=CARTESIAN_POINT('Ctrl Pts',(0.983909678540035,-3.40038425065325,
-2.60079818651808));
#48176=CARTESIAN_POINT('Ctrl Pts',(0.7983385571865,-3.45398822948136,-2.6073115964797));
#48177=CARTESIAN_POINT('Ctrl Pts',(0.608398132847114,-3.49243632959352,
-2.6138250064413));
#48178=CARTESIAN_POINT('Ctrl Pts',(0.416593020999057,-3.51524584577225,
-2.62033841640292));
#48179=CARTESIAN_POINT('Ctrl Pts',(0.276336123570182,-3.53192523424243,
-2.62510132738114));
#48180=CARTESIAN_POINT('Ctrl Pts',(0.135071043364323,-3.54024113541699,
-2.62986423835936));
#48181=CARTESIAN_POINT('Ctrl Pts',(-0.00617846241521518,-3.539994608273,
-2.63462714933759));
#48182=CARTESIAN_POINT('Ctrl Pts',(-0.0580914873315994,-3.53990400286027,
-2.63637764832109));
#48183=CARTESIAN_POINT('Ctrl Pts',(-0.110002393163228,-3.53865692860149,
-2.63812814730459));
#48184=CARTESIAN_POINT('Ctrl Pts',(-0.161860370969655,-3.53626328586113,
-2.6398786462881));
#48185=CARTESIAN_POINT('Ctrl Pts',(-0.35481807755392,-3.52735681026954,
-2.64639205624973));
#48186=CARTESIAN_POINT('Ctrl Pts',(-0.547027243948119,-3.50257873337156,
-2.65290546621137));
#48187=CARTESIAN_POINT('Ctrl Pts',(-0.735963904152669,-3.46243784695285,
-2.659418876173));
#48188=CARTESIAN_POINT('Ctrl Pts',(-0.92490056435722,-3.42229696053415,
-2.66593228613464));
#48189=CARTESIAN_POINT('Ctrl Pts',(-1.11058788540349,-3.36678693880149,
-2.67244569609627));
#48190=CARTESIAN_POINT('Ctrl Pts',(-1.29047199844307,-3.29639980380972,
-2.67895910605791));
#48191=CARTESIAN_POINT('Ctrl Pts',(-1.30621201758925,-3.29024086718272,
-2.67952903519601));
#48192=CARTESIAN_POINT('Ctrl Pts',(-1.32190738964502,-3.28396810707535,
-2.68009896433411));
#48193=CARTESIAN_POINT('Ctrl Pts',(-1.33755638533705,-3.27758187022733,
-2.68066889347221));
#48194=CARTESIAN_POINT('Ctrl Pts',(-1.5007512451651,-3.21098328155419,-2.68661237429584));
#48195=CARTESIAN_POINT('Ctrl Pts',(-1.65890194128621,-3.13204291772606,
-2.69255585511947));
#48196=CARTESIAN_POINT('Ctrl Pts',(-1.81033770201859,-3.04186253180114,
-2.69849933594308));
#48197=CARTESIAN_POINT('Ctrl Pts',(-1.97629486109295,-2.94303461572669,
-2.7050127459047));
#48198=CARTESIAN_POINT('Ctrl Pts',(-2.13420984660948,-2.83069876261338,
-2.7115261558663));
#48199=CARTESIAN_POINT('Ctrl Pts',(-2.28193901730622,-2.70625136015001,
-2.71803956582792));
#48200=CARTESIAN_POINT('Ctrl Pts',(-2.34749402191622,-2.65102766936699,
-2.72092989966008));
#48201=CARTESIAN_POINT('Ctrl Pts',(-2.41104305301027,-2.593418363129,-2.72382023349223));
#48202=CARTESIAN_POINT('Ctrl Pts',(-2.47239011042567,-2.53355227731117,
-2.72671056732439));
#48203=CARTESIAN_POINT('Ctrl Pts',(-2.54928955258278,-2.45850925491567,
-2.73033364345396));
#48204=CARTESIAN_POINT('Ctrl Pts',(-2.62272889170948,-2.37992008874756,
-2.73395671958353));
#48205=CARTESIAN_POINT('Ctrl Pts',(-2.69244525650513,-2.29816470206638,
-2.7375797957131));
#48206=CARTESIAN_POINT('Ctrl Pts',(-2.81777832948228,-2.15118839492212,
-2.74409320567473));
#48207=CARTESIAN_POINT('Ctrl Pts',(-2.93108910381199,-1.9939736040557,-2.75060661563637));
#48208=CARTESIAN_POINT('Ctrl Pts',(-3.03092976256236,-1.82862245583661,
-2.757120025598));
#48209=CARTESIAN_POINT('Ctrl Pts',(-3.11080203430125,-1.69634196001263,
-2.76233073691455));
#48210=CARTESIAN_POINT('Ctrl Pts',(-3.18205838653695,-1.55884051299148,
-2.7675414482311));
#48211=CARTESIAN_POINT('Ctrl Pts',(-3.2439240626505,-1.41723557525111,-2.77275215954765));
#48212=CARTESIAN_POINT('Ctrl Pts',(-3.25939072882222,-1.38183377512727,
-2.77405485819274));
#48213=CARTESIAN_POINT('Ctrl Pts',(-3.27427051474745,-1.34617553341453,
-2.77535755683782));
#48214=CARTESIAN_POINT('Ctrl Pts',(-3.28855875162332,-1.31028157168752,
-2.77666025548291));
#48215=CARTESIAN_POINT('Ctrl Pts',(-3.35999902275125,-1.13081405726206,
-2.78317366544464));
#48216=CARTESIAN_POINT('Ctrl Pts',(-3.41664396289098,-0.9454748130943,-2.78968707540637));
#48217=CARTESIAN_POINT('Ctrl Pts',(-3.45794355355989,-0.756788175000208,
-2.79620048536809));
#48218=CARTESIAN_POINT('Ctrl Pts',(-3.4992431442282,-0.568101536908848,
-2.80271389532973));
#48219=CARTESIAN_POINT('Ctrl Pts',(-3.52520219045535,-0.376044002607322,
-2.80922730529137));
#48220=CARTESIAN_POINT('Ctrl Pts',(-3.53524656047543,-0.183140996775931,
-2.815740715253));
#48221=CARTESIAN_POINT('Ctrl Pts',(-3.5368160129307,-0.152999524933752,
-2.8167584482951));
#48222=CARTESIAN_POINT('Ctrl Pts',(-3.53799685819296,-0.122838037839213,
-2.8177761813372));
#48223=CARTESIAN_POINT('Ctrl Pts',(-3.53878693041333,-0.0926663970097928,
-2.8187939143793));
#48224=CARTESIAN_POINT('Ctrl Pts',(-3.54305325712833,0.0702580470943514,
-2.82428959129884));
#48225=CARTESIAN_POINT('Ctrl Pts',(-3.5359238682156,0.233478412978711,-2.82978526821837));
#48226=CARTESIAN_POINT('Ctrl Pts',(-3.51766563120604,0.39542686488809,-2.83528094513791));
#48227=CARTESIAN_POINT('Ctrl Pts',(-3.4960261890476,0.587366215653757,-2.84179435509964));
#48228=CARTESIAN_POINT('Ctrl Pts',(-3.4587560775586,0.777542371199,-2.84830776506136));
#48229=CARTESIAN_POINT('Ctrl Pts',(-3.40627360153106,0.963435501424819,
-2.85482117502308));
#48230=CARTESIAN_POINT('Ctrl Pts',(-3.3793763475951,1.05870567743577,-2.85815929576337));
#48231=CARTESIAN_POINT('Ctrl Pts',(-3.34848198131686,1.15285246353696,-2.86149741650365));
#48232=CARTESIAN_POINT('Ctrl Pts',(-3.313650756516,1.24551943535272,-2.86483553724394));
#48233=CARTESIAN_POINT('Ctrl Pts',(-3.28051857787996,1.33366616810228,-2.86801082646526));
#48234=CARTESIAN_POINT('Ctrl Pts',(-3.24382428725794,1.42047390410623,-2.87118611568659));
#48235=CARTESIAN_POINT('Ctrl Pts',(-3.20373088991644,1.50567764427224,-2.87436140490792));
#48236=CARTESIAN_POINT('Ctrl Pts',(-3.12148807187998,1.68045444452225,-2.88087481486964));
#48237=CARTESIAN_POINT('Ctrl Pts',(-3.02494376338762,1.84848829715205,-2.88738822483137));
#48238=CARTESIAN_POINT('Ctrl Pts',(-2.91544434228993,2.0076070020078,-2.89390163479326));
#48239=CARTESIAN_POINT('Ctrl Pts',(-2.82031689157503,2.14584112783464,-2.89956014950434));
#48240=CARTESIAN_POINT('Ctrl Pts',(-2.7153993256723,2.27735955487245,-2.90521866421555));
#48241=CARTESIAN_POINT('Ctrl Pts',(-2.601597666831,2.400685231333,-2.91087717892667));
#48242=CARTESIAN_POINT('Ctrl Pts',(-2.58440437448575,2.41931742378652,-2.91173207417739));
#48243=CARTESIAN_POINT('Ctrl Pts',(-2.5670083197053,2.43776262618973,-2.91258696942811));
#48244=CARTESIAN_POINT('Ctrl Pts',(-2.54941430867889,2.4560172922504,-2.91344186467883));
#48245=CARTESIAN_POINT('Ctrl Pts',(-2.41536629918196,2.59509880389615,-2.91995527464064));
#48246=CARTESIAN_POINT('Ctrl Pts',(-2.26984684389257,2.72310064051428,-2.92646868460227));
#48247=CARTESIAN_POINT('Ctrl Pts',(-2.11495442977927,2.83849845023986,-2.93298209456391));
#48248=CARTESIAN_POINT('Ctrl Pts',(-1.96006201566371,2.95389625996712,-2.93949550452564));
#48249=CARTESIAN_POINT('Ctrl Pts',(-1.79577783391285,3.05670494108783,-2.94600891448736));
#48250=CARTESIAN_POINT('Ctrl Pts',(-1.62417584367481,3.14538952674968,-2.95252232444909));
#48251=CARTESIAN_POINT('Ctrl Pts',(-1.5855649121518,3.16534380851171,-2.95398786005078));
#48252=CARTESIAN_POINT('Ctrl Pts',(-1.54658437024401,3.18458250627967,-2.95545339565246));
#48253=CARTESIAN_POINT('Ctrl Pts',(-1.50725869214041,3.20308776572967,-2.95691893125415));
#48254=CARTESIAN_POINT('Ctrl Pts',(-1.37180576833643,3.26682707345756,-2.9619668056141));
#48255=CARTESIAN_POINT('Ctrl Pts',(-1.23225792299338,3.32186406534164,-2.96701467997405));
#48256=CARTESIAN_POINT('Ctrl Pts',(-1.08981621794126,3.36789750679959,-2.972062554334));
#48257=CARTESIAN_POINT('Ctrl Pts',(-0.90601980097821,3.42729571182215,-2.97857596429564));
#48258=CARTESIAN_POINT('Ctrl Pts',(-0.717386036659192,3.47171455680863,
-2.98508937425727));
#48259=CARTESIAN_POINT('Ctrl Pts',(-0.526388358542247,3.50052703129853,
-2.99160278421891));
#48260=CARTESIAN_POINT('Ctrl Pts',(-0.415371292863036,3.51727423160149,
-2.99538869234426));
#48261=CARTESIAN_POINT('Ctrl Pts',(-0.303551189065533,3.52874803372401,
-2.99917460046961));
#48262=CARTESIAN_POINT('Ctrl Pts',(-0.191438997966164,3.5348198129545,-3.00296050859496));
#48263=CARTESIAN_POINT('Ctrl Pts',(-0.110669418520737,3.53919413701438,
-3.00568801043134));
#48264=CARTESIAN_POINT('Ctrl Pts',(-0.0297482761444177,3.54076478310675,
-3.00841551226771));
#48265=CARTESIAN_POINT('Ctrl Pts',(0.0511292772991568,3.53955874091815,
-3.01114301410408));
#48266=CARTESIAN_POINT('Ctrl Pts',(0.244268895115812,3.53667865222285,-3.0176564240657));
#48267=CARTESIAN_POINT('Ctrl Pts',(0.437158914978994,3.51796689039577,-3.0241698340273));
#48268=CARTESIAN_POINT('Ctrl Pts',(0.627264950562928,3.48378569015157,-3.03068324398892));
#48269=CARTESIAN_POINT('Ctrl Pts',(0.805489255928714,3.45174083344104,-3.03678956229916));
#48270=CARTESIAN_POINT('Ctrl Pts',(0.981286782970914,3.40609307546753,-3.0428958806094));
#48271=CARTESIAN_POINT('Ctrl Pts',(1.15251126677808,3.3471357576215,-3.04900219891965));
#48272=CARTESIAN_POINT('Ctrl Pts',(1.16392633791351,3.34320523342191,-3.04940929057113));
#48273=CARTESIAN_POINT('Ctrl Pts',(1.1753210843407,3.33921555889236,-3.04981638222261));
#48274=CARTESIAN_POINT('Ctrl Pts',(1.18669494970798,3.33516705334005,-3.05022347387409));
#48275=CARTESIAN_POINT('Ctrl Pts',(1.36867521807276,3.27039152601533,-3.05673688383573));
#48276=CARTESIAN_POINT('Ctrl Pts',(1.54528068641558,3.19056603871398,-3.06325029379737));
#48277=CARTESIAN_POINT('Ctrl Pts',(1.7142617758279,3.09700442209031,-3.069763703759));
#48278=CARTESIAN_POINT('Ctrl Pts',(1.88324286524021,3.00344280546664,-3.07627711372064));
#48279=CARTESIAN_POINT('Ctrl Pts',(2.04462139391706,2.89613498241052,-3.08279052368227));
#48280=CARTESIAN_POINT('Ctrl Pts',(2.19616581212668,2.77635948507303,-3.08930393364391));
#48281=CARTESIAN_POINT('Ctrl Pts',(2.24068245442155,2.74117506169632,-3.09121726799701));
#48282=CARTESIAN_POINT('Ctrl Pts',(2.28434948110076,2.70491536505777,-3.09313060235012));
#48283=CARTESIAN_POINT('Ctrl Pts',(2.32710837011083,2.667614408748,-3.09504393670323));
#48284=CARTESIAN_POINT('Ctrl Pts',(2.42991012144495,2.57793472520482,-3.09964401231185));
#48285=CARTESIAN_POINT('Ctrl Pts',(2.52746203568147,2.4822357996935,-3.10424408792047));
#48286=CARTESIAN_POINT('Ctrl Pts',(2.61918727517748,2.38126086742591,-3.10884416352909));
#48287=CARTESIAN_POINT('Ctrl Pts',(2.74906429014366,2.2382868848952,-3.11535757349073));
#48288=CARTESIAN_POINT('Ctrl Pts',(2.8672760376804,2.08472396627836,-3.12187098345237));
#48289=CARTESIAN_POINT('Ctrl Pts',(2.97225682514692,1.92258536488255,-3.128384393414));
#48290=CARTESIAN_POINT('Ctrl Pts',(3.04049404589932,1.81719572356882,-3.13261809182805));
#48291=CARTESIAN_POINT('Ctrl Pts',(3.10314345866287,1.7081759162302,-3.13685179024211));
#48292=CARTESIAN_POINT('Ctrl Pts',(3.15975379732033,1.59610649404043,-3.14108548865616));
#48293=CARTESIAN_POINT('Ctrl Pts',(3.19023665890577,1.53576068503122,-3.14336520020374));
#48294=CARTESIAN_POINT('Ctrl Pts',(3.21896862084255,1.4745307323558,-3.14564491175132));
#48295=CARTESIAN_POINT('Ctrl Pts',(3.24591833613534,1.41252706412558,-3.14792462329891));
#48296=CARTESIAN_POINT('Ctrl Pts',(3.32291691266137,1.23537512981941,-3.15443803326064));
#48297=CARTESIAN_POINT('Ctrl Pts',(3.38536604105095,1.05191544335807,-3.16095144322237));
#48298=CARTESIAN_POINT('Ctrl Pts',(3.43257863439251,0.864620338177983,-3.16746485318408));
#48299=CARTESIAN_POINT('Ctrl Pts',(3.47979122773339,0.677325233000615,-3.1739782631457));
#48300=CARTESIAN_POINT('Ctrl Pts',(3.51177061081401,0.486170850953884,-3.1804916731073));
#48301=CARTESIAN_POINT('Ctrl Pts',(3.52779770972739,0.293671846368205,-3.18700508306892));
#48302=CARTESIAN_POINT('Ctrl Pts',(3.543824808641,0.101172841779728,-3.19351849303064));
#48303=CARTESIAN_POINT('Ctrl Pts',(3.54389063706576,-0.0926387220615211,
-3.20003190299237));
#48304=CARTESIAN_POINT('Ctrl Pts',(3.52829370107048,-0.285162093399606,
-3.20654531295409));
#48305=CARTESIAN_POINT('Ctrl Pts',(3.51269676507543,-0.477685464734901,
-3.21305872291573));
#48306=CARTESIAN_POINT('Ctrl Pts',(3.48143795907197,-0.668944729192226,
-3.21957213287737));
#48307=CARTESIAN_POINT('Ctrl Pts',(3.43479147403392,-0.856389724647796,
-3.226085542839));
#48308=CARTESIAN_POINT('Ctrl Pts',(3.41788200033906,-0.924339029237458,
-3.22844667110665));
#48309=CARTESIAN_POINT('Ctrl Pts',(3.39895032352517,-0.991786185528747,
-3.23080779937431));
#48310=CARTESIAN_POINT('Ctrl Pts',(3.37801076294783,-1.05860440458689,-3.23316892764197));
#48311=CARTESIAN_POINT('Ctrl Pts',(3.34118643821444,-1.17611096770774,-3.23732120933597));
#48312=CARTESIAN_POINT('Ctrl Pts',(3.29815197932222,-1.29167222505157,-3.24147349102998));
#48313=CARTESIAN_POINT('Ctrl Pts',(3.24923804098248,-1.40467798595002,-3.24562577272407));
#48314=CARTESIAN_POINT('Ctrl Pts',(3.17250997753937,-1.58194265704298,-3.25213918268597));
#48315=CARTESIAN_POINT('Ctrl Pts',(3.08131256433664,-1.75293573710959,-3.25865259264803));
#48316=CARTESIAN_POINT('Ctrl Pts',(2.97686209402291,-1.91541538362651,-3.26516600260991));
#48317=CARTESIAN_POINT('Ctrl Pts',(2.90178864237807,-2.03219712572322,-3.26984749582241));
#48318=CARTESIAN_POINT('Ctrl Pts',(2.81986112148131,-2.14458818654423,-3.27452898903482));
#48319=CARTESIAN_POINT('Ctrl Pts',(2.73155102519233,-2.2517168997835,-3.27921048224721));
#48320=CARTESIAN_POINT('Ctrl Pts',(2.6969943704714,-2.29363747409692,-3.28104239899645));
#48321=CARTESIAN_POINT('Ctrl Pts',(2.66146049390567,-2.3347523204531,-3.28287431574568));
#48322=CARTESIAN_POINT('Ctrl Pts',(2.62499516111465,-2.37502361902704,-3.28470623249492));
#48323=CARTESIAN_POINT('Ctrl Pts',(2.4953420740096,-2.51820887971737,-3.29121964245664));
#48324=CARTESIAN_POINT('Ctrl Pts',(2.35392512391005,-2.65072077167277,-3.29773305241837));
#48325=CARTESIAN_POINT('Ctrl Pts',(2.20273828215037,-2.77093269463369,-3.3042464623801));
#48326=CARTESIAN_POINT('Ctrl Pts',(2.05155144039287,-2.89114461759288,-3.31075987234173));
#48327=CARTESIAN_POINT('Ctrl Pts',(1.89057497031891,-2.9990702680108,-3.31727328230337));
#48328=CARTESIAN_POINT('Ctrl Pts',(1.7218118521876,-3.09304726818777,-3.323786692265));
#48329=CARTESIAN_POINT('Ctrl Pts',(1.70915449898499,-3.10009560965795,-3.32427520261816));
#48330=CARTESIAN_POINT('Ctrl Pts',(1.69645349524291,-3.10706540362333,-3.32476371297131));
#48331=CARTESIAN_POINT('Ctrl Pts',(1.68370970010857,-3.11395594794783,-3.32525222332447));
#48332=CARTESIAN_POINT('Ctrl Pts',(1.52653782888907,-3.19893846169562,-3.33127712293295));
#48333=CARTESIAN_POINT('Ctrl Pts',(1.36285678345318,-3.2718654745696,-3.33730202254143));
#48334=CARTESIAN_POINT('Ctrl Pts',(1.19465624061227,-3.33212144593867,-3.34332692214991));
#48335=CARTESIAN_POINT('Ctrl Pts',(1.01281767690137,-3.39726308640959,-3.34984033211164));
#48336=CARTESIAN_POINT('Ctrl Pts',(0.825675827052175,-3.44760704052864,
-3.35635374207337));
#48337=CARTESIAN_POINT('Ctrl Pts',(0.635671099317594,-3.48238259226642,
-3.3628671520351));
#48338=CARTESIAN_POINT('Ctrl Pts',(0.553731273711291,-3.49737960143946,
-3.36567606991167));
#48339=CARTESIAN_POINT('Ctrl Pts',(0.471258885802527,-3.50948064073937,
-3.36848498778823));
#48340=CARTESIAN_POINT('Ctrl Pts',(0.38845946126229,-3.51862178231117,-3.37129390566481));
#48341=CARTESIAN_POINT('Ctrl Pts',(0.279260892156459,-3.53067741657646,
-3.37499839774987));
#48342=CARTESIAN_POINT('Ctrl Pts',(0.169493539234521,-3.53758465049955,
-3.37870288983494));
#48343=CARTESIAN_POINT('Ctrl Pts',(0.059649471939911,-3.53938415619341,
-3.38240738192));
#48344=CARTESIAN_POINT('Ctrl Pts',(-0.133483466588335,-3.54254813064478,
-3.38892079188164));
#48345=CARTESIAN_POINT('Ctrl Pts',(-0.326865118477281,-3.52992630187154,
-3.39543420184327));
#48346=CARTESIAN_POINT('Ctrl Pts',(-0.517952514192366,-3.50173373138306,
-3.40194761180491));
#48347=CARTESIAN_POINT('Ctrl Pts',(-0.668433322988736,-3.47953215815382,
-3.40707690458417));
#48348=CARTESIAN_POINT('Ctrl Pts',(-0.817504437674782,-3.44766956351041,
-3.41220619736343));
#48349=CARTESIAN_POINT('Ctrl Pts',(-0.963872074523706,-3.4062516970935,
-3.41733549014268));
#48350=CARTESIAN_POINT('Ctrl Pts',(-1.00336874001705,-3.39507526731343,
-3.41871960732515));
#48351=CARTESIAN_POINT('Ctrl Pts',(-1.04266855713235,-3.38320312817922,
-3.42010372450761));
#48352=CARTESIAN_POINT('Ctrl Pts',(-1.0817487466423,-3.37064673995017,-3.42148784169008));
#48353=CARTESIAN_POINT('Ctrl Pts',(-1.26565318687387,-3.31155860405448,
-3.4280012516517));
#48354=CARTESIAN_POINT('Ctrl Pts',(-1.4446743658271,-3.23732575217221,-3.4345146616133));
#48355=CARTESIAN_POINT('Ctrl Pts',(-1.61651402611654,-3.14912462305492,
-3.44102807157492));
#48356=CARTESIAN_POINT('Ctrl Pts',(-1.78835368640846,-3.06092349393635,
-3.44754148153664));
#48357=CARTESIAN_POINT('Ctrl Pts',(-1.95303292882817,-2.95874267186129,
-3.45405489149837));
#48358=CARTESIAN_POINT('Ctrl Pts',(-2.10823418017326,-2.84374236629767,
-3.4605683014601));
#48359=CARTESIAN_POINT('Ctrl Pts',(-2.13054463355673,-2.8272108697142,-3.46150461562032));
#48360=CARTESIAN_POINT('Ctrl Pts',(-2.15265877543496,-2.81041477835907,
-3.46244092978054));
#48361=CARTESIAN_POINT('Ctrl Pts',(-2.17456960835048,-2.79335766031483,
-3.46337724394076));
#48362=CARTESIAN_POINT('Ctrl Pts',(-2.30508009238466,-2.69175802050364,
-3.46895433974217));
#48363=CARTESIAN_POINT('Ctrl Pts',(-2.42837651672354,-2.58089661856788,
-3.47453143554359));
#48364=CARTESIAN_POINT('Ctrl Pts',(-2.5433709048767,-2.46202800977271,-3.480108531345));
#48365=CARTESIAN_POINT('Ctrl Pts',(-2.67767119664131,-2.3232030714498,-3.48662194130664));
#48366=CARTESIAN_POINT('Ctrl Pts',(-2.80066707596171,-2.17344287527037,
-3.49313535126827));
#48367=CARTESIAN_POINT('Ctrl Pts',(-2.91067619386607,-2.01467029405205,
-3.49964876122991));
#48368=CARTESIAN_POINT('Ctrl Pts',(-2.96568075281904,-1.93528400344175,
-3.50290546621077));
#48369=CARTESIAN_POINT('Ctrl Pts',(-3.01743874035383,-1.85364279298029,
-3.50616217119164));
#48370=CARTESIAN_POINT('Ctrl Pts',(-3.06572992939683,-1.76999999999985,
-3.5094188761725));
#48371=CARTESIAN_POINT('Ctrl Pts',(-3.11402111843984,-1.6863572070194,-3.51267558115337));
#48372=CARTESIAN_POINT('Ctrl Pts',(-3.15884548692774,-1.60071286973475,
-3.51593228613423));
#48373=CARTESIAN_POINT('Ctrl Pts',(-3.20009375183195,-1.51338437905234,
-3.51918899111509));
#48374=CARTESIAN_POINT('Ctrl Pts',(-3.28259028163917,-1.33872739769007,
-3.52570240107673));
#48375=CARTESIAN_POINT('Ctrl Pts',(-3.350788476346,-1.15732974354807,-3.53221581103837));
#48376=CARTESIAN_POINT('Ctrl Pts',(-3.40386425373005,-0.971609809982892,
-3.538729221));
#48377=CARTESIAN_POINT('Ctrl Pts',(-3.44931029458254,-0.812587444152017,
-3.54430631680142));
#48378=CARTESIAN_POINT('Ctrl Pts',(-3.48367087278858,-0.650378907510944,
-3.54988341260283));
#48379=CARTESIAN_POINT('Ctrl Pts',(-3.50640349986333,-0.486553692971483,
-3.55546050840425));
#48380=CARTESIAN_POINT('Ctrl Pts',(-3.51021998094721,-0.45904979602653,
-3.55639682256447));
#48381=CARTESIAN_POINT('Ctrl Pts',(-3.51370875180592,-0.431500341699595,
-3.55733313672469));
#48382=CARTESIAN_POINT('Ctrl Pts',(-3.51687022111804,-0.4039131740079,-3.55826945088491));
#48383=CARTESIAN_POINT('Ctrl Pts',(-3.53886278150659,-0.21200479486206,
-3.56478286084664));
#48384=CARTESIAN_POINT('Ctrl Pts',(-3.54501434799336,-0.018297976412778,
-3.57129627080837));
#48385=CARTESIAN_POINT('Ctrl Pts',(-3.53547893630661,0.174620099336988,
-3.57780968077025));
#48386=CARTESIAN_POINT('Ctrl Pts',(-3.52594352461999,0.367538175083959,
-3.58432309073203));
#48387=CARTESIAN_POINT('Ctrl Pts',(-3.50072047066892,0.559691489813732,
-3.59083650069397));
#48388=CARTESIAN_POINT('Ctrl Pts',(-3.45994007730116,0.748501474870884,
-3.59734991065576));
#48389=CARTESIAN_POINT('Ctrl Pts',(-3.45127413373233,0.788624105885788,
-3.59873402783826));
#48390=CARTESIAN_POINT('Ctrl Pts',(-3.44190579926218,0.828594815438887,
-3.60011814502075));
#48391=CARTESIAN_POINT('Ctrl Pts',(-3.43183653862866,0.868388146010993,
-3.60150226220324));
#48392=CARTESIAN_POINT('Ctrl Pts',(-3.39452164469186,1.01585517102254,-3.60663155498258));
#48393=CARTESIAN_POINT('Ctrl Pts',(-3.34757990374054,1.16088584063295,-3.61176084776184));
#48394=CARTESIAN_POINT('Ctrl Pts',(-3.2915666257629,1.30230683044729,-3.61689014054109));
#48395=CARTESIAN_POINT('Ctrl Pts',(-3.22043841014641,1.48188965472389,-3.62340355050273));
#48396=CARTESIAN_POINT('Ctrl Pts',(-3.13467840856183,1.65567399227211,-3.62991696046437));
#48397=CARTESIAN_POINT('Ctrl Pts',(-3.03537185704593,1.82135003611944,-3.636430370426));
#48398=CARTESIAN_POINT('Ctrl Pts',(-2.97889140575354,1.91557803600459,-3.64013486251106));
#48399=CARTESIAN_POINT('Ctrl Pts',(-2.91802588924534,2.00718573517956,-3.64383935459613));
#48400=CARTESIAN_POINT('Ctrl Pts',(-2.85298611916,2.09572665294942,-3.64754384668119));
#48401=CARTESIAN_POINT('Ctrl Pts',(-2.80366994606909,2.16286248723415,-3.65035276455776));
#48402=CARTESIAN_POINT('Ctrl Pts',(-2.75195394466873,2.228235150624,-3.65316168243433));
#48403=CARTESIAN_POINT('Ctrl Pts',(-2.6979962409409,2.29169861659425,-3.65597060031091));
#48404=CARTESIAN_POINT('Ctrl Pts',(-2.57287736583807,2.43885976178261,-3.66248401027264));
#48405=CARTESIAN_POINT('Ctrl Pts',(-2.43570729771941,2.57575738080365,-3.66899742023437));
#48406=CARTESIAN_POINT('Ctrl Pts',(-2.2883737003719,2.70066337612947,-3.67551083019609));
#48407=CARTESIAN_POINT('Ctrl Pts',(-2.15209022701611,2.81620133347544,-3.68153572980457));
#48408=CARTESIAN_POINT('Ctrl Pts',(-2.00709305852713,2.92148977050388,-3.68756062941305));
#48409=CARTESIAN_POINT('Ctrl Pts',(-1.85491010713434,3.01511334686633,-3.69358552902153));
#48410=CARTESIAN_POINT('Ctrl Pts',(-1.84257082313618,3.02270452503107,-3.69407403937469));
#48411=CARTESIAN_POINT('Ctrl Pts',(-1.83018430263193,3.03021901994261,-3.69456254972784));
#48412=CARTESIAN_POINT('Ctrl Pts',(-1.81775158326284,3.03765643862568,-3.695051060081));
#48413=CARTESIAN_POINT('Ctrl Pts',(-1.65198355467242,3.13682108606072,-3.70156447004264));
#48414=CARTESIAN_POINT('Ctrl Pts',(-1.47802896465355,3.22226797334726,-3.70807788000427));
#48415=CARTESIAN_POINT('Ctrl Pts',(-1.2983289646543,3.29309365754754,-3.71459128996591));
#48416=CARTESIAN_POINT('Ctrl Pts',(-1.11862896465245,3.36391934174885,-3.72110469992764));
#48417=CARTESIAN_POINT('Ctrl Pts',(-0.933161824865596,3.42013406708304,
-3.72761810988937));
#48418=CARTESIAN_POINT('Ctrl Pts',(-0.744333208107735,3.46082430384987,
-3.73413151985108));
#48419=CARTESIAN_POINT('Ctrl Pts',(-0.691224574103849,3.47226855911735,
-3.73596343660032));
#48420=CARTESIAN_POINT('Ctrl Pts',(-0.637851134403885,3.48248437574009,
-3.73779535334955));
#48421=CARTESIAN_POINT('Ctrl Pts',(-0.58426852474683,3.4914510294415,-3.73962727009879));
#48422=CARTESIAN_POINT('Ctrl Pts',(-0.447337289462379,3.51436545961875,
-3.74430876331116));
#48423=CARTESIAN_POINT('Ctrl Pts',(-0.309040015184776,3.5291212435739,-3.74899025652354));
#48424=CARTESIAN_POINT('Ctrl Pts',(-0.17036733400844,3.53574588879975,-3.75367174973592));
#48425=CARTESIAN_POINT('Ctrl Pts',(0.0225694026298665,3.5449628262702,-3.76018515969764));
#48426=CARTESIAN_POINT('Ctrl Pts',(0.216252460440131,3.5384455628299,-3.76669856965937));
#48427=CARTESIAN_POINT('Ctrl Pts',(0.408132200521637,3.51626167940836,-3.7732119796211));
#48428=CARTESIAN_POINT('Ctrl Pts',(0.530455029403651,3.50211951216048,-3.77736426131508));
#48429=CARTESIAN_POINT('Ctrl Pts',(0.652051243402925,3.48160781812733,-3.78151654300907));
#48430=CARTESIAN_POINT('Ctrl Pts',(0.772227074543825,3.45474533726317,-3.78566882470305));
#48431=CARTESIAN_POINT('Ctrl Pts',(0.840563129972376,3.43947041913817,-3.7880299529707));
#48432=CARTESIAN_POINT('Ctrl Pts',(0.908439919140494,3.4221421540496,-3.79039108123835));
#48433=CARTESIAN_POINT('Ctrl Pts',(0.975740479931958,3.40281153553916,-3.792752209506));
#48434=CARTESIAN_POINT('Ctrl Pts',(1.16139585032783,3.34948607885153,-3.79926561946764));
#48435=CARTESIAN_POINT('Ctrl Pts',(1.34266063505881,3.28092736671375,-3.80577902942927));
#48436=CARTESIAN_POINT('Ctrl Pts',(1.51718923345482,3.19817302383904,-3.81229243939091));
#48437=CARTESIAN_POINT('Ctrl Pts',(1.69171783185335,3.11541868096314,-3.81880584935264));
#48438=CARTESIAN_POINT('Ctrl Pts',(1.85953065547441,3.01845588995455,-3.82531925931437));
#48439=CARTESIAN_POINT('Ctrl Pts',(2.0182261341945,2.90832651285219,-3.83183266927608));
#48440=CARTESIAN_POINT('Ctrl Pts',(2.1769216129123,2.79819713575142,-3.8383460792377));
#48441=CARTESIAN_POINT('Ctrl Pts',(2.32647647226952,2.67492498658273,-3.8448594891993));
#48442=CARTESIAN_POINT('Ctrl Pts',(2.4650724946873,2.54039012878225,-3.85137289916092));
#48443=CARTESIAN_POINT('Ctrl Pts',(2.60366851710708,2.40585527097982,-3.85788630912264));
#48444=CARTESIAN_POINT('Ctrl Pts',(2.73132470195812,2.26004289611969,-3.86439971908436));
#48445=CARTESIAN_POINT('Ctrl Pts',(2.84624348913382,2.10478420563982,-3.87091312904609));
#48446=CARTESIAN_POINT('Ctrl Pts',(2.88646538330249,2.05044323345657,-3.87319284059367));
#48447=CARTESIAN_POINT('Ctrl Pts',(2.92512609682342,1.99494564818121,-3.87547255214125));
#48448=CARTESIAN_POINT('Ctrl Pts',(2.96214566964451,1.93837381116374,-3.87775226368882));
#48449=CARTESIAN_POINT('Ctrl Pts',(3.03089546691971,1.83331310867443,-3.88198596210288));
#48450=CARTESIAN_POINT('Ctrl Pts',(3.09398468320899,1.72454722201944,-3.88621966051694));
#48451=CARTESIAN_POINT('Ctrl Pts',(3.1511361795063,1.61275723470709,-3.890453358931));
#48452=CARTESIAN_POINT('Ctrl Pts',(3.23906193351585,1.4407719051538,-3.89696676889264));
#48453=CARTESIAN_POINT('Ctrl Pts',(3.31294544834883,1.26161606945278,-3.90348017885427));
#48454=CARTESIAN_POINT('Ctrl Pts',(3.37182604181743,1.07765228385916,-3.90999358881607));
#48455=CARTESIAN_POINT('Ctrl Pts',(3.41341027855843,0.947728430153869,-3.91459366442481));
#48456=CARTESIAN_POINT('Ctrl Pts',(3.44751202204771,0.815396531481927,-3.91919374003363));
#48457=CARTESIAN_POINT('Ctrl Pts',(3.47377603053233,0.681527761501758,-3.92379381564241));
#48458=CARTESIAN_POINT('Ctrl Pts',(3.48470016177703,0.625846999226429,-3.92570714999559));
#48459=CARTESIAN_POINT('Ctrl Pts',(3.49426846685995,0.569900396495106,-3.92762048434877));
#48460=CARTESIAN_POINT('Ctrl Pts',(3.50248075017427,0.513755641688056,-3.92953381870193));
#48461=CARTESIAN_POINT('Ctrl Pts',(3.53043716451462,0.322626577048128,-3.93604722866373));
#48462=CARTESIAN_POINT('Ctrl Pts',(3.54267920096763,0.129214760060477,-3.94256063862537));
#48463=CARTESIAN_POINT('Ctrl Pts',(3.53921539307674,-0.063907964441538,
-3.949074048587));
#48464=CARTESIAN_POINT('Ctrl Pts',(3.53575158518584,-0.257030688943553,
-3.95558745854864));
#48465=CARTESIAN_POINT('Ctrl Pts',(3.51657975088695,-0.449888254626207,
-3.96210086851027));
#48466=CARTESIAN_POINT('Ctrl Pts',(3.48168686891133,-0.639875553680029,
-3.96861427847191));
#48467=CARTESIAN_POINT('Ctrl Pts',(3.47950604488335,-0.651749862803495,
-3.96902137012339));
#48468=CARTESIAN_POINT('Ctrl Pts',(3.47726383116518,-0.663612839943919,
-3.96942846177487));
#48469=CARTESIAN_POINT('Ctrl Pts',(3.4749602294045,-0.675463843633017,-3.96983555342635));
#48470=CARTESIAN_POINT('Ctrl Pts',(3.4404065224946,-0.853227255282967,-3.9759418717366));
#48471=CARTESIAN_POINT('Ctrl Pts',(3.39203987700435,-1.02829625861096,-3.98204819004685));
#48472=CARTESIAN_POINT('Ctrl Pts',(3.33067938429338,-1.19866546298495,-3.98815450835708));
#48473=CARTESIAN_POINT('Ctrl Pts',(3.26522815424471,-1.38039271933565,-3.9946679183187));
#48474=CARTESIAN_POINT('Ctrl Pts',(3.18498800540492,-1.55679625758723,-4.0011813282803));
#48475=CARTESIAN_POINT('Ctrl Pts',(3.09091242647188,-1.72550011744132,-4.00769473824192));
#48476=CARTESIAN_POINT('Ctrl Pts',(3.05151811292345,-1.79614515441368,-4.01042224007829));
#48477=CARTESIAN_POINT('Ctrl Pts',(3.00969732231895,-1.86543959636863,-4.01314974191466));
#48478=CARTESIAN_POINT('Ctrl Pts',(2.965524256836,-1.9332009419914,-4.01587724375104));
#48479=CARTESIAN_POINT('Ctrl Pts',(2.90420984622655,-2.02725705794212,-4.01966315187639));
#48480=CARTESIAN_POINT('Ctrl Pts',(2.83836319021171,-2.11835920742328,-4.02344906000174));
#48481=CARTESIAN_POINT('Ctrl Pts',(2.76835115646748,-2.20612920640356,-4.02723496812709));
#48482=CARTESIAN_POINT('Ctrl Pts',(2.64789998255489,-2.35713181047166,-4.03374837808873));
#48483=CARTESIAN_POINT('Ctrl Pts',(2.5151152522304,-2.49828401989007,-4.04026178805037));
#48484=CARTESIAN_POINT('Ctrl Pts',(2.37177668926012,-2.62775728359333,-4.046775198012));
#48485=CARTESIAN_POINT('Ctrl Pts',(2.26068970700779,-2.7280986979979,-4.05182307237195));
#48486=CARTESIAN_POINT('Ctrl Pts',(2.14325235121661,-2.82143218116641,-4.05687094673191));
#48487=CARTESIAN_POINT('Ctrl Pts',(2.02032602960248,-2.90686820033367,-4.06191882109186));
#48488=CARTESIAN_POINT('Ctrl Pts',(1.98463716576339,-2.93167260686741,-4.06338435669354));
#48489=CARTESIAN_POINT('Ctrl Pts',(1.94848569380674,-2.95581139752882,-4.06484989229522));
#48490=CARTESIAN_POINT('Ctrl Pts',(1.91189931312508,-2.97927230421048,-4.06631542789691));
#48491=CARTESIAN_POINT('Ctrl Pts',(1.7492952138987,-3.08354169426571,-4.07282883785864));
#48492=CARTESIAN_POINT('Ctrl Pts',(1.57811819344313,-3.17441162854151,-4.07934224782037));
#48493=CARTESIAN_POINT('Ctrl Pts',(1.40073455162058,-3.25085348915537,-4.0858556577821));
#48494=CARTESIAN_POINT('Ctrl Pts',(1.22335090980063,-3.32729534976811,-4.09236906774373));
#48495=CARTESIAN_POINT('Ctrl Pts',(1.03973833991381,-3.38931797648445,-4.09888247770537));
#48496=CARTESIAN_POINT('Ctrl Pts',(0.852266212883417,-3.43586620221265,
-4.105395887667));
#48497=CARTESIAN_POINT('Ctrl Pts',(0.827660202824008,-3.44197572968566,
-4.1062507829177));
#48498=CARTESIAN_POINT('Ctrl Pts',(0.802988161574587,-3.44781855384957,
-4.1071056781684));
#48499=CARTESIAN_POINT('Ctrl Pts',(0.778255563408939,-3.4533922855685,-4.1079605734191));
#48500=CARTESIAN_POINT('Ctrl Pts',(0.614551565234618,-3.49028457488758,
-4.11361908813004));
#48501=CARTESIAN_POINT('Ctrl Pts',(0.448194483402658,-3.51538663874368,
-4.11927760284097));
#48502=CARTESIAN_POINT('Ctrl Pts',(0.280916493409238,-3.52865236474662,
-4.12493611755191));
#48503=CARTESIAN_POINT('Ctrl Pts',(0.0883659422379453,-3.54392229268905,
-4.13144952751364));
#48504=CARTESIAN_POINT('Ctrl Pts',(-0.105427797081422,-3.54351519011934,
-4.13796293747536));
#48505=CARTESIAN_POINT('Ctrl Pts',(-0.297910355108321,-3.52735115969274,
-4.14447634743708));
#48506=CARTESIAN_POINT('Ctrl Pts',(-0.39174565726025,-3.51947119023151,
-4.14765163665841));
#48507=CARTESIAN_POINT('Ctrl Pts',(-0.485270507195668,-3.50784551008206,
-4.15082692587973));
#48508=CARTESIAN_POINT('Ctrl Pts',(-0.578173906335351,-3.49246545208883,
-4.15400221510106));
#48509=CARTESIAN_POINT('Ctrl Pts',(-0.675841470420018,-3.47629669170343,
-4.15734033584135));
#48510=CARTESIAN_POINT('Ctrl Pts',(-0.772822162007415,-3.45597860468362,
-4.16067845658163));
#48511=CARTESIAN_POINT('Ctrl Pts',(-0.868777181623859,-3.43163722187875,
-4.16401657732192));
#48512=CARTESIAN_POINT('Ctrl Pts',(-1.05600659280207,-3.38414181425924,
-4.17052998728364));
#48513=CARTESIAN_POINT('Ctrl Pts',(-1.23933903044262,-3.32133059983808,
-4.17704339724537));
#48514=CARTESIAN_POINT('Ctrl Pts',(-1.41638310527089,-3.24410123108816,
-4.1835568072071));
#48515=CARTESIAN_POINT('Ctrl Pts',(-1.56576369723281,-3.17893910221207,
-4.18905248412663));
#48516=CARTESIAN_POINT('Ctrl Pts',(-1.71068137496023,-3.10350315118168,
-4.19454816104616));
#48517=CARTESIAN_POINT('Ctrl Pts',(-1.8496449190945,-3.0183461818135,-4.20004383796569));
#48518=CARTESIAN_POINT('Ctrl Pts',(-1.87537929041651,-3.00257613878509,
-4.2010615710078));
#48519=CARTESIAN_POINT('Ctrl Pts',(-1.90090948182522,-2.98647275324273,
-4.2020793040499));
#48520=CARTESIAN_POINT('Ctrl Pts',(-1.9262280359204,-2.97004283162531,-4.203097037092));
#48521=CARTESIAN_POINT('Ctrl Pts',(-2.08826475442685,-2.86489264910712,
-4.20961044705364));
#48522=CARTESIAN_POINT('Ctrl Pts',(-2.24161193500656,-2.74638268846562,
-4.21612385701527));
#48523=CARTESIAN_POINT('Ctrl Pts',(-2.38436956161414,-2.61627287473533,
-4.22263726697691));
#48524=CARTESIAN_POINT('Ctrl Pts',(-2.52712718822379,-2.48616306100314,
-4.22915067693864));
#48525=CARTESIAN_POINT('Ctrl Pts',(-2.65931321192137,-2.34443748176244,
-4.23566408690037));
#48526=CARTESIAN_POINT('Ctrl Pts',(-2.77901650300382,-2.19283463489973,
-4.2421774968621));
#48527=CARTESIAN_POINT('Ctrl Pts',(-2.80295746726397,-2.16251367792641,
-4.24348019550718));
#48528=CARTESIAN_POINT('Ctrl Pts',(-2.8263985174789,-2.13179828445587,-4.24478289415227));
#48529=CARTESIAN_POINT('Ctrl Pts',(-2.84932404264,-2.10070285857735,-4.24608559279736));
#48530=CARTESIAN_POINT('Ctrl Pts',(-2.94102467796757,-1.97632314257066,
-4.25129630411391));
#48531=CARTESIAN_POINT('Ctrl Pts',(-3.02447624802702,-1.84586260784311,
-4.25650701543049));
#48532=CARTESIAN_POINT('Ctrl Pts',(-3.09909838196629,-1.71055094354732,
-4.26171772674717));
#48533=CARTESIAN_POINT('Ctrl Pts',(-3.19237634749372,-1.54141082262935,
-4.26823113670897));
#48534=CARTESIAN_POINT('Ctrl Pts',(-3.27187296306989,-1.36467341810391,
-4.27474454667094));
#48535=CARTESIAN_POINT('Ctrl Pts',(-3.33649164232266,-1.18264363939907,
-4.28125795663274));
#48536=CARTESIAN_POINT('Ctrl Pts',(-3.37243570168691,-1.08138980308597,
-4.2848810327624));
#48537=CARTESIAN_POINT('Ctrl Pts',(-3.40377624648734,-0.978494886681129,
-4.288504108892));
#48538=CARTESIAN_POINT('Ctrl Pts',(-3.43031568918,-0.874376505038574,-4.29212718502158));
#48539=CARTESIAN_POINT('Ctrl Pts',(-3.45148771161571,-0.791315351960366,
-4.29501751885376));
#48540=CARTESIAN_POINT('Ctrl Pts',(-3.4696043187652,-0.707475623527939,
-4.29790785268592));
#48541=CARTESIAN_POINT('Ctrl Pts',(-3.48465193556905,-0.623091478798857,
-4.30079818651808));
#48542=CARTESIAN_POINT('Ctrl Pts',(-3.51856196218893,-0.432930562863846,
-4.3073115964797));
#48543=CARTESIAN_POINT('Ctrl Pts',(-3.5368901719826,-0.240004247211696,
-4.3138250064413));
#48544=CARTESIAN_POINT('Ctrl Pts',(-3.539499078369,-0.0468671734762678,
-4.32033841640292));
#48545=CARTESIAN_POINT('Ctrl Pts',(-3.5418797031369,0.129370235321772,-4.32628189722653));
#48546=CARTESIAN_POINT('Ctrl Pts',(-3.53116871553553,0.305802937702781,
-4.33222537805016));
#48547=CARTESIAN_POINT('Ctrl Pts',(-3.50724735526867,0.480433126417416,
-4.33816885887379));
#48548=CARTESIAN_POINT('Ctrl Pts',(-3.50495350076762,0.497178672654429,
-4.33873878801189));
#48549=CARTESIAN_POINT('Ctrl Pts',(-3.50253818434456,0.513907643630247,
-4.33930871714999));
#48550=CARTESIAN_POINT('Ctrl Pts',(-3.50000197035076,0.530618368380382,
-4.33987864628809));
#48551=CARTESIAN_POINT('Ctrl Pts',(-3.47101696083347,0.72159614750572,-4.34639205624973));
#48552=CARTESIAN_POINT('Ctrl Pts',(-3.42624638929545,0.910161095558849,
-4.35290546621137));
#48553=CARTESIAN_POINT('Ctrl Pts',(-3.36654108656219,1.09385548621155,-4.359418876173));
#48554=CARTESIAN_POINT('Ctrl Pts',(-3.30683578382893,1.27754987686425,-4.36593228613464));
#48555=CARTESIAN_POINT('Ctrl Pts',(-3.23218964468241,1.45639693625083,-4.37244569609627));
#48556=CARTESIAN_POINT('Ctrl Pts',(-3.14342402551079,1.62795644980454,-4.37895910605791));
#48557=CARTESIAN_POINT('Ctrl Pts',(-3.11956799202827,1.67406359734405,-4.38070960504141));
#48558=CARTESIAN_POINT('Ctrl Pts',(-3.09469253710093,1.71964329765716,-4.38246010402492));
#48559=CARTESIAN_POINT('Ctrl Pts',(-3.06881449123183,1.76464659872848,-4.38421060300842));
#48560=CARTESIAN_POINT('Ctrl Pts',(-2.99840323711153,1.88709552257745,-4.38897351398665));
#48561=CARTESIAN_POINT('Ctrl Pts',(-2.92056891533613,2.00527672011598,-4.39373642496487));
#48562=CARTESIAN_POINT('Ctrl Pts',(-2.83599569248695,2.11840306211022,-4.39849933594308));
#48563=CARTESIAN_POINT('Ctrl Pts',(-2.72033951610409,2.27310640345701,-4.4050127459047));
#48564=CARTESIAN_POINT('Ctrl Pts',(-2.59207227250994,2.4183755860845,-4.4115261558663));
#48565=CARTESIAN_POINT('Ctrl Pts',(-2.45286430442405,2.55228290197142,-4.41803956582792));
#48566=CARTESIAN_POINT('Ctrl Pts',(-2.36585966860048,2.63597464327796,-4.42211043094773));
#48567=CARTESIAN_POINT('Ctrl Pts',(-2.27457583085879,2.71523107830464,-4.42618129606755));
#48568=CARTESIAN_POINT('Ctrl Pts',(-2.17944162265286,2.78955806776767,-4.43025216118736));
#48569=CARTESIAN_POINT('Ctrl Pts',(-2.12236049549604,2.83415473196168,-4.43269470602927));
#48570=CARTESIAN_POINT('Ctrl Pts',(-2.06389331379296,2.87697685360123,-4.43513725087118));
#48571=CARTESIAN_POINT('Ctrl Pts',(-2.00416594676152,2.91796018932203,-4.43757979571309));
#48572=CARTESIAN_POINT('Ctrl Pts',(-1.84489401826728,3.02724836391952,-4.44409320567473));
#48573=CARTESIAN_POINT('Ctrl Pts',(-1.67666686505147,3.12346020277471,-4.45060661563637));
#48574=CARTESIAN_POINT('Ctrl Pts',(-1.50177399217723,3.20544206238398,-4.457120025598));
#48575=CARTESIAN_POINT('Ctrl Pts',(-1.33016037878431,3.28588675363412,-4.46351130844821));
#48576=CARTESIAN_POINT('Ctrl Pts',(-1.15210659968557,3.35263728831822,-4.46990259129843));
#48577=CARTESIAN_POINT('Ctrl Pts',(-0.969815634171214,3.40456423580433,
-4.47629387414864));
#48578=CARTESIAN_POINT('Ctrl Pts',(-0.966332347704576,3.40555647605564,
-4.47641600126006));
#48579=CARTESIAN_POINT('Ctrl Pts',(-0.962847514285249,3.40654330398007,
-4.47653812837148));
#48580=CARTESIAN_POINT('Ctrl Pts',(-0.959361151106016,3.4075247180546,-4.47666025548291));
#48581=CARTESIAN_POINT('Ctrl Pts',(-0.773422808690397,3.45986651288758,
-4.48317366544464));
#48582=CARTESIAN_POINT('Ctrl Pts',(-0.583164165584344,3.49679998871353,
-4.48968707540637));
#48583=CARTESIAN_POINT('Ctrl Pts',(-0.391189760153187,3.51811400704572,
-4.4962004853681));
#48584=CARTESIAN_POINT('Ctrl Pts',(-0.199215354724813,3.53942802537761,
-4.50271389532973));
#48585=CARTESIAN_POINT('Ctrl Pts',(-0.00550164725985493,3.54512763200719,
-4.50922730529137));
#48586=CARTESIAN_POINT('Ctrl Pts',(0.187394174250291,3.53498576596323,-4.515740715253));
#48587=CARTESIAN_POINT('Ctrl Pts',(0.25249707115236,3.53156285688057,-4.51793900992778));
#48588=CARTESIAN_POINT('Ctrl Pts',(0.317505759619646,3.52633524440815,-4.52013730460256));
#48589=CARTESIAN_POINT('Ctrl Pts',(0.382317719199291,3.519294412462,-4.52233559927734));
#48590=CARTESIAN_POINT('Ctrl Pts',(0.509539551996122,3.50547369865527,-4.5266507145642));
#48591=CARTESIAN_POINT('Ctrl Pts',(0.636003219410405,3.48466589220727,-4.53096582985105));
#48592=CARTESIAN_POINT('Ctrl Pts',(0.760965615923843,3.45710192869036,-4.53528094513791));
#48593=CARTESIAN_POINT('Ctrl Pts',(0.949588923572606,3.41549576463196,-4.54179435509963));
#48594=CARTESIAN_POINT('Ctrl Pts',(1.13480966416368,3.35849703359421,-4.54830776506137));
#48595=CARTESIAN_POINT('Ctrl Pts',(1.31419238471769,3.28686253261049,-4.55482117502308));
#48596=CARTESIAN_POINT('Ctrl Pts',(1.43863859651384,3.23716631742433,-4.55933983319209));
#48597=CARTESIAN_POINT('Ctrl Pts',(1.56028265268397,3.18042068936791,-4.56385849136109));
#48598=CARTESIAN_POINT('Ctrl Pts',(1.67827226002658,3.1168898314225,-4.5683771495301));
#48599=CARTESIAN_POINT('Ctrl Pts',(1.73035851482898,3.08884427275604,-4.5703719013227));
#48600=CARTESIAN_POINT('Ctrl Pts',(1.78173265010367,3.05947655931791,-4.57236665311531));
#48601=CARTESIAN_POINT('Ctrl Pts',(1.83233522030034,3.02883524024529,-4.57436140490792));
#48602=CARTESIAN_POINT('Ctrl Pts',(1.99756644657541,2.92878295623329,-4.58087481486964));
#48603=CARTESIAN_POINT('Ctrl Pts',(2.15456198585818,2.81515968928226,-4.58738822483137));
#48604=CARTESIAN_POINT('Ctrl Pts',(2.30134084431348,2.68960344508741,-4.59390163479326));
#48605=CARTESIAN_POINT('Ctrl Pts',(2.44811970276666,2.56404720089438,-4.60041504475506));
#48606=CARTESIAN_POINT('Ctrl Pts',(2.58469882886557,2.42654092551998,-4.60692845471703));
#48607=CARTESIAN_POINT('Ctrl Pts',(2.70905533377063,2.2787296820682,-4.61344186467883));
#48608=CARTESIAN_POINT('Ctrl Pts',(2.71527320777415,2.2713390619411,-4.61376753773073));
#48609=CARTESIAN_POINT('Ctrl Pts',(2.72146047398848,2.26392273951171,-4.61409321078263));
#48610=CARTESIAN_POINT('Ctrl Pts',(2.72761687942599,2.25648092371001,-4.61441888383453));
#48611=CARTESIAN_POINT('Ctrl Pts',(2.84458761721353,2.1150875905972,-4.62060662074442));
#48612=CARTESIAN_POINT('Ctrl Pts',(2.95041694207574,1.96449093844901,-4.62679435765416));
#48613=CARTESIAN_POINT('Ctrl Pts',(3.04403466981377,1.80667228922409,-4.63298209456391));
#48614=CARTESIAN_POINT('Ctrl Pts',(3.14257968705312,1.64054732673751,-4.63949550452564));
#48615=CARTESIAN_POINT('Ctrl Pts',(3.2276089004457,1.4664013198912,-4.64600891448737));
#48616=CARTESIAN_POINT('Ctrl Pts',(3.29789079596611,1.2864798567823,-4.65252232444909));
#48617=CARTESIAN_POINT('Ctrl Pts',(3.32644295523914,1.21338640599696,-4.65516841014813));
#48618=CARTESIAN_POINT('Ctrl Pts',(3.35256060096538,1.13933993490305,-4.65781449584717));
#48619=CARTESIAN_POINT('Ctrl Pts',(3.37615800564866,1.06449853024478,-4.66046058154621));
#48620=CARTESIAN_POINT('Ctrl Pts',(3.410646236963,0.955115837089003,-4.66432790580881));
#48621=CARTESIAN_POINT('Ctrl Pts',(3.43975080156849,0.844035097395934,-4.6681952300714));
#48622=CARTESIAN_POINT('Ctrl Pts',(3.46340847798809,0.731814199250707,-4.672062554334));
#48623=CARTESIAN_POINT('Ctrl Pts',(3.50325311857094,0.542809950770156,-4.67857596429564));
#48624=CARTESIAN_POINT('Ctrl Pts',(3.52765418600473,0.350559382295599,-4.68508937425727));
#48625=CARTESIAN_POINT('Ctrl Pts',(3.53632795873358,0.157598006434378,-4.69160278421891));
#48626=CARTESIAN_POINT('Ctrl Pts',(3.54294168510181,0.0104655210122198,
-4.69656924028791));
#48627=CARTESIAN_POINT('Ctrl Pts',(3.54040940290031,-0.137092750504991,
-4.70153569635691));
#48628=CARTESIAN_POINT('Ctrl Pts',(3.52859722973483,-0.283904192124258,
-4.7065021524259));
#48629=CARTESIAN_POINT('Ctrl Pts',(3.52491796890859,-0.329633083703001,
-4.70804910631863));
#48630=CARTESIAN_POINT('Ctrl Pts',(3.52033846393456,-0.375289512400935,
-4.70959606021136));
#48631=CARTESIAN_POINT('Ctrl Pts',(3.5148682535165,-0.420839119723915,-4.71114301410408));
#48632=CARTESIAN_POINT('Ctrl Pts',(3.49183607188734,-0.612624581126916,
-4.7176564240657));
#48633=CARTESIAN_POINT('Ctrl Pts',(3.4530172602035,-0.80249780061272,-4.7241698340273));
#48634=CARTESIAN_POINT('Ctrl Pts',(3.3991184205719,-0.987978897271879,-4.73068324398892));
#48635=CARTESIAN_POINT('Ctrl Pts',(3.34521958093952,-1.17345999393373,-4.73719665395063));
#48636=CARTESIAN_POINT('Ctrl Pts',(3.2762331580479,-1.35457174622048,-4.74371006391237));
#48637=CARTESIAN_POINT('Ctrl Pts',(3.19284833403879,-1.52881164096968,-4.75022347387409));
#48638=CARTESIAN_POINT('Ctrl Pts',(3.18294627225166,-1.5495028665505,-4.7509969502069));
#48639=CARTESIAN_POINT('Ctrl Pts',(3.17284133069424,-1.57009682188359,-4.7517704265397));
#48640=CARTESIAN_POINT('Ctrl Pts',(3.1625347146805,-1.5905892551004,-4.7525439028725));
#48641=CARTESIAN_POINT('Ctrl Pts',(3.08604977345116,-1.74266269493216,-4.75828383650133));
#48642=CARTESIAN_POINT('Ctrl Pts',(2.99845761324308,-1.88914457163618,-4.76402377013017));
#48643=CARTESIAN_POINT('Ctrl Pts',(2.90086776956525,-2.02860868265436,-4.769763703759));
#48644=CARTESIAN_POINT('Ctrl Pts',(2.79012734971569,-2.18686607528926,-4.77627711372064));
#48645=CARTESIAN_POINT('Ctrl Pts',(2.6665030824214,-2.33610851677235,-4.78279052368227));
#48646=CARTESIAN_POINT('Ctrl Pts',(2.53155468743157,-2.47431060311237,-4.78930393364391));
#48647=CARTESIAN_POINT('Ctrl Pts',(2.46745412259722,-2.53995667319974,-4.7923978071025));
#48648=CARTESIAN_POINT('Ctrl Pts',(2.40079731960751,-2.60311185453884,-4.79549168056109));
#48649=CARTESIAN_POINT('Ctrl Pts',(2.33176068881981,-2.66354877749069,-4.79858555401968));
#48650=CARTESIAN_POINT('Ctrl Pts',(2.25545721933669,-2.7303473285424,-4.80200509052282));
#48651=CARTESIAN_POINT('Ctrl Pts',(2.17624654724241,-2.79382517537667,-4.80542462702596));
#48652=CARTESIAN_POINT('Ctrl Pts',(2.09446454668198,-2.85378693812754,-4.80884416352909));
#48653=CARTESIAN_POINT('Ctrl Pts',(1.93868913775044,-2.96799994403061,-4.81535757349073));
#48654=CARTESIAN_POINT('Ctrl Pts',(1.77358024536384,-3.06946424600634,-4.82187098345237));
#48655=CARTESIAN_POINT('Ctrl Pts',(1.60134875634575,-3.15690183524312,-4.828384393414));
#48656=CARTESIAN_POINT('Ctrl Pts',(1.45818170002382,-3.22958414400259,-4.83379865149271));
#48657=CARTESIAN_POINT('Ctrl Pts',(1.31007763847309,-3.29257884054208,-4.83921290957143));
#48658=CARTESIAN_POINT('Ctrl Pts',(1.15835136238572,-3.34511914903784,-4.84462716765014));
#48659=CARTESIAN_POINT('Ctrl Pts',(1.12754931718851,-3.35578538957768,-4.84572631953306));
#48660=CARTESIAN_POINT('Ctrl Pts',(1.09659801000313,-3.36602081032388,-4.84682547141599));
#48661=CARTESIAN_POINT('Ctrl Pts',(1.06551003781568,-3.37582359101795,-4.84792462329891));
#48662=CARTESIAN_POINT('Ctrl Pts',(0.8812873558714,-3.43391340591755,-4.85443803326064));
#48663=CARTESIAN_POINT('Ctrl Pts',(0.692289542666389,-3.47680428037546,
-4.86095144322237));
#48664=CARTESIAN_POINT('Ctrl Pts',(0.501080685143525,-3.50414476472143,
-4.86746485318408));
#48665=CARTESIAN_POINT('Ctrl Pts',(0.309871827623432,-3.53148524906699,
-4.8739782631457));
#48666=CARTESIAN_POINT('Ctrl Pts',(0.116428217970221,-3.54327886708705,
-4.8804916731073));
#48667=CARTESIAN_POINT('Ctrl Pts',(-0.0766918204989502,-3.53915174526628,
-4.88700508306892));
#48668=CARTESIAN_POINT('Ctrl Pts',(-0.112902286566704,-3.53837790011881,
-4.88822636291264));
#48669=CARTESIAN_POINT('Ctrl Pts',(-0.149100544630311,-3.53704430365368,
-4.88944764275636));
#48670=CARTESIAN_POINT('Ctrl Pts',(-0.185269285100072,-3.53514855303133,
-4.89066892260008));
#48671=CARTESIAN_POINT('Ctrl Pts',(-0.341998049399606,-3.52693376178892,
-4.89596105271809));
#48672=CARTESIAN_POINT('Ctrl Pts',(-0.49817233969735,-3.50816226468903,
-4.90125318283612));
#48673=CARTESIAN_POINT('Ctrl Pts',(-0.652411741910373,-3.47918285964478,
-4.90654531295425));
#48674=CARTESIAN_POINT('Ctrl Pts',(-0.842245398493005,-3.44351579697333,
-4.91305872260848));
#48675=CARTESIAN_POINT('Ctrl Pts',(-1.02917125546825,-3.3923861748366,-4.91957213226287));
#48676=CARTESIAN_POINT('Ctrl Pts',(-1.21071388570407,-3.32640898834169,
-4.92608554191631));
#48677=CARTESIAN_POINT('',(-1.210751307373,-3.326511877582,-4.926085542839));
#48678=CARTESIAN_POINT('Ctrl Pts',(-3.841349734859,-1.189096377216,-1.539436278284));
#48679=CARTESIAN_POINT('Ctrl Pts',(-3.994234933732,-0.6952040995074,-1.554783500506));
#48680=CARTESIAN_POINT('Ctrl Pts',(-4.10706259235,0.3520715397013,-1.58547794495));
#48681=CARTESIAN_POINT('Ctrl Pts',(-3.672853039324,1.871418570915,-1.631519611617));
#48682=CARTESIAN_POINT('Ctrl Pts',(-2.698930474802,3.115729236588,-1.677561278284));
#48683=CARTESIAN_POINT('Ctrl Pts',(-1.328423408128,3.902218173295,-1.72360294495));
#48684=CARTESIAN_POINT('Ctrl Pts',(0.2372868317335,4.115301255755,-1.769644611617));
#48685=CARTESIAN_POINT('Ctrl Pts',(1.76812922683,3.723671568578,-1.815686278284));
#48686=CARTESIAN_POINT('Ctrl Pts',(3.039157943544,2.784875152802,-1.86172794495));
#48687=CARTESIAN_POINT('Ctrl Pts',(3.863604450802,1.43686161852,-1.907769611617));
#48688=CARTESIAN_POINT('Ctrl Pts',(4.120322345675,-0.1222883131347,-1.953811278284));
#48689=CARTESIAN_POINT('Ctrl Pts',(3.771588791194,-1.663468860739,-1.99985294495));
#48690=CARTESIAN_POINT('Ctrl Pts',(2.868647652528,-2.960214740138,-2.045894611617));
#48691=CARTESIAN_POINT('Ctrl Pts',(1.544179572608,-3.821978559474,-2.091936278284));
#48692=CARTESIAN_POINT('Ctrl Pts',(-0.007194482043365,-4.122130383809,-2.13797794495));
#48693=CARTESIAN_POINT('Ctrl Pts',(-1.557511359811,-3.816565082075,-2.184019611617));
#48694=CARTESIAN_POINT('Ctrl Pts',(-2.8789632535,-2.950183256454,-2.230061278284));
#48695=CARTESIAN_POINT('Ctrl Pts',(-3.777372403381,-1.65029342477,-2.27610294495));
#48696=CARTESIAN_POINT('Ctrl Pts',(-4.120724108895,-0.1079049583238,-2.322144611617));
#48697=CARTESIAN_POINT('Ctrl Pts',(-3.85856533025,1.45033935817,-2.368186278284));
#48698=CARTESIAN_POINT('Ctrl Pts',(-3.029418396237,2.795466837973,-2.41422794495));
#48699=CARTESIAN_POINT('Ctrl Pts',(-1.755120427756,3.7298207659,-2.460269611617));
#48700=CARTESIAN_POINT('Ctrl Pts',(-0.2229202576515,4.11610461728,-2.506311278284));
#48701=CARTESIAN_POINT('Ctrl Pts',(1.342036425525,3.897556785247,-2.55235294495));
#48702=CARTESIAN_POINT('Ctrl Pts',(2.709790601495,3.106291286681,-2.598394611617));
#48703=CARTESIAN_POINT('Ctrl Pts',(3.679360726381,1.858578840628,-2.644436278284));
#48704=CARTESIAN_POINT('Ctrl Pts',(4.108275511099,0.337761730468,-2.69047794495));
#48705=CARTESIAN_POINT('Ctrl Pts',(3.933509042705,-1.232687013245,-2.736519611617));
#48706=CARTESIAN_POINT('Ctrl Pts',(3.180741984619,-2.622001351819,-2.782561278284));
#48707=CARTESIAN_POINT('Ctrl Pts',(1.960587989627,-3.626031632045,-2.82860294495));
#48708=CARTESIAN_POINT('Ctrl Pts',(0.4523398268471,-4.097242895254,-2.874644611617));
#48709=CARTESIAN_POINT('Ctrl Pts',(-1.122376388713,-3.966394068133,-2.920686278284));
#48710=CARTESIAN_POINT('Ctrl Pts',(-2.532167544361,-3.252712435637,-2.96672794495));
#48711=CARTESIAN_POINT('Ctrl Pts',(-3.569875067316,-2.061068331088,-3.012769611617));
#48712=CARTESIAN_POINT('Ctrl Pts',(-4.083015372648,-0.566565202236,-3.058811278284));
#48713=CARTESIAN_POINT('Ctrl Pts',(-3.99618621878,1.011190568834,-3.10485294495));
#48714=CARTESIAN_POINT('Ctrl Pts',(-3.322146519342,2.44035922882,-3.150894611617));
#48715=CARTESIAN_POINT('Ctrl Pts',(-2.159941513463,3.510934821395,-3.196936278284));
#48716=CARTESIAN_POINT('Ctrl Pts',(-0.6803487871228,4.065604037474,-3.24297794495));
#48717=CARTESIAN_POINT('Ctrl Pts',(0.8992162529668,4.022862263621,-3.289019611617));
#48718=CARTESIAN_POINT('Ctrl Pts',(2.346647994561,3.388990093123,-3.335061278284));
#48719=CARTESIAN_POINT('Ctrl Pts',(3.44925685411,2.257130438418,-3.38110294495));
#48720=CARTESIAN_POINT('Ctrl Pts',(4.045022466568,0.7936018564908,-3.427144611617));
#48721=CARTESIAN_POINT('Ctrl Pts',(4.046401401479,-0.7865407553148,-3.473186278284));
#48722=CARTESIAN_POINT('Ctrl Pts',(3.453191034373,-2.251106914784,-3.51922794495));
#48723=CARTESIAN_POINT('Ctrl Pts',(2.352559320954,-3.384889260088,-3.565269611617));
#48724=CARTESIAN_POINT('Ctrl Pts',(0.9062360990033,-4.021286708819,-3.611311278284));
#48725=CARTESIAN_POINT('Ctrl Pts',(-0.6732519368415,-4.066785277243,-3.65735294495));
#48726=CARTESIAN_POINT('Ctrl Pts',(-2.15381048955,-3.514699281129,-3.703394611617));
#48727=CARTESIAN_POINT('Ctrl Pts',(-3.31788223124,-2.446153748497,-3.749436278284));
#48728=CARTESIAN_POINT('Ctrl Pts',(-3.994415272659,-1.018163685866,-3.79547794495));
#48729=CARTESIAN_POINT('Ctrl Pts',(-4.083997996179,0.559438136759,-3.841519611617));
#48730=CARTESIAN_POINT('Ctrl Pts',(-3.573466871112,2.054834587688,-3.887561278284));
#48731=CARTESIAN_POINT('Ctrl Pts',(-2.537840738919,3.248288017621,-3.93360294495));
#48732=CARTESIAN_POINT('Ctrl Pts',(-1.129297339352,3.964429111665,-3.979644611617));
#48733=CARTESIAN_POINT('Ctrl Pts',(0.4451881037925,4.098026136172,-4.025686278284));
#48734=CARTESIAN_POINT('Ctrl Pts',(1.954256387077,3.629447979702,-4.07172794495));
#48735=CARTESIAN_POINT('Ctrl Pts',(3.176160888763,2.627548795309,-4.117769611617));
#48736=CARTESIAN_POINT('Ctrl Pts',(3.931351600467,1.239550408822,-4.163811278284));
#48737=CARTESIAN_POINT('Ctrl Pts',(4.108858787154,-0.3305909566808,-4.20985294495));
#48738=CARTESIAN_POINT('Ctrl Pts',(3.682598847576,-1.852154203613,-4.255894611617));
#48739=CARTESIAN_POINT('Ctrl Pts',(2.715208365118,-3.101557505068,-4.301936278284));
#48740=CARTESIAN_POINT('Ctrl Pts',(1.348835432798,-3.89520697252,-4.34797794495));
#48741=CARTESIAN_POINT('Ctrl Pts',(-0.2157304961352,-4.116493321879,-4.394019611617));
#48742=CARTESIAN_POINT('Ctrl Pts',(-1.748628398844,-3.732856309759,-4.440061278284));
#48743=CARTESIAN_POINT('Ctrl Pts',(-2.599181877855,-3.111506871542,-4.470755722728));
#48744=CARTESIAN_POINT('Ctrl Pts',(-2.950462537646,-2.7321582666,-4.48610294495));
#48745=CARTESIAN_POINT('Ctrl Pts',(-3.681382861754,-1.139578358183,-1.636116911815));
#48746=CARTESIAN_POINT('Ctrl Pts',(-3.827901400756,-0.6662534353805,-1.651464134037));
#48747=CARTESIAN_POINT('Ctrl Pts',(-3.936030531775,0.337410082869,-1.682158578481));
#48748=CARTESIAN_POINT('Ctrl Pts',(-3.519902941929,1.793486334144,-1.728200245148));
#48749=CARTESIAN_POINT('Ctrl Pts',(-2.586537826753,2.985979669945,-1.774241911815));
#48750=CARTESIAN_POINT('Ctrl Pts',(-1.27310333747,3.739716531309,-1.820283578481));
#48751=CARTESIAN_POINT('Ctrl Pts',(0.2274054006946,3.943926109203,-1.866325245148));
#48752=CARTESIAN_POINT('Ctrl Pts',(1.694498309787,3.568605214716,-1.912366911815));
#48753=CARTESIAN_POINT('Ctrl Pts',(2.912597066077,2.668903475936,-1.958408578481));
#48754=CARTESIAN_POINT('Ctrl Pts',(3.702710815604,1.377025811821,-2.004450245148));
#48755=CARTESIAN_POINT('Ctrl Pts',(3.948738103854,-0.1171958116913,-2.050491911815));
#48756=CARTESIAN_POINT('Ctrl Pts',(3.614527001144,-1.594196357445,-2.096533578481));
#48757=CARTESIAN_POINT('Ctrl Pts',(2.749187403738,-2.836941326264,-2.142575245148));
#48758=CARTESIAN_POINT('Ctrl Pts',(1.479874681153,-3.662818368022,-2.188616911815));
#48759=CARTESIAN_POINT('Ctrl Pts',(-0.006894879331943,-3.950470849129,-2.234658578481));
#48760=CARTESIAN_POINT('Ctrl Pts',(-1.492651287375,-3.657630326242,-2.280700245148));
#48761=CARTESIAN_POINT('Ctrl Pts',(-2.759073427987,-2.827327587693,-2.326741911815));
#48762=CARTESIAN_POINT('Ctrl Pts',(-3.620069764041,-1.581569591459,-2.372783578481));
#48763=CARTESIAN_POINT('Ctrl Pts',(-3.949123136288,-0.1034114287139,-2.418825245148));
#48764=CARTESIAN_POINT('Ctrl Pts',(-3.697881541177,1.389942292534,-2.464866911815));
#48765=CARTESIAN_POINT('Ctrl Pts',(-2.903263106658,2.679054087298,-2.510908578481));
#48766=CARTESIAN_POINT('Ctrl Pts',(-1.682031241369,3.574498338538,-2.556950245148));
#48767=CARTESIAN_POINT('Ctrl Pts',(-0.2136370996395,3.944696016021,-2.602991911815));
#48768=CARTESIAN_POINT('Ctrl Pts',(1.286149462504,3.73524925932,-2.649033578481));
#48769=CARTESIAN_POINT('Ctrl Pts',(2.59694570082,2.976934748386,-2.695075245148));
#48770=CARTESIAN_POINT('Ctrl Pts',(3.526139626754,1.781181293913,-2.741116911815));
#48771=CARTESIAN_POINT('Ctrl Pts',(3.93719294046,0.3236961827811,-2.787158578481));
#48772=CARTESIAN_POINT('Ctrl Pts',(3.76970434245,-1.181353731811,-2.833200245148));
#48773=CARTESIAN_POINT('Ctrl Pts',(3.048285065944,-2.512812294202,-2.879241911815));
#48774=CARTESIAN_POINT('Ctrl Pts',(1.878942434863,-3.475031337359,-2.925283578481));
#48775=CARTESIAN_POINT('Ctrl Pts',(0.4335028573765,-3.926619760277,-2.971325245148));
#48776=CARTESIAN_POINT('Ctrl Pts',(-1.075636817015,-3.801219923529,-3.017366911815));
#48777=CARTESIAN_POINT('Ctrl Pts',(-2.426719472144,-3.117258422503,-3.063408578481));
#48778=CARTESIAN_POINT('Ctrl Pts',(-3.421213323057,-1.975238433022,-3.109450245148));
#48779=CARTESIAN_POINT('Ctrl Pts',(-3.912984720121,-0.5429714994837,-3.155491911815));
#48780=CARTESIAN_POINT('Ctrl Pts',(-3.829771427655,0.969081152984,-3.201533578481));
#48781=CARTESIAN_POINT('Ctrl Pts',(-3.183801034714,2.33873436724,-3.247575245148));
#48782=CARTESIAN_POINT('Ctrl Pts',(-2.069994199668,3.364727549519,-3.293616911815));
#48783=CARTESIAN_POINT('Ctrl Pts',(-0.6520167487486,3.896298452185,-3.339658578481));
#48784=CARTESIAN_POINT('Ctrl Pts',(0.861769828621,3.855336591224,-3.385700245148));
#48785=CARTESIAN_POINT('Ctrl Pts',(2.248925587626,3.247861014648,-3.431741911815));
#48786=CARTESIAN_POINT('Ctrl Pts',(3.305618062651,2.163135847104,-3.477783578481));
#48787=CARTESIAN_POINT('Ctrl Pts',(3.87657396792,0.760553574966,-3.523825245148));
#48788=CARTESIAN_POINT('Ctrl Pts',(3.87789547929,-0.7537865220682,-3.569866911815));
#48789=CARTESIAN_POINT('Ctrl Pts',(3.309388410261,-2.157363163489,-3.615908578481));
#48790=CARTESIAN_POINT('Ctrl Pts',(2.254590746275,-3.243930954253,-3.661950245148));
#48791=CARTESIAN_POINT('Ctrl Pts',(0.8684973443836,-3.853826647885,-3.707991911815));
#48792=CARTESIAN_POINT('Ctrl Pts',(-0.64521543546,-3.897430501112,-3.754033578481));
#48793=CARTESIAN_POINT('Ctrl Pts',(-2.064118492452,-3.368335244341,-3.800075245148));
#48794=CARTESIAN_POINT('Ctrl Pts',(-3.179714326077,-2.344287583402,-3.846116911815));
#48795=CARTESIAN_POINT('Ctrl Pts',(-3.828074229756,-0.9757638856968,-3.892158578481));
#48796=CARTESIAN_POINT('Ctrl Pts',(-3.913926423865,0.5361412292629,-3.938200245148));
#48797=CARTESIAN_POINT('Ctrl Pts',(-3.424655551922,1.969264283907,-3.984241911815));
#48798=CARTESIAN_POINT('Ctrl Pts',(-2.432156415579,3.113018252307,-4.030283578481));
#48799=CARTESIAN_POINT('Ctrl Pts',(-1.082269555721,3.799336794534,-4.076325245148));
#48800=CARTESIAN_POINT('Ctrl Pts',(0.4266489564036,3.927370384378,-4.122366911815));
#48801=CARTESIAN_POINT('Ctrl Pts',(1.872874501785,3.478305416675,-4.168408578481));
#48802=CARTESIAN_POINT('Ctrl Pts',(3.043894742506,2.51812872327,-4.214450245148));
#48803=CARTESIAN_POINT('Ctrl Pts',(3.767636743447,1.187931312243,-4.260491911815));
#48804=CARTESIAN_POINT('Ctrl Pts',(3.937751926915,-0.3168240244129,-4.306533578481));
#48805=CARTESIAN_POINT('Ctrl Pts',(3.529242901566,-1.775024200642,-4.352575245148));
#48806=CARTESIAN_POINT('Ctrl Pts',(2.602137850332,-2.972398097546,-4.398616911815));
#48807=CARTESIAN_POINT('Ctrl Pts',(1.29266533598,-3.73299730079,-4.444658578481));
#48808=CARTESIAN_POINT('Ctrl Pts',(-0.2067467442558,-3.945068533638,-4.490700245148));
#48809=CARTESIAN_POINT('Ctrl Pts',(-1.67580956263,-3.577407472023,-4.536741911815));
#48810=CARTESIAN_POINT('Ctrl Pts',(-2.490943100776,-2.981933138547,-4.567436356259));
#48811=CARTESIAN_POINT('Ctrl Pts',(-2.827595238666,-2.618381900244,-4.582783578481));
#48812=CARTESIAN_POINT('Ctrl Pts',(-3.521415988649,-1.090060339149,-1.732797545346));
#48813=CARTESIAN_POINT('Ctrl Pts',(-3.66156786778,-0.6373027712535,-1.748144767568));
#48814=CARTESIAN_POINT('Ctrl Pts',(-3.764998471199,0.3227486260367,-1.778839212012));
#48815=CARTESIAN_POINT('Ctrl Pts',(-3.366952844534,1.715554097372,-1.824880878679));
#48816=CARTESIAN_POINT('Ctrl Pts',(-2.474145178704,2.856230103303,-1.870922545346));
#48817=CARTESIAN_POINT('Ctrl Pts',(-1.217783266811,3.577214889324,-1.916964212012));
#48818=CARTESIAN_POINT('Ctrl Pts',(0.2175239696557,3.772550962651,-1.963005878679));
#48819=CARTESIAN_POINT('Ctrl Pts',(1.620867392743,3.413538860853,-2.009047545346));
#48820=CARTESIAN_POINT('Ctrl Pts',(2.78603618861,2.552931799069,-2.055089212012));
#48821=CARTESIAN_POINT('Ctrl Pts',(3.541817180406,1.317190005122,-2.101130878679));
#48822=CARTESIAN_POINT('Ctrl Pts',(3.777153862034,-0.1121033102479,-2.147172545346));
#48823=CARTESIAN_POINT('Ctrl Pts',(3.457465211094,-1.524923854152,-2.193214212012));
#48824=CARTESIAN_POINT('Ctrl Pts',(2.629727154949,-2.71366791239,-2.239255878679));
#48825=CARTESIAN_POINT('Ctrl Pts',(1.415569789697,-3.50365817657,-2.285297545346));
#48826=CARTESIAN_POINT('Ctrl Pts',(-0.006595276620518,-3.778811314449,-2.331339212012));
#48827=CARTESIAN_POINT('Ctrl Pts',(-1.427791214939,-3.498695570408,-2.377380878679));
#48828=CARTESIAN_POINT('Ctrl Pts',(-2.639183602474,-2.704471918932,-2.423422545346));
#48829=CARTESIAN_POINT('Ctrl Pts',(-3.462767124701,-1.512845758149,-2.469464212012));
#48830=CARTESIAN_POINT('Ctrl Pts',(-3.77752216368,-0.09891789910402,-2.515505878679));
#48831=CARTESIAN_POINT('Ctrl Pts',(-3.537197752104,1.329545226898,-2.561547545346));
#48832=CARTESIAN_POINT('Ctrl Pts',(-2.77710781708,2.562641336623,-2.607589212012));
#48833=CARTESIAN_POINT('Ctrl Pts',(-1.608942054981,3.419175911177,-2.653630878679));
#48834=CARTESIAN_POINT('Ctrl Pts',(-0.2043539416274,3.773287414762,-2.699672545346));
#48835=CARTESIAN_POINT('Ctrl Pts',(1.230262499482,3.572941733393,-2.745714212012));
#48836=CARTESIAN_POINT('Ctrl Pts',(2.484100800144,2.84757821009,-2.791755878679));
#48837=CARTESIAN_POINT('Ctrl Pts',(3.372918527128,1.703783747197,-2.837797545346));
#48838=CARTESIAN_POINT('Ctrl Pts',(3.76611036982,0.3096306350943,-2.883839212012));
#48839=CARTESIAN_POINT('Ctrl Pts',(3.605899642196,-1.130020450377,-2.929880878679));
#48840=CARTESIAN_POINT('Ctrl Pts',(2.915828147269,-2.403623236585,-2.975922545346));
#48841=CARTESIAN_POINT('Ctrl Pts',(1.797296880098,-3.324031042672,-3.021964212012));
#48842=CARTESIAN_POINT('Ctrl Pts',(0.4146658879059,-3.7559966253,-3.068005878679));
#48843=CARTESIAN_POINT('Ctrl Pts',(-1.028897245317,-3.636045778925,-3.114047545346));
#48844=CARTESIAN_POINT('Ctrl Pts',(-2.321271399928,-2.981804409369,-3.160089212012));
#48845=CARTESIAN_POINT('Ctrl Pts',(-3.272551578798,-1.889408534956,-3.206130878679));
#48846=CARTESIAN_POINT('Ctrl Pts',(-3.742954067594,-0.5193777967315,-3.252172545346));
#48847=CARTESIAN_POINT('Ctrl Pts',(-3.66335663653,0.9269717371343,-3.298214212012));
#48848=CARTESIAN_POINT('Ctrl Pts',(-3.045455550085,2.237109505659,-3.344255878679));
#48849=CARTESIAN_POINT('Ctrl Pts',(-1.980046885873,3.218520277643,-3.390297545346));
#48850=CARTESIAN_POINT('Ctrl Pts',(-0.6236847103744,3.726992866897,-3.436339212012));
#48851=CARTESIAN_POINT('Ctrl Pts',(0.8243234042752,3.687810918827,-3.482380878679));
#48852=CARTESIAN_POINT('Ctrl Pts',(2.151203180692,3.106731936173,-3.528422545346));
#48853=CARTESIAN_POINT('Ctrl Pts',(3.161979271192,2.06914125579,-3.574464212012));
#48854=CARTESIAN_POINT('Ctrl Pts',(3.708125469273,0.7275052934411,-3.620505878679));
#48855=CARTESIAN_POINT('Ctrl Pts',(3.709389557102,-0.7210322888216,-3.666547545346));
#48856=CARTESIAN_POINT('Ctrl Pts',(3.16558578615,-2.063619412194,-3.712589212012));
#48857=CARTESIAN_POINT('Ctrl Pts',(2.156622171596,-3.102972648419,-3.758630878679));
#48858=CARTESIAN_POINT('Ctrl Pts',(0.8307585897638,-3.686366586951,-3.804672545346));
#48859=CARTESIAN_POINT('Ctrl Pts',(-0.6171789340784,-3.72807572498,-3.850714212012));
#48860=CARTESIAN_POINT('Ctrl Pts',(-1.974426495353,-3.221971207554,-3.896755878679));
#48861=CARTESIAN_POINT('Ctrl Pts',(-3.041546420915,-2.242421418306,-3.942797545346));
#48862=CARTESIAN_POINT('Ctrl Pts',(-3.661733186854,-0.9333640855279,-3.988839212012));
#48863=CARTESIAN_POINT('Ctrl Pts',(-3.743854851551,0.5128443217669,-4.034880878679));
#48864=CARTESIAN_POINT('Ctrl Pts',(-3.275844232732,1.883693980126,-4.080922545346));
#48865=CARTESIAN_POINT('Ctrl Pts',(-2.326472092238,2.977748486993,-4.126964212012));
#48866=CARTESIAN_POINT('Ctrl Pts',(-1.03524177209,3.634244477402,-4.173005878679));
#48867=CARTESIAN_POINT('Ctrl Pts',(0.4081098090146,3.756714632584,-4.219047545346));
#48868=CARTESIAN_POINT('Ctrl Pts',(1.791492616494,3.327162853648,-4.265089212012));
#48869=CARTESIAN_POINT('Ctrl Pts',(2.911628596249,2.40870865123,-4.311130878679));
#48870=CARTESIAN_POINT('Ctrl Pts',(3.603921886428,1.136312215665,-4.357172545346));
#48871=CARTESIAN_POINT('Ctrl Pts',(3.766645066676,-0.303057092145,-4.403214212012));
#48872=CARTESIAN_POINT('Ctrl Pts',(3.375886955555,-1.697894197672,-4.449255878679));
#48873=CARTESIAN_POINT('Ctrl Pts',(2.489067335545,-2.843238690024,-4.495297545346));
#48874=CARTESIAN_POINT('Ctrl Pts',(1.236495239162,-3.570787629061,-4.541339212012));
#48875=CARTESIAN_POINT('Ctrl Pts',(-0.1977629923763,-3.773643745397,-4.587380878679));
#48876=CARTESIAN_POINT('Ctrl Pts',(-1.602990726415,-3.421958634286,-4.633422545346));
#48877=CARTESIAN_POINT('Ctrl Pts',(-2.382704323698,-2.852359405552,-4.66411698979));
#48878=CARTESIAN_POINT('Ctrl Pts',(-2.704727939686,-2.504605533888,-4.679464212012));
#48879=CARTESIAN_POINT('Ctrl Pts',(-3.361449115544,-1.040542320116,-1.829478178877));
#48880=CARTESIAN_POINT('Ctrl Pts',(-3.495234334804,-0.6083521071266,-1.844825401099));
#48881=CARTESIAN_POINT('Ctrl Pts',(-3.593966410624,0.3080871692045,-1.875519845544));
#48882=CARTESIAN_POINT('Ctrl Pts',(-3.214002747139,1.6376218606,-1.92156151221));
#48883=CARTESIAN_POINT('Ctrl Pts',(-2.361752530656,2.726480536661,-1.967603178877));
#48884=CARTESIAN_POINT('Ctrl Pts',(-1.162463196152,3.414713247338,-2.013644845544));
#48885=CARTESIAN_POINT('Ctrl Pts',(0.2076425386167,3.6011758161,-2.05968651221));
#48886=CARTESIAN_POINT('Ctrl Pts',(1.5472364757,3.258472506991,-2.105728178877));
#48887=CARTESIAN_POINT('Ctrl Pts',(2.659475311144,2.436960122203,-2.151769845544));
#48888=CARTESIAN_POINT('Ctrl Pts',(3.380923545207,1.257354198423,-2.19781151221));
#48889=CARTESIAN_POINT('Ctrl Pts',(3.605569620214,-0.1070108088044,-2.243853178877));
#48890=CARTESIAN_POINT('Ctrl Pts',(3.300403421044,-1.455651350858,-2.289894845544));
#48891=CARTESIAN_POINT('Ctrl Pts',(2.510266906159,-2.590394498517,-2.33593651221));
#48892=CARTESIAN_POINT('Ctrl Pts',(1.351264898242,-3.344497985119,-2.381978178877));
#48893=CARTESIAN_POINT('Ctrl Pts',(-0.006295673909096,-3.607151779769,-2.428019845544));
#48894=CARTESIAN_POINT('Ctrl Pts',(-1.362931142503,-3.339760814575,-2.47406151221));
#48895=CARTESIAN_POINT('Ctrl Pts',(-2.519293776961,-2.581616250171,-2.520103178877));
#48896=CARTESIAN_POINT('Ctrl Pts',(-3.305464485361,-1.444121924838,-2.566144845544));
#48897=CARTESIAN_POINT('Ctrl Pts',(-3.605921191072,-0.09442436949412,-2.61218651221));
#48898=CARTESIAN_POINT('Ctrl Pts',(-3.376513963031,1.269148161262,-2.658228178877));
#48899=CARTESIAN_POINT('Ctrl Pts',(-2.650952527502,2.446228585948,-2.704269845544));
#48900=CARTESIAN_POINT('Ctrl Pts',(-1.535852868594,3.263853483815,-2.75031151221));
#48901=CARTESIAN_POINT('Ctrl Pts',(-0.1950707836154,3.601878813503,-2.796353178877));
#48902=CARTESIAN_POINT('Ctrl Pts',(1.174375536461,3.410634207467,-2.842394845544));
#48903=CARTESIAN_POINT('Ctrl Pts',(2.371255899469,2.718221671795,-2.88843651221));
#48904=CARTESIAN_POINT('Ctrl Pts',(3.219697427502,1.626386200482,-2.934478178877));
#48905=CARTESIAN_POINT('Ctrl Pts',(3.595027799181,0.2955650874075,-2.980519845544));
#48906=CARTESIAN_POINT('Ctrl Pts',(3.442094941941,-1.078687168943,-3.02656151221));
#48907=CARTESIAN_POINT('Ctrl Pts',(2.783371228594,-2.294434178968,-3.072603178877));
#48908=CARTESIAN_POINT('Ctrl Pts',(1.715651325333,-3.173030747985,-3.118644845544));
#48909=CARTESIAN_POINT('Ctrl Pts',(0.3958289184352,-3.585373490323,-3.16468651221));
#48910=CARTESIAN_POINT('Ctrl Pts',(-0.9821576736188,-3.470871634321,-3.210728178877));
#48911=CARTESIAN_POINT('Ctrl Pts',(-2.215823327712,-2.846350396235,-3.256769845544));
#48912=CARTESIAN_POINT('Ctrl Pts',(-3.123889834539,-1.80357863689,-3.30281151221));
#48913=CARTESIAN_POINT('Ctrl Pts',(-3.572923415067,-0.4957840939792,-3.348853178877));
#48914=CARTESIAN_POINT('Ctrl Pts',(-3.496941845406,0.8848623212845,-3.394894845544));
#48915=CARTESIAN_POINT('Ctrl Pts',(-2.907110065457,2.135484644079,-3.44093651221));
#48916=CARTESIAN_POINT('Ctrl Pts',(-1.890099572078,3.072313005768,-3.486978178877));
#48917=CARTESIAN_POINT('Ctrl Pts',(-0.5953526720002,3.557687281609,-3.533019845544));
#48918=CARTESIAN_POINT('Ctrl Pts',(0.7868769799293,3.520285246431,-3.57906151221));
#48919=CARTESIAN_POINT('Ctrl Pts',(2.053480773757,2.965602857698,-3.625103178877));
#48920=CARTESIAN_POINT('Ctrl Pts',(3.018340479732,1.975146664475,-3.671144845544));
#48921=CARTESIAN_POINT('Ctrl Pts',(3.539676970626,0.6944570119162,-3.71718651221));
#48922=CARTESIAN_POINT('Ctrl Pts',(3.540883634913,-0.688278055575,-3.763228178877));
#48923=CARTESIAN_POINT('Ctrl Pts',(3.021783162038,-1.969875660898,-3.809269845544));
#48924=CARTESIAN_POINT('Ctrl Pts',(2.058653596917,-2.962014342585,-3.85531151221));
#48925=CARTESIAN_POINT('Ctrl Pts',(0.7930198351441,-3.518906526017,-3.901353178877));
#48926=CARTESIAN_POINT('Ctrl Pts',(-0.5891424326969,-3.558720948849,-3.947394845544));
#48927=CARTESIAN_POINT('Ctrl Pts',(-1.884734498254,-3.075607170766,-3.99343651221));
#48928=CARTESIAN_POINT('Ctrl Pts',(-2.903378515752,-2.140555253211,-4.039478178877));
#48929=CARTESIAN_POINT('Ctrl Pts',(-3.495392143951,-0.890964285359,-4.085519845544));
#48930=CARTESIAN_POINT('Ctrl Pts',(-3.573783279237,0.4895474142708,-4.13156151221));
#48931=CARTESIAN_POINT('Ctrl Pts',(-3.127032913541,1.798123676345,-4.177603178877));
#48932=CARTESIAN_POINT('Ctrl Pts',(-2.220787768898,2.842478721679,-4.223644845544));
#48933=CARTESIAN_POINT('Ctrl Pts',(-0.9882139884594,3.469152160271,-4.26968651221));
#48934=CARTESIAN_POINT('Ctrl Pts',(0.3895706616256,3.58605888079,-4.315728178877));
#48935=CARTESIAN_POINT('Ctrl Pts',(1.710110731203,3.176020290621,-4.361769845544));
#48936=CARTESIAN_POINT('Ctrl Pts',(2.779362449993,2.299288579191,-4.40781151221));
#48937=CARTESIAN_POINT('Ctrl Pts',(3.440207029409,1.084693119086,-4.453853178877));
#48938=CARTESIAN_POINT('Ctrl Pts',(3.595538206437,-0.2892901598772,-4.499894845544));
#48939=CARTESIAN_POINT('Ctrl Pts',(3.222531009545,-1.620764194701,-4.54593651221));
#48940=CARTESIAN_POINT('Ctrl Pts',(2.375996820758,-2.714079282501,-4.591978178877));
#48941=CARTESIAN_POINT('Ctrl Pts',(1.180325142345,-3.408577957331,-4.638019845544));
#48942=CARTESIAN_POINT('Ctrl Pts',(-0.1887792404969,-3.602218957155,-4.68406151221));
#48943=CARTESIAN_POINT('Ctrl Pts',(-1.530171890201,-3.26650979655,-4.730103178877));
#48944=CARTESIAN_POINT('Ctrl Pts',(-2.27446554662,-2.722785672557,-4.760797623321));
#48945=CARTESIAN_POINT('Ctrl Pts',(-2.581860640706,-2.390829167532,-4.776144845544));
#48946=CARTESIAN_POINT('',(-3.93911337870815,0.694572063117019,-1.60839731732686));
#48947=CARTESIAN_POINT('Ctrl Pts',(-3.9391476461815,0.694580681980914,-1.60831164028612));
#48948=CARTESIAN_POINT('Ctrl Pts',(-3.87575636899027,1.05329971993104,-1.61916055136511));
#48949=CARTESIAN_POINT('Ctrl Pts',(-3.76331552410144,1.40367728055008,-1.63004175976234));
#48950=CARTESIAN_POINT('Ctrl Pts',(-3.44908409131853,2.05768393665711,-1.65177420498472));
#48951=CARTESIAN_POINT('Ctrl Pts',(-3.24867678133451,2.36091786560673,-1.66242155380477));
#48952=CARTESIAN_POINT('Ctrl Pts',(-2.85427330231202,2.81251457419833,-1.68033258195991));
#48953=CARTESIAN_POINT('Ctrl Pts',(-2.68089218807246,2.97828559101128,-1.68755165834065));
#48954=CARTESIAN_POINT('Ctrl Pts',(-2.29199649028268,3.28815721323979,-1.70234773215377));
#48955=CARTESIAN_POINT('Ctrl Pts',(-2.07541513183239,3.42900620445079,-1.70993152711484));
#48956=CARTESIAN_POINT('Ctrl Pts',(-1.73246767296789,3.60753719420245,-1.72151186108472));
#48957=CARTESIAN_POINT('Ctrl Pts',(-1.6152980874153,3.66151208582675,-1.72539240561347));
#48958=CARTESIAN_POINT('Ctrl Pts',(-1.26155783509673,3.80419579142845,-1.73684399654552));
#48959=CARTESIAN_POINT('Ctrl Pts',(-1.01959031116382,3.87599732536495,-1.74426624699113));
#48960=CARTESIAN_POINT('Ctrl Pts',(-0.520819148694711,3.97409498843021,
-1.75936524951164));
#48961=CARTESIAN_POINT('Ctrl Pts',(-0.264781011431223,3.9992682257859,-1.76708259008009));
#48962=CARTESIAN_POINT('Ctrl Pts',(0.24893970914982,4.00053834585732,-1.78247105983387));
#48963=CARTESIAN_POINT('Ctrl Pts',(0.505470134302276,3.97626597241578,-1.79004184896571));
#48964=CARTESIAN_POINT('Ctrl Pts',(1.01240067258279,3.87819256282968,-1.8054348808173));
#48965=CARTESIAN_POINT('Ctrl Pts',(1.26150083420194,3.80449777615572,-1.81319367488307));
#48966=CARTESIAN_POINT('Ctrl Pts',(1.74342457165987,3.60956884353135,-1.82873460850295));
#48967=CARTESIAN_POINT('Ctrl Pts',(1.97457153864621,3.48830483716102,-1.83645395373821));
#48968=CARTESIAN_POINT('Ctrl Pts',(2.62992623847885,3.05858975308443,-1.85980733424332));
#48969=CARTESIAN_POINT('Ctrl Pts',(3.00637774151654,2.6901616353728,-1.87531400123001));
#48970=CARTESIAN_POINT('Ctrl Pts',(3.44781193210487,2.04384145685652,-1.89857824856414));
#48971=CARTESIAN_POINT('Ctrl Pts',(3.57243967653421,1.81757792873232,-1.90625597378683));
#48972=CARTESIAN_POINT('Ctrl Pts',(3.77617991548416,1.34412722685851,-1.92173915500655));
#48973=CARTESIAN_POINT('Ctrl Pts',(3.85474827892487,1.09817128411223,-1.92935993309336));
#48974=CARTESIAN_POINT('Ctrl Pts',(3.96319739898563,0.597574292783151,-1.94456013998803));
#48975=CARTESIAN_POINT('Ctrl Pts',(3.99320564673335,0.344047886583298,-1.95220040824628));
#48976=CARTESIAN_POINT('Ctrl Pts',(4.00458381732679,-0.162576490571243,
-1.96740990150124));
#48977=CARTESIAN_POINT('Ctrl Pts',(3.98641123253988,-0.413670763323244,
-1.97480775895236));
#48978=CARTESIAN_POINT('Ctrl Pts',(3.92319550876267,-0.790361327529153,
-1.98615799566182));
#48979=CARTESIAN_POINT('Ctrl Pts',(3.89526587387948,-0.9180352503498,-1.99006416710248));
#48980=CARTESIAN_POINT('Ctrl Pts',(3.79391229657841,-1.29288061633546,-2.00170958005469));
#48981=CARTESIAN_POINT('Ctrl Pts',(3.70261571485556,-1.53537175287446,-2.00945323725056));
#48982=CARTESIAN_POINT('Ctrl Pts',(3.47453219068466,-1.99840856444878,-2.02476565236659));
#48983=CARTESIAN_POINT('Ctrl Pts',(3.33842647584621,-2.21798524879933,-2.03243546445543));
#48984=CARTESIAN_POINT('Ctrl Pts',(2.86447884276471,-2.84079120359918,-2.05585926705293));
#48985=CARTESIAN_POINT('Ctrl Pts',(2.46970933926694,-3.18935455492974,-2.07121509202959));
#48986=CARTESIAN_POINT('Ctrl Pts',(1.79334333320813,-3.58483604994515,-2.09461011537361));
#48987=CARTESIAN_POINT('Ctrl Pts',(1.55647028382883,-3.69401257860335,-2.10241022000926));
#48988=CARTESIAN_POINT('Ctrl Pts',(1.06633238570733,-3.86369280979337,-2.11786329345988));
#48989=CARTESIAN_POINT('Ctrl Pts',(0.814729067481227,-3.92443178881597,
-2.12549294687453));
#48990=CARTESIAN_POINT('Ctrl Pts',(0.305940997637993,-3.99645945661362,
-2.14084188698538));
#48991=CARTESIAN_POINT('Ctrl Pts',(0.0497744729073863,-4.00787011059076,
-2.14855605117495));
#48992=CARTESIAN_POINT('Ctrl Pts',(-0.460511180924768,-3.98141866816329,
-2.16374520187095));
#48993=CARTESIAN_POINT('Ctrl Pts',(-0.713171682148684,-3.94404452875386,
-2.17125045661919));
#48994=CARTESIAN_POINT('Ctrl Pts',(-1.20616270496559,-3.82207313292113,
-2.1864759203107));
#48995=CARTESIAN_POINT('Ctrl Pts',(-1.44578608562418,-3.73812438180054,
-2.19409957806823));
#48996=CARTESIAN_POINT('Ctrl Pts',(-1.79243706317895,-3.57813833673693,
-2.20542588038207));
#48997=CARTESIAN_POINT('Ctrl Pts',(-1.90642404006754,-3.51871380126743,
-2.20922126752684));
#48998=CARTESIAN_POINT('Ctrl Pts',(-2.2318305682894,-3.32860139091786,-2.22042824021237));
#48999=CARTESIAN_POINT('Ctrl Pts',(-2.43459498834245,-3.18326446341512,
-2.22791388798638));
#49000=CARTESIAN_POINT('Ctrl Pts',(-2.81827082920698,-2.85037426083714,
-2.24312531473129));
#49001=CARTESIAN_POINT('Ctrl Pts',(-2.99678000710199,-2.66202820658115,
-2.25075054803303));
#49002=CARTESIAN_POINT('Ctrl Pts',(-3.31540162582115,-2.25250451580803,
-2.26622360816346));
#49003=CARTESIAN_POINT('Ctrl Pts',(-3.45476507159533,-2.03239459659418,
-2.27400186365226));
#49004=CARTESIAN_POINT('Ctrl Pts',(-3.80523178798918,-1.33796544403393,
-2.29725172660996));
#49005=CARTESIAN_POINT('Ctrl Pts',(-3.90874827153045,-0.910232814772706,
-2.31012052099671));
#49006=CARTESIAN_POINT('Ctrl Pts',(-3.98832494428433,-0.372437174862723,
-2.32636476587382));
#49007=CARTESIAN_POINT('Ctrl Pts',(-4.00260791525811,-0.158802003029431,
-2.33277805970415));
#49008=CARTESIAN_POINT('Ctrl Pts',(-3.99651941653082,0.269734882242017,
-2.34555535366208));
#49009=CARTESIAN_POINT('Ctrl Pts',(-3.97624197357851,0.483643897924661,
-2.35190371057797));
#49010=CARTESIAN_POINT('Ctrl Pts',(-3.93908532777216,0.694566072447258,
-2.35828102994364));
#49011=CARTESIAN_POINT('',(-3.48621875314954,0.61471493280625,-1.87404472598981));
#49012=CARTESIAN_POINT('Ctrl Pts',(-3.48611163489721,0.614695485491625,
-1.873914457161));
#49013=CARTESIAN_POINT('Ctrl Pts',(-3.45247823923436,0.804904617636081,
-1.880427867122));
#49014=CARTESIAN_POINT('Ctrl Pts',(-3.40329486078119,0.992351978567723,
-1.886941277084));
#49015=CARTESIAN_POINT('Ctrl Pts',(-3.33926661181778,1.17458628760328,-1.89345468704583));
#49016=CARTESIAN_POINT('Ctrl Pts',(-3.28724381166632,1.32265123070542,-1.89874681716394));
#49017=CARTESIAN_POINT('Ctrl Pts',(-3.22541325987337,1.46728788207019,-1.90403894728194));
#49018=CARTESIAN_POINT('Ctrl Pts',(-3.15416309562667,1.60712636907785,-1.90933107739992));
#49019=CARTESIAN_POINT('Ctrl Pts',(-3.13772049359028,1.63939729245812,-1.91055235724362));
#49020=CARTESIAN_POINT('Ctrl Pts',(-3.12077629297601,1.67141270174591,-1.91177363708731));
#49021=CARTESIAN_POINT('Ctrl Pts',(-3.10334122949876,1.70315880781664,-1.91299491693101));
#49022=CARTESIAN_POINT('Ctrl Pts',(-3.010355402605,1.87246922802227,-1.91950832689267));
#49023=CARTESIAN_POINT('Ctrl Pts',(-2.90342002496954,2.03409949917319,-1.92602173685433));
#49024=CARTESIAN_POINT('Ctrl Pts',(-2.78413804221371,2.18602098504228,-1.93253514681599));
#49025=CARTESIAN_POINT('Ctrl Pts',(-2.66485605945771,2.33794247091159,-1.93904855677766));
#49026=CARTESIAN_POINT('Ctrl Pts',(-2.53321256598554,2.48017394117643,-1.94556196673933));
#49027=CARTESIAN_POINT('Ctrl Pts',(-2.39079396961086,2.61067055624253,-1.952075376701));
#49028=CARTESIAN_POINT('Ctrl Pts',(-2.36676052640752,2.63269213956278,-1.95317452858396));
#49029=CARTESIAN_POINT('Ctrl Pts',(-2.34242073842935,2.65437904749335,-1.95427368046692));
#49030=CARTESIAN_POINT('Ctrl Pts',(-2.3177824805595,2.6757212808535,-1.95537283234988));
#49031=CARTESIAN_POINT('Ctrl Pts',(-2.19641810063612,2.78084993611871,-1.96078709042859));
#49032=CARTESIAN_POINT('Ctrl Pts',(-2.06781106235418,2.87761446755544,-1.96620134850729));
#49033=CARTESIAN_POINT('Ctrl Pts',(-1.93328280840194,2.96525962093555,-1.971615606586));
#49034=CARTESIAN_POINT('Ctrl Pts',(-1.7714438903673,3.07069767113915,-1.97812901654767));
#49035=CARTESIAN_POINT('Ctrl Pts',(-1.6010187810845,3.16295401534946,-1.98464242650933));
#49036=CARTESIAN_POINT('Ctrl Pts',(-1.42421971206299,3.24075297381787,-1.991155836471));
#49037=CARTESIAN_POINT('Ctrl Pts',(-1.33140030198562,3.28159738249964,-1.99457537297411));
#49038=CARTESIAN_POINT('Ctrl Pts',(-1.23682153800335,3.31845691336659,-1.99799490947721));
#49039=CARTESIAN_POINT('Ctrl Pts',(-1.14082056111593,3.35113838080967,-2.00141444598032));
#49040=CARTESIAN_POINT('Ctrl Pts',(-1.05396233511999,3.38070739538729,-2.00450831943888));
#49041=CARTESIAN_POINT('Ctrl Pts',(-0.965939942205691,3.40685628944164,
-2.00760219289745));
#49042=CARTESIAN_POINT('Ctrl Pts',(-0.877038495435007,3.42954597194126,
-2.01069606635601));
#49043=CARTESIAN_POINT('Ctrl Pts',(-0.689877780312868,3.47731366703263,
-2.01720947631767));
#49044=CARTESIAN_POINT('Ctrl Pts',(-0.498817901017613,3.50975420229228,
-2.02372288627933));
#49045=CARTESIAN_POINT('Ctrl Pts',(-0.306392768733605,3.52652952279029,
-2.03023629624099));
#49046=CARTESIAN_POINT('Ctrl Pts',(-0.136818383836607,3.54131275105748,
-2.03597622986983));
#49047=CARTESIAN_POINT('Ctrl Pts',(0.0338347226870868,3.54392884861796,
-2.04171616349867));
#49048=CARTESIAN_POINT('Ctrl Pts',(0.203776655436933,3.53413003081367,-2.0474560971275));
#49049=CARTESIAN_POINT('Ctrl Pts',(0.226676931195759,3.53280960550016,-2.04822957346034));
#49050=CARTESIAN_POINT('Ctrl Pts',(0.249564290458189,3.53126376392604,-2.04900304979317));
#49051=CARTESIAN_POINT('Ctrl Pts',(0.27243444834103,3.52949358819305,-2.049776526126));
#49052=CARTESIAN_POINT('Ctrl Pts',(0.46502303554917,3.51458701670047,-2.05628993608767));
#49053=CARTESIAN_POINT('Ctrl Pts',(0.656363625397378,3.4837751352979,-2.06280334604933));
#49054=CARTESIAN_POINT('Ctrl Pts',(0.843944386843304,3.43771235132368,-2.069316756011));
#49055=CARTESIAN_POINT('Ctrl Pts',(1.03152514828923,3.39164956734945,-2.07583016597267));
#49056=CARTESIAN_POINT('Ctrl Pts',(1.21536958570617,3.33033103466894,-2.08234357593433));
#49057=CARTESIAN_POINT('Ctrl Pts',(1.39297675817359,3.25438475836223,-2.088856985896));
#49058=CARTESIAN_POINT('Ctrl Pts',(1.43515898045606,3.23634729588709,-2.0904039397887));
#49059=CARTESIAN_POINT('Ctrl Pts',(1.47698836004088,3.2174850491827,-2.0919508936814));
#49060=CARTESIAN_POINT('Ctrl Pts',(1.5184303722474,3.19780693673633,-2.0934978475741));
#49061=CARTESIAN_POINT('Ctrl Pts',(1.65147889683793,3.13463085796226,-2.09846430364307));
#49062=CARTESIAN_POINT('Ctrl Pts',(1.78053424961026,3.06304474292021,-2.10343075971204));
#49063=CARTESIAN_POINT('Ctrl Pts',(1.90464785652295,2.98375084516111,-2.10839721578101));
#49064=CARTESIAN_POINT('Ctrl Pts',(2.06742042360426,2.87975844970031,-2.11491062574267));
#49065=CARTESIAN_POINT('Ctrl Pts',(2.22171376607907,2.76250122118534,-2.12142403570433));
#49066=CARTESIAN_POINT('Ctrl Pts',(2.36547392639545,2.63349262599518,-2.12793744566599));
#49067=CARTESIAN_POINT('Ctrl Pts',(2.45083123681511,2.55689402814848,-2.13180476992859));
#49068=CARTESIAN_POINT('Ctrl Pts',(2.53247769695781,2.47614836598736,-2.13567209419119));
#49069=CARTESIAN_POINT('Ctrl Pts',(2.609961772308,2.3915893349595,-2.1395394184538));
#49070=CARTESIAN_POINT('Ctrl Pts',(2.66297762765571,2.3337326807108,-2.14218550415286));
#49071=CARTESIAN_POINT('Ctrl Pts',(2.71404492982089,2.27409090047738,-2.14483158985192));
#49072=CARTESIAN_POINT('Ctrl Pts',(2.7630696354151,2.21281727982083,-2.14747767555098));
#49073=CARTESIAN_POINT('Ctrl Pts',(2.88374524539246,2.06199064132035,-2.15399108551267));
#49074=CARTESIAN_POINT('Ctrl Pts',(2.99204550459216,1.90128017903614,-2.16050449547437));
#49075=CARTESIAN_POINT('Ctrl Pts',(3.08664143368824,1.73287520944786,-2.16701790543607));
#49076=CARTESIAN_POINT('Ctrl Pts',(3.17650752923906,1.57289055436952,-2.17320564234583));
#49077=CARTESIAN_POINT('Ctrl Pts',(3.2540133932933,1.40594134449907,-2.17939337925558));
#49078=CARTESIAN_POINT('Ctrl Pts',(3.317978242801,1.23394504751905,-2.18558111616548));
#49079=CARTESIAN_POINT('Ctrl Pts',(3.32134484161676,1.22489253611342,-2.18590678921737));
#49080=CARTESIAN_POINT('Ctrl Pts',(3.32467393213607,1.21582604517722,-2.18623246226927));
#49081=CARTESIAN_POINT('Ctrl Pts',(3.32796545991406,1.20674589826919,-2.18655813532116));
#49082=CARTESIAN_POINT('Ctrl Pts',(3.39379549925573,1.02514438416957,-2.19307154528297));
#49083=CARTESIAN_POINT('Ctrl Pts',(3.4445898638602,0.838110253654046,-2.19958495524494));
#49084=CARTESIAN_POINT('Ctrl Pts',(3.47993533170847,0.648217911398604,-2.20609836520674));
#49085=CARTESIAN_POINT('Ctrl Pts',(3.51528079955726,0.458325569140407,-2.21261177516864));
#49086=CARTESIAN_POINT('Ctrl Pts',(3.53518366555639,0.265551810365206,-2.21912518513037));
#49087=CARTESIAN_POINT('Ctrl Pts',(3.53921587207989,0.0724312289064312,
-2.22563859509208));
#49088=CARTESIAN_POINT('Ctrl Pts',(3.5404507477039,0.0132874580830817,-2.22763334688469));
#49089=CARTESIAN_POINT('Ctrl Pts',(3.54019686595504,-0.0458877048812477,
-2.22962809867729));
#49090=CARTESIAN_POINT('Ctrl Pts',(3.53844190482233,-0.105018504061302,
-2.2316228504699));
#49091=CARTESIAN_POINT('Ctrl Pts',(3.53446643805599,-0.238965930375457,
-2.2361415086389));
#49092=CARTESIAN_POINT('Ctrl Pts',(3.52278756542149,-0.372685587266579,
-2.24066016680791));
#49093=CARTESIAN_POINT('Ctrl Pts',(3.50360264434659,-0.505307275679988,
-2.24517882497692));
#49094=CARTESIAN_POINT('Ctrl Pts',(3.47594858170895,-0.69647451917164,-2.25169223493864));
#49095=CARTESIAN_POINT('Ctrl Pts',(3.43270056047567,-0.885379751350099,
-2.25820564490037));
#49096=CARTESIAN_POINT('Ctrl Pts',(3.37442090167997,-1.06953540954889,-2.26471905486209));
#49097=CARTESIAN_POINT('Ctrl Pts',(3.33581079605796,-1.19153800120563,-2.26903417014895));
#49098=CARTESIAN_POINT('Ctrl Pts',(3.29059905133193,-1.31146265306598,-2.2733492854358));
#49099=CARTESIAN_POINT('Ctrl Pts',(3.23895722418867,-1.42855034908728,-2.27766440072265));
#49100=CARTESIAN_POINT('Ctrl Pts',(3.21264878372798,-1.48819956852543,-2.27986269539743));
#49101=CARTESIAN_POINT('Ctrl Pts',(3.18467168469657,-1.54711255044106,-2.28206099007222));
#49102=CARTESIAN_POINT('Ctrl Pts',(3.15508456246594,-1.60520476755959,-2.284259284747));
#49103=CARTESIAN_POINT('Ctrl Pts',(3.06741976534675,-1.77732838229316,-2.29077269470864));
#49104=CARTESIAN_POINT('Ctrl Pts',(2.96562690748143,-1.94223957070431,-2.29728610467027));
#49105=CARTESIAN_POINT('Ctrl Pts',(2.85118122343503,-2.0978372735158,-2.30379951463191));
#49106=CARTESIAN_POINT('Ctrl Pts',(2.73673553938697,-2.25343497632954,-2.31031292459364));
#49107=CARTESIAN_POINT('Ctrl Pts',(2.60962088951851,-2.39973705663602,-2.31682633455537));
#49108=CARTESIAN_POINT('Ctrl Pts',(2.47132239430563,-2.53459348728904,-2.32333974451709));
#49109=CARTESIAN_POINT('Ctrl Pts',(2.4687292831959,-2.53712205933177,-2.32346187162851));
#49110=CARTESIAN_POINT('Ctrl Pts',(2.46613224843455,-2.5396465996386,-2.32358399873993));
#49111=CARTESIAN_POINT('Ctrl Pts',(2.463531299937,-2.54216709408167,-2.32370612585135));
#49112=CARTESIAN_POINT('Ctrl Pts',(2.32741576151579,-2.67407222735452,-2.33009740870157));
#49113=CARTESIAN_POINT('Ctrl Pts',(2.18058121321383,-2.79489605595183,-2.33648869155178));
#49114=CARTESIAN_POINT('Ctrl Pts',(2.02510726029512,-2.90329545916035,-2.342879974402));
#49115=CARTESIAN_POINT('Ctrl Pts',(1.8666624507869,-3.01376620020569,-2.34939338436364));
#49116=CARTESIAN_POINT('Ctrl Pts',(1.69922697758555,-3.11134926906942,-2.35590679432527));
#49117=CARTESIAN_POINT('Ctrl Pts',(1.52494467780377,-3.19463871795646,-2.36242020428691));
#49118=CARTESIAN_POINT('Ctrl Pts',(1.45958838442203,-3.22587246724644,-2.36486274912882));
#49119=CARTESIAN_POINT('Ctrl Pts',(1.39326974838671,-3.25509547106922,-2.36730529397073));
#49120=CARTESIAN_POINT('Ctrl Pts',(1.32610734069228,-3.28223084516667,-2.36974783881264));
#49121=CARTESIAN_POINT('Ctrl Pts',(1.21417117552754,-3.32745599151041,-2.37381870393245));
#49122=CARTESIAN_POINT('Ctrl Pts',(1.09989117051022,-3.3668818964363,-2.37788956905227));
#49123=CARTESIAN_POINT('Ctrl Pts',(0.983909678540035,-3.40038425065325,
-2.38196043417208));
#49124=CARTESIAN_POINT('Ctrl Pts',(0.7983385571865,-3.45398822948136,-2.3884738441337));
#49125=CARTESIAN_POINT('Ctrl Pts',(0.608398132847113,-3.49243632959352,
-2.3949872540953));
#49126=CARTESIAN_POINT('Ctrl Pts',(0.416593020999056,-3.51524584577225,
-2.40150066405692));
#49127=CARTESIAN_POINT('Ctrl Pts',(0.276336123570181,-3.53192523424243,
-2.40626357503514));
#49128=CARTESIAN_POINT('Ctrl Pts',(0.135071043364323,-3.54024113541699,
-2.41102648601336));
#49129=CARTESIAN_POINT('Ctrl Pts',(-0.00617846241521584,-3.539994608273,
-2.41578939699159));
#49130=CARTESIAN_POINT('Ctrl Pts',(-0.0580914873316,-3.53990400286027,-2.41753989597509));
#49131=CARTESIAN_POINT('Ctrl Pts',(-0.110002393163228,-3.53865692860149,
-2.41929039495859));
#49132=CARTESIAN_POINT('Ctrl Pts',(-0.161860370969656,-3.53626328586113,
-2.4210408939421));
#49133=CARTESIAN_POINT('Ctrl Pts',(-0.354818077553921,-3.52735681026954,
-2.42755430390373));
#49134=CARTESIAN_POINT('Ctrl Pts',(-0.547027243948119,-3.50257873337156,
-2.43406771386537));
#49135=CARTESIAN_POINT('Ctrl Pts',(-0.73596390415267,-3.46243784695285,
-2.440581123827));
#49136=CARTESIAN_POINT('Ctrl Pts',(-0.924900564357221,-3.42229696053415,
-2.44709453378864));
#49137=CARTESIAN_POINT('Ctrl Pts',(-1.11058788540349,-3.36678693880149,
-2.45360794375027));
#49138=CARTESIAN_POINT('Ctrl Pts',(-1.29047199844307,-3.29639980380972,
-2.46012135371191));
#49139=CARTESIAN_POINT('Ctrl Pts',(-1.30621201758925,-3.29024086718272,
-2.46069128285001));
#49140=CARTESIAN_POINT('Ctrl Pts',(-1.32190738964502,-3.28396810707535,
-2.46126121198811));
#49141=CARTESIAN_POINT('Ctrl Pts',(-1.33755638533705,-3.27758187022733,
-2.46183114112621));
#49142=CARTESIAN_POINT('Ctrl Pts',(-1.5007512451651,-3.21098328155419,-2.46777462194984));
#49143=CARTESIAN_POINT('Ctrl Pts',(-1.65890194128621,-3.13204291772606,
-2.47371810277347));
#49144=CARTESIAN_POINT('Ctrl Pts',(-1.81033770201859,-3.04186253180114,
-2.47966158359708));
#49145=CARTESIAN_POINT('Ctrl Pts',(-1.97629486109295,-2.94303461572669,
-2.4861749935587));
#49146=CARTESIAN_POINT('Ctrl Pts',(-2.13420984660948,-2.83069876261338,
-2.4926884035203));
#49147=CARTESIAN_POINT('Ctrl Pts',(-2.28193901730622,-2.70625136015001,
-2.49920181348192));
#49148=CARTESIAN_POINT('Ctrl Pts',(-2.34749402191622,-2.65102766936699,
-2.50209214731408));
#49149=CARTESIAN_POINT('Ctrl Pts',(-2.41104305301027,-2.593418363129,-2.50498248114623));
#49150=CARTESIAN_POINT('Ctrl Pts',(-2.47239011042567,-2.53355227731117,
-2.50787281497841));
#49151=CARTESIAN_POINT('Ctrl Pts',(-2.54928955258278,-2.45850925491567,
-2.51149589110799));
#49152=CARTESIAN_POINT('Ctrl Pts',(-2.62272889170948,-2.37992008874756,
-2.5151189672376));
#49153=CARTESIAN_POINT('Ctrl Pts',(-2.69244525650513,-2.29816470206638,
-2.51874204336726));
#49154=CARTESIAN_POINT('Ctrl Pts',(-2.81777832948228,-2.15118839492212,
-2.52525545332906));
#49155=CARTESIAN_POINT('Ctrl Pts',(-2.93108910381199,-1.9939736040557,-2.53176886329103));
#49156=CARTESIAN_POINT('Ctrl Pts',(-3.03092976256236,-1.82862245583661,
-2.53828227325283));
#49157=CARTESIAN_POINT('Ctrl Pts',(-3.11080203430125,-1.69634196001263,
-2.54349298456952));
#49158=CARTESIAN_POINT('Ctrl Pts',(-3.18205838653695,-1.55884051299148,
-2.5487036958861));
#49159=CARTESIAN_POINT('Ctrl Pts',(-3.2439240626505,-1.41723557525112,-2.55391440720265));
#49160=CARTESIAN_POINT('Ctrl Pts',(-3.25939072882222,-1.38183377512727,
-2.55521710584774));
#49161=CARTESIAN_POINT('Ctrl Pts',(-3.27427051474745,-1.34617553341453,
-2.55651980449282));
#49162=CARTESIAN_POINT('Ctrl Pts',(-3.28855875162332,-1.31028157168752,
-2.55782250313791));
#49163=CARTESIAN_POINT('Ctrl Pts',(-3.35999902275125,-1.13081405726206,
-2.56433591309964));
#49164=CARTESIAN_POINT('Ctrl Pts',(-3.41664396289098,-0.9454748130943,-2.57084932306137));
#49165=CARTESIAN_POINT('Ctrl Pts',(-3.45794355355989,-0.756788175000208,
-2.57736273302309));
#49166=CARTESIAN_POINT('Ctrl Pts',(-3.49924314422819,-0.568101536908852,
-2.58387614298473));
#49167=CARTESIAN_POINT('Ctrl Pts',(-3.52520219045534,-0.376044002607325,
-2.59038955294637));
#49168=CARTESIAN_POINT('Ctrl Pts',(-3.53524656047543,-0.183140996775934,
-2.596902962908));
#49169=CARTESIAN_POINT('Ctrl Pts',(-3.5368160129307,-0.152999524933752,
-2.5979206959501));
#49170=CARTESIAN_POINT('Ctrl Pts',(-3.53799685819296,-0.122838037839204,
-2.5989384289922));
#49171=CARTESIAN_POINT('Ctrl Pts',(-3.53878693041333,-0.0926663970097817,
-2.5999561620343));
#49172=CARTESIAN_POINT('Ctrl Pts',(-3.54305325712833,0.070258047094353,
-2.60545183895384));
#49173=CARTESIAN_POINT('Ctrl Pts',(-3.5359238682156,0.233478412978716,-2.61094751587337));
#49174=CARTESIAN_POINT('Ctrl Pts',(-3.51766563120604,0.395426864888091,
-2.61644319279291));
#49175=CARTESIAN_POINT('Ctrl Pts',(-3.4960261890476,0.587366215653757,-2.62295660275464));
#49176=CARTESIAN_POINT('Ctrl Pts',(-3.4587560775586,0.777542371198995,-2.62947001271637));
#49177=CARTESIAN_POINT('Ctrl Pts',(-3.40627360153106,0.963435501424812,
-2.63598342267808));
#49178=CARTESIAN_POINT('Ctrl Pts',(-3.3793763475951,1.05870567743576,-2.63932154341837));
#49179=CARTESIAN_POINT('Ctrl Pts',(-3.34848198131686,1.15285246353695,-2.64265966415865));
#49180=CARTESIAN_POINT('Ctrl Pts',(-3.313650756516,1.24551943535272,-2.64599778489894));
#49181=CARTESIAN_POINT('Ctrl Pts',(-3.28051857787996,1.33366616810227,-2.64917307412027));
#49182=CARTESIAN_POINT('Ctrl Pts',(-3.24382428725794,1.42047390410623,-2.65234836334159));
#49183=CARTESIAN_POINT('Ctrl Pts',(-3.20373088991644,1.50567764427224,-2.65552365256292));
#49184=CARTESIAN_POINT('Ctrl Pts',(-3.12148807187998,1.68045444452225,-2.66203706252464));
#49185=CARTESIAN_POINT('Ctrl Pts',(-3.02494376338762,1.84848829715205,-2.66855047248637));
#49186=CARTESIAN_POINT('Ctrl Pts',(-2.91544434228993,2.0076070020078,-2.67506388244809));
#49187=CARTESIAN_POINT('Ctrl Pts',(-2.82031689157503,2.14584112783464,-2.68072239715903));
#49188=CARTESIAN_POINT('Ctrl Pts',(-2.7153993256723,2.27735955487245,-2.68638091186997));
#49189=CARTESIAN_POINT('Ctrl Pts',(-2.601597666831,2.400685231333,-2.69203942658091));
#49190=CARTESIAN_POINT('Ctrl Pts',(-2.58440437448575,2.41931742378652,-2.6928943218316));
#49191=CARTESIAN_POINT('Ctrl Pts',(-2.5670083197053,2.43776262618973,-2.6937492170823));
#49192=CARTESIAN_POINT('Ctrl Pts',(-2.54941430867889,2.4560172922504,-2.694604112333));
#49193=CARTESIAN_POINT('Ctrl Pts',(-2.41536629918196,2.59509880389615,-2.70111752229464));
#49194=CARTESIAN_POINT('Ctrl Pts',(-2.26984684389257,2.72310064051428,-2.70763093225627));
#49195=CARTESIAN_POINT('Ctrl Pts',(-2.11495442977927,2.83849845023986,-2.71414434221791));
#49196=CARTESIAN_POINT('Ctrl Pts',(-1.96006201566371,2.95389625996712,-2.72065775217964));
#49197=CARTESIAN_POINT('Ctrl Pts',(-1.79577783391285,3.05670494108783,-2.72717116214137));
#49198=CARTESIAN_POINT('Ctrl Pts',(-1.62417584367481,3.14538952674968,-2.73368457210309));
#49199=CARTESIAN_POINT('Ctrl Pts',(-1.5855649121518,3.16534380851171,-2.73515010770478));
#49200=CARTESIAN_POINT('Ctrl Pts',(-1.54658437024401,3.18458250627967,-2.73661564330646));
#49201=CARTESIAN_POINT('Ctrl Pts',(-1.50725869214041,3.20308776572967,-2.73808117890815));
#49202=CARTESIAN_POINT('Ctrl Pts',(-1.37180576833643,3.26682707345756,-2.7431290532681));
#49203=CARTESIAN_POINT('Ctrl Pts',(-1.23225792299338,3.32186406534164,-2.74817692762805));
#49204=CARTESIAN_POINT('Ctrl Pts',(-1.08981621794126,3.36789750679959,-2.753224801988));
#49205=CARTESIAN_POINT('Ctrl Pts',(-0.90601980097821,3.42729571182215,-2.75973821194964));
#49206=CARTESIAN_POINT('Ctrl Pts',(-0.717386036659192,3.47171455680863,
-2.76625162191127));
#49207=CARTESIAN_POINT('Ctrl Pts',(-0.526388358542247,3.50052703129853,
-2.77276503187291));
#49208=CARTESIAN_POINT('Ctrl Pts',(-0.415371292863036,3.51727423160149,
-2.77655093999826));
#49209=CARTESIAN_POINT('Ctrl Pts',(-0.303551189065533,3.52874803372401,
-2.78033684812361));
#49210=CARTESIAN_POINT('Ctrl Pts',(-0.191438997966164,3.5348198129545,-2.78412275624896));
#49211=CARTESIAN_POINT('Ctrl Pts',(-0.110669418520737,3.53919413701438,
-2.78685025808534));
#49212=CARTESIAN_POINT('Ctrl Pts',(-0.0297482761444177,3.54076478310675,
-2.78957775992171));
#49213=CARTESIAN_POINT('Ctrl Pts',(0.0511292772991568,3.53955874091815,
-2.79230526175808));
#49214=CARTESIAN_POINT('Ctrl Pts',(0.244268895115812,3.53667865222285,-2.7988186717197));
#49215=CARTESIAN_POINT('Ctrl Pts',(0.437158914978994,3.51796689039577,-2.8053320816813));
#49216=CARTESIAN_POINT('Ctrl Pts',(0.627264950562928,3.48378569015157,-2.81184549164292));
#49217=CARTESIAN_POINT('Ctrl Pts',(0.805489255928714,3.45174083344104,-2.81795180995316));
#49218=CARTESIAN_POINT('Ctrl Pts',(0.981286782970914,3.40609307546753,-2.8240581282634));
#49219=CARTESIAN_POINT('Ctrl Pts',(1.15251126677808,3.3471357576215,-2.83016444657365));
#49220=CARTESIAN_POINT('Ctrl Pts',(1.16392633791351,3.34320523342191,-2.83057153822513));
#49221=CARTESIAN_POINT('Ctrl Pts',(1.1753210843407,3.33921555889236,-2.83097862987661));
#49222=CARTESIAN_POINT('Ctrl Pts',(1.18669494970798,3.33516705334005,-2.83138572152809));
#49223=CARTESIAN_POINT('Ctrl Pts',(1.36867521807276,3.27039152601533,-2.83789913148973));
#49224=CARTESIAN_POINT('Ctrl Pts',(1.54528068641558,3.19056603871398,-2.84441254145137));
#49225=CARTESIAN_POINT('Ctrl Pts',(1.7142617758279,3.09700442209031,-2.850925951413));
#49226=CARTESIAN_POINT('Ctrl Pts',(1.88324286524021,3.00344280546664,-2.85743936137464));
#49227=CARTESIAN_POINT('Ctrl Pts',(2.04462139391706,2.89613498241052,-2.86395277133627));
#49228=CARTESIAN_POINT('Ctrl Pts',(2.19616581212668,2.77635948507303,-2.87046618129807));
#49229=CARTESIAN_POINT('Ctrl Pts',(2.24068245442155,2.74117506169632,-2.87237951565123));
#49230=CARTESIAN_POINT('Ctrl Pts',(2.28434948110076,2.70491536505777,-2.8742928500044));
#49231=CARTESIAN_POINT('Ctrl Pts',(2.32710837011083,2.667614408748,-2.87620618435757));
#49232=CARTESIAN_POINT('Ctrl Pts',(2.42991012144495,2.57793472520482,-2.88080625996636));
#49233=CARTESIAN_POINT('Ctrl Pts',(2.52746203568147,2.4822357996935,-2.88540633557519));
#49234=CARTESIAN_POINT('Ctrl Pts',(2.61918727517748,2.38126086742591,-2.89000641118393));
#49235=CARTESIAN_POINT('Ctrl Pts',(2.74906429014366,2.2382868848952,-2.89651982114573));
#49236=CARTESIAN_POINT('Ctrl Pts',(2.8672760376804,2.08472396627836,-2.90303323110736));
#49237=CARTESIAN_POINT('Ctrl Pts',(2.97225682514692,1.92258536488254,-2.909546641069));
#49238=CARTESIAN_POINT('Ctrl Pts',(3.04049404589932,1.8171957235688,-2.91378033948305));
#49239=CARTESIAN_POINT('Ctrl Pts',(3.10314345866287,1.70817591623019,-2.9180140378971));
#49240=CARTESIAN_POINT('Ctrl Pts',(3.15975379732033,1.59610649404042,-2.92224773631116));
#49241=CARTESIAN_POINT('Ctrl Pts',(3.19023665890577,1.53576068503121,-2.92452744785874));
#49242=CARTESIAN_POINT('Ctrl Pts',(3.21896862084254,1.47453073235579,-2.92680715940632));
#49243=CARTESIAN_POINT('Ctrl Pts',(3.24591833613534,1.41252706412557,-2.92908687095391));
#49244=CARTESIAN_POINT('Ctrl Pts',(3.32291691266136,1.23537512981941,-2.93560028091564));
#49245=CARTESIAN_POINT('Ctrl Pts',(3.38536604105094,1.05191544335807,-2.94211369087737));
#49246=CARTESIAN_POINT('Ctrl Pts',(3.43257863439251,0.864620338177981,-2.94862710083908));
#49247=CARTESIAN_POINT('Ctrl Pts',(3.47979122773339,0.677325233000614,-2.9551405108007));
#49248=CARTESIAN_POINT('Ctrl Pts',(3.51177061081401,0.486170850953884,-2.9616539207623));
#49249=CARTESIAN_POINT('Ctrl Pts',(3.52779770972739,0.293671846368202,-2.96816733072392));
#49250=CARTESIAN_POINT('Ctrl Pts',(3.54382480864101,0.101172841779726,-2.97468074068564));
#49251=CARTESIAN_POINT('Ctrl Pts',(3.54389063706576,-0.0926387220615205,
-2.98119415064737));
#49252=CARTESIAN_POINT('Ctrl Pts',(3.52829370107045,-0.285162093399601,
-2.98770756060909));
#49253=CARTESIAN_POINT('Ctrl Pts',(3.51269676507538,-0.477685464734896,
-2.99422097057073));
#49254=CARTESIAN_POINT('Ctrl Pts',(3.48143795907187,-0.668944729192209,
-3.00073438053237));
#49255=CARTESIAN_POINT('Ctrl Pts',(3.43479147403378,-0.856389724647762,
-3.007247790494));
#49256=CARTESIAN_POINT('Ctrl Pts',(3.41788200033896,-0.92433902923723,-3.00960891876165));
#49257=CARTESIAN_POINT('Ctrl Pts',(3.39895032352512,-0.991786185528306,
-3.0119700470293));
#49258=CARTESIAN_POINT('Ctrl Pts',(3.37801076294783,-1.05860440458627,-3.01433117529694));
#49259=CARTESIAN_POINT('Ctrl Pts',(3.34118643821438,-1.17611096770731,-3.01848345699093));
#49260=CARTESIAN_POINT('Ctrl Pts',(3.29815197932209,-1.29167222505131,-3.02263573868492));
#49261=CARTESIAN_POINT('Ctrl Pts',(3.24923804098228,-1.40467798594993,-3.02678802037891));
#49262=CARTESIAN_POINT('Ctrl Pts',(3.17250997753916,-1.58194265704288,-3.03330143034064));
#49263=CARTESIAN_POINT('Ctrl Pts',(3.08131256433646,-1.75293573710948,-3.03981484030237));
#49264=CARTESIAN_POINT('Ctrl Pts',(2.97686209402276,-1.91541538362641,-3.04632825026408));
#49265=CARTESIAN_POINT('Ctrl Pts',(2.90178864237797,-2.0321971257231,-3.05100974347646));
#49266=CARTESIAN_POINT('Ctrl Pts',(2.81986112148126,-2.14458818654409,-3.05569123668883));
#49267=CARTESIAN_POINT('Ctrl Pts',(2.73155102519233,-2.25171689978334,-3.06037272990121));
#49268=CARTESIAN_POINT('Ctrl Pts',(2.69699437047138,-2.2936374740968,-3.06220464665044));
#49269=CARTESIAN_POINT('Ctrl Pts',(2.66146049390564,-2.33475232045301,-3.06403656339968));
#49270=CARTESIAN_POINT('Ctrl Pts',(2.6249951611146,-2.37502361902699,-3.06586848014892));
#49271=CARTESIAN_POINT('Ctrl Pts',(2.49534207400957,-2.51820887971733,-3.07238189011064));
#49272=CARTESIAN_POINT('Ctrl Pts',(2.35392512391004,-2.65072077167275,-3.07889530007237));
#49273=CARTESIAN_POINT('Ctrl Pts',(2.20273828215036,-2.77093269463368,-3.08540871003409));
#49274=CARTESIAN_POINT('Ctrl Pts',(2.05155144039287,-2.89114461759288,-3.09192211999573));
#49275=CARTESIAN_POINT('Ctrl Pts',(1.89057497031891,-2.9990702680108,-3.09843552995737));
#49276=CARTESIAN_POINT('Ctrl Pts',(1.7218118521876,-3.09304726818777,-3.104948939919));
#49277=CARTESIAN_POINT('Ctrl Pts',(1.70915449898499,-3.10009560965795,-3.10543745027216));
#49278=CARTESIAN_POINT('Ctrl Pts',(1.69645349524291,-3.10706540362333,-3.10592596062531));
#49279=CARTESIAN_POINT('Ctrl Pts',(1.68370970010857,-3.11395594794783,-3.10641447097847));
#49280=CARTESIAN_POINT('Ctrl Pts',(1.52653782888907,-3.19893846169562,-3.11243937058695));
#49281=CARTESIAN_POINT('Ctrl Pts',(1.36285678345318,-3.2718654745696,-3.11846427019543));
#49282=CARTESIAN_POINT('Ctrl Pts',(1.19465624061227,-3.33212144593867,-3.12448916980391));
#49283=CARTESIAN_POINT('Ctrl Pts',(1.01281767690137,-3.39726308640959,-3.13100257976564));
#49284=CARTESIAN_POINT('Ctrl Pts',(0.825675827052175,-3.44760704052864,
-3.13751598972737));
#49285=CARTESIAN_POINT('Ctrl Pts',(0.635671099317594,-3.48238259226642,
-3.1440293996891));
#49286=CARTESIAN_POINT('Ctrl Pts',(0.553731273711291,-3.49737960143946,
-3.14683831756567));
#49287=CARTESIAN_POINT('Ctrl Pts',(0.471258885802527,-3.50948064073937,
-3.14964723544223));
#49288=CARTESIAN_POINT('Ctrl Pts',(0.38845946126229,-3.51862178231117,-3.15245615331881));
#49289=CARTESIAN_POINT('Ctrl Pts',(0.279260892156459,-3.53067741657646,
-3.15616064540387));
#49290=CARTESIAN_POINT('Ctrl Pts',(0.169493539234521,-3.53758465049955,
-3.15986513748894));
#49291=CARTESIAN_POINT('Ctrl Pts',(0.059649471939911,-3.53938415619341,
-3.163569629574));
#49292=CARTESIAN_POINT('Ctrl Pts',(-0.133483466588335,-3.54254813064478,
-3.17008303953564));
#49293=CARTESIAN_POINT('Ctrl Pts',(-0.326865118477281,-3.52992630187154,
-3.17659644949727));
#49294=CARTESIAN_POINT('Ctrl Pts',(-0.517952514192366,-3.50173373138306,
-3.18310985945891));
#49295=CARTESIAN_POINT('Ctrl Pts',(-0.668433322988736,-3.47953215815382,
-3.18823915223817));
#49296=CARTESIAN_POINT('Ctrl Pts',(-0.817504437674782,-3.44766956351041,
-3.19336844501743));
#49297=CARTESIAN_POINT('Ctrl Pts',(-0.963872074523706,-3.4062516970935,
-3.19849773779676));
#49298=CARTESIAN_POINT('Ctrl Pts',(-1.00336874001705,-3.39507526731343,
-3.19988185497925));
#49299=CARTESIAN_POINT('Ctrl Pts',(-1.04266855713235,-3.38320312817922,
-3.20126597216175));
#49300=CARTESIAN_POINT('Ctrl Pts',(-1.0817487466423,-3.37064673995017,-3.20265008934425));
#49301=CARTESIAN_POINT('Ctrl Pts',(-1.26565318687387,-3.31155860405448,
-3.20916349930603));
#49302=CARTESIAN_POINT('Ctrl Pts',(-1.4446743658271,-3.23732575217221,-3.21567690926797));
#49303=CARTESIAN_POINT('Ctrl Pts',(-1.61651402611654,-3.14912462305492,
-3.22219031922975));
#49304=CARTESIAN_POINT('Ctrl Pts',(-1.78835368640846,-3.06092349393635,
-3.22870372919164));
#49305=CARTESIAN_POINT('Ctrl Pts',(-1.95303292882817,-2.95874267186129,
-3.23521713915337));
#49306=CARTESIAN_POINT('Ctrl Pts',(-2.10823418017326,-2.84374236629767,
-3.2417305491151));
#49307=CARTESIAN_POINT('Ctrl Pts',(-2.13054463355673,-2.8272108697142,-3.24266686327532));
#49308=CARTESIAN_POINT('Ctrl Pts',(-2.15265877543496,-2.81041477835907,
-3.24360317743554));
#49309=CARTESIAN_POINT('Ctrl Pts',(-2.17456960835048,-2.79335766031483,
-3.24453949159576));
#49310=CARTESIAN_POINT('Ctrl Pts',(-2.30508009238466,-2.69175802050364,
-3.25011658739717));
#49311=CARTESIAN_POINT('Ctrl Pts',(-2.42837651672354,-2.58089661856788,
-3.25569368319859));
#49312=CARTESIAN_POINT('Ctrl Pts',(-2.5433709048767,-2.46202800977271,-3.261270779));
#49313=CARTESIAN_POINT('Ctrl Pts',(-2.67767119664131,-2.3232030714498,-3.26778418896164));
#49314=CARTESIAN_POINT('Ctrl Pts',(-2.80066707596171,-2.17344287527037,
-3.27429759892327));
#49315=CARTESIAN_POINT('Ctrl Pts',(-2.91067619386607,-2.01467029405205,
-3.28081100888491));
#49316=CARTESIAN_POINT('Ctrl Pts',(-2.96568075281904,-1.93528400344175,
-3.28406771386577));
#49317=CARTESIAN_POINT('Ctrl Pts',(-3.01743874035383,-1.85364279298029,
-3.28732441884663));
#49318=CARTESIAN_POINT('Ctrl Pts',(-3.06572992939683,-1.76999999999985,
-3.2905811238275));
#49319=CARTESIAN_POINT('Ctrl Pts',(-3.11402111843984,-1.6863572070194,-3.29383782880836));
#49320=CARTESIAN_POINT('Ctrl Pts',(-3.15884548692774,-1.60071286973475,
-3.29709453378923));
#49321=CARTESIAN_POINT('Ctrl Pts',(-3.20009375183195,-1.51338437905234,
-3.30035123877009));
#49322=CARTESIAN_POINT('Ctrl Pts',(-3.28259028163917,-1.33872739769007,
-3.30686464873173));
#49323=CARTESIAN_POINT('Ctrl Pts',(-3.350788476346,-1.15732974354807,-3.31337805869336));
#49324=CARTESIAN_POINT('Ctrl Pts',(-3.40386425373005,-0.971609809982892,
-3.319891468655));
#49325=CARTESIAN_POINT('Ctrl Pts',(-3.44931029458254,-0.812587444152017,
-3.32546856445642));
#49326=CARTESIAN_POINT('Ctrl Pts',(-3.48367087278858,-0.650378907510944,
-3.33104566025783));
#49327=CARTESIAN_POINT('Ctrl Pts',(-3.50640349986333,-0.486553692971483,
-3.33662275605925));
#49328=CARTESIAN_POINT('Ctrl Pts',(-3.51021998094721,-0.45904979602653,
-3.33755907021947));
#49329=CARTESIAN_POINT('Ctrl Pts',(-3.51370875180592,-0.431500341699595,
-3.33849538437969));
#49330=CARTESIAN_POINT('Ctrl Pts',(-3.51687022111804,-0.4039131740079,-3.33943169853991));
#49331=CARTESIAN_POINT('Ctrl Pts',(-3.53886278150659,-0.21200479486206,
-3.34594510850164));
#49332=CARTESIAN_POINT('Ctrl Pts',(-3.54501434799336,-0.018297976412778,
-3.35245851846337));
#49333=CARTESIAN_POINT('Ctrl Pts',(-3.53547893630661,0.174620099336988,
-3.35897192842508));
#49334=CARTESIAN_POINT('Ctrl Pts',(-3.52594352461999,0.367538175083959,
-3.3654853383867));
#49335=CARTESIAN_POINT('Ctrl Pts',(-3.50072047066892,0.559691489813732,
-3.3719987483483));
#49336=CARTESIAN_POINT('Ctrl Pts',(-3.45994007730116,0.748501474870884,
-3.37851215830992));
#49337=CARTESIAN_POINT('Ctrl Pts',(-3.45127413373233,0.788624105885788,
-3.37989627549239));
#49338=CARTESIAN_POINT('Ctrl Pts',(-3.44190579926218,0.828594815438887,
-3.38128039267486));
#49339=CARTESIAN_POINT('Ctrl Pts',(-3.43183653862866,0.868388146010993,
-3.38266450985732));
#49340=CARTESIAN_POINT('Ctrl Pts',(-3.39452164469186,1.01585517102254,-3.38779380263658));
#49341=CARTESIAN_POINT('Ctrl Pts',(-3.34757990374054,1.16088584063295,-3.39292309541584));
#49342=CARTESIAN_POINT('Ctrl Pts',(-3.2915666257629,1.30230683044729,-3.3980523881951));
#49343=CARTESIAN_POINT('Ctrl Pts',(-3.22043841014641,1.48188965472389,-3.40456579815673));
#49344=CARTESIAN_POINT('Ctrl Pts',(-3.13467840856183,1.65567399227211,-3.41107920811837));
#49345=CARTESIAN_POINT('Ctrl Pts',(-3.03537185704593,1.82135003611944,-3.41759261808));
#49346=CARTESIAN_POINT('Ctrl Pts',(-2.97889140575354,1.91557803600459,-3.42129711016506));
#49347=CARTESIAN_POINT('Ctrl Pts',(-2.91802588924534,2.00718573517956,-3.42500160225013));
#49348=CARTESIAN_POINT('Ctrl Pts',(-2.85298611916,2.09572665294942,-3.42870609433519));
#49349=CARTESIAN_POINT('Ctrl Pts',(-2.80366994606909,2.16286248723414,-3.43151501221176));
#49350=CARTESIAN_POINT('Ctrl Pts',(-2.75195394466874,2.228235150624,-3.43432393008833));
#49351=CARTESIAN_POINT('Ctrl Pts',(-2.6979962409409,2.29169861659424,-3.43713284796491));
#49352=CARTESIAN_POINT('Ctrl Pts',(-2.57287736583807,2.43885976178261,-3.44364625792664));
#49353=CARTESIAN_POINT('Ctrl Pts',(-2.43570729771941,2.57575738080365,-3.45015966788836));
#49354=CARTESIAN_POINT('Ctrl Pts',(-2.2883737003719,2.70066337612947,-3.45667307785009));
#49355=CARTESIAN_POINT('Ctrl Pts',(-2.15209022701611,2.81620133347544,-3.46269797745857));
#49356=CARTESIAN_POINT('Ctrl Pts',(-2.00709305852713,2.92148977050388,-3.46872287706705));
#49357=CARTESIAN_POINT('Ctrl Pts',(-1.85491010713434,3.01511334686633,-3.47474777667553));
#49358=CARTESIAN_POINT('Ctrl Pts',(-1.84257082313618,3.02270452503107,-3.47523628702869));
#49359=CARTESIAN_POINT('Ctrl Pts',(-1.83018430263193,3.03021901994261,-3.47572479738184));
#49360=CARTESIAN_POINT('Ctrl Pts',(-1.81775158326284,3.03765643862568,-3.476213307735));
#49361=CARTESIAN_POINT('Ctrl Pts',(-1.65198355467242,3.13682108606072,-3.48272671769664));
#49362=CARTESIAN_POINT('Ctrl Pts',(-1.47802896465355,3.22226797334726,-3.48924012765827));
#49363=CARTESIAN_POINT('Ctrl Pts',(-1.2983289646543,3.29309365754754,-3.49575353761991));
#49364=CARTESIAN_POINT('Ctrl Pts',(-1.11862896465245,3.36391934174885,-3.50226694758164));
#49365=CARTESIAN_POINT('Ctrl Pts',(-0.933161824865596,3.42013406708304,
-3.50878035754337));
#49366=CARTESIAN_POINT('Ctrl Pts',(-0.744333208107735,3.46082430384987,
-3.51529376750508));
#49367=CARTESIAN_POINT('Ctrl Pts',(-0.691224574103849,3.47226855911735,
-3.51712568425432));
#49368=CARTESIAN_POINT('Ctrl Pts',(-0.637851134403885,3.48248437574009,
-3.51895760100355));
#49369=CARTESIAN_POINT('Ctrl Pts',(-0.58426852474683,3.4914510294415,-3.52078951775279));
#49370=CARTESIAN_POINT('Ctrl Pts',(-0.447337289462379,3.51436545961875,
-3.52547101096518));
#49371=CARTESIAN_POINT('Ctrl Pts',(-0.309040015184776,3.5291212435739,-3.53015250417759));
#49372=CARTESIAN_POINT('Ctrl Pts',(-0.17036733400844,3.53574588879975,-3.53483399739009));
#49373=CARTESIAN_POINT('Ctrl Pts',(0.0225694026298665,3.5449628262702,-3.54134740735197));
#49374=CARTESIAN_POINT('Ctrl Pts',(0.216252460440131,3.5384455628299,-3.54786081731403));
#49375=CARTESIAN_POINT('Ctrl Pts',(0.408132200521637,3.51626167940836,-3.55437422727593));
#49376=CARTESIAN_POINT('Ctrl Pts',(0.530455029403651,3.50211951216048,-3.55852650897002));
#49377=CARTESIAN_POINT('Ctrl Pts',(0.652051243402925,3.48160781812733,-3.56267879066404));
#49378=CARTESIAN_POINT('Ctrl Pts',(0.772227074543825,3.45474533726317,-3.56683107235804));
#49379=CARTESIAN_POINT('Ctrl Pts',(0.840563129972376,3.43947041913817,-3.5691922006257));
#49380=CARTESIAN_POINT('Ctrl Pts',(0.908439919140494,3.4221421540496,-3.57155332889335));
#49381=CARTESIAN_POINT('Ctrl Pts',(0.975740479931958,3.40281153553916,-3.573914457161));
#49382=CARTESIAN_POINT('Ctrl Pts',(1.16139585032783,3.34948607885153,-3.58042786712264));
#49383=CARTESIAN_POINT('Ctrl Pts',(1.34266063505881,3.28092736671375,-3.58694127708427));
#49384=CARTESIAN_POINT('Ctrl Pts',(1.51718923345482,3.19817302383904,-3.59345468704591));
#49385=CARTESIAN_POINT('Ctrl Pts',(1.69171783185335,3.11541868096314,-3.59996809700764));
#49386=CARTESIAN_POINT('Ctrl Pts',(1.85953065547441,3.01845588995455,-3.60648150696937));
#49387=CARTESIAN_POINT('Ctrl Pts',(2.0182261341945,2.90832651285219,-3.61299491693108));
#49388=CARTESIAN_POINT('Ctrl Pts',(2.1769216129123,2.79819713575142,-3.6195083268927));
#49389=CARTESIAN_POINT('Ctrl Pts',(2.32647647226952,2.67492498658273,-3.6260217368543));
#49390=CARTESIAN_POINT('Ctrl Pts',(2.4650724946873,2.54039012878225,-3.63253514681592));
#49391=CARTESIAN_POINT('Ctrl Pts',(2.60366851710708,2.40585527097982,-3.63904855677764));
#49392=CARTESIAN_POINT('Ctrl Pts',(2.73132470195812,2.26004289611969,-3.64556196673937));
#49393=CARTESIAN_POINT('Ctrl Pts',(2.84624348913382,2.10478420563982,-3.6520753767011));
#49394=CARTESIAN_POINT('Ctrl Pts',(2.88646538330249,2.05044323345657,-3.65435508824867));
#49395=CARTESIAN_POINT('Ctrl Pts',(2.92512609682342,1.99494564818121,-3.65663479979625));
#49396=CARTESIAN_POINT('Ctrl Pts',(2.96214566964451,1.93837381116374,-3.65891451134382));
#49397=CARTESIAN_POINT('Ctrl Pts',(3.03089546691971,1.83331310867443,-3.66314820975788));
#49398=CARTESIAN_POINT('Ctrl Pts',(3.09398468320899,1.72454722201944,-3.66738190817194));
#49399=CARTESIAN_POINT('Ctrl Pts',(3.1511361795063,1.61275723470709,-3.671615606586));
#49400=CARTESIAN_POINT('Ctrl Pts',(3.23906193351585,1.4407719051538,-3.67812901654764));
#49401=CARTESIAN_POINT('Ctrl Pts',(3.31294544834883,1.26161606945278,-3.68464242650927));
#49402=CARTESIAN_POINT('Ctrl Pts',(3.37182604181743,1.07765228385916,-3.69115583647091));
#49403=CARTESIAN_POINT('Ctrl Pts',(3.41341027855843,0.947728430153869,-3.69575591207952));
#49404=CARTESIAN_POINT('Ctrl Pts',(3.44751202204771,0.815396531481927,-3.70035598768814));
#49405=CARTESIAN_POINT('Ctrl Pts',(3.47377603053233,0.681527761501758,-3.70495606329676));
#49406=CARTESIAN_POINT('Ctrl Pts',(3.48470016177703,0.625846999226429,-3.70686939764987));
#49407=CARTESIAN_POINT('Ctrl Pts',(3.49426846685995,0.569900396495106,-3.70878273200298));
#49408=CARTESIAN_POINT('Ctrl Pts',(3.50248075017427,0.513755641688056,-3.7106960663561));
#49409=CARTESIAN_POINT('Ctrl Pts',(3.53043716451462,0.322626577048128,-3.71720947631773));
#49410=CARTESIAN_POINT('Ctrl Pts',(3.54267920096763,0.129214760060477,-3.72372288627937));
#49411=CARTESIAN_POINT('Ctrl Pts',(3.53921539307674,-0.063907964441538,
-3.730236296241));
#49412=CARTESIAN_POINT('Ctrl Pts',(3.53575158518584,-0.257030688943553,
-3.73674970620264));
#49413=CARTESIAN_POINT('Ctrl Pts',(3.51657975088695,-0.449888254626207,
-3.74326311616427));
#49414=CARTESIAN_POINT('Ctrl Pts',(3.48168686891133,-0.639875553680029,
-3.74977652612591));
#49415=CARTESIAN_POINT('Ctrl Pts',(3.47950604488335,-0.651749862803495,
-3.75018361777739));
#49416=CARTESIAN_POINT('Ctrl Pts',(3.47726383116518,-0.663612839943919,
-3.75059070942887));
#49417=CARTESIAN_POINT('Ctrl Pts',(3.4749602294045,-0.675463843633017,-3.75099780108035));
#49418=CARTESIAN_POINT('Ctrl Pts',(3.4404065224946,-0.853227255282967,-3.7571041193906));
#49419=CARTESIAN_POINT('Ctrl Pts',(3.39203987700435,-1.02829625861096,-3.76321043770085));
#49420=CARTESIAN_POINT('Ctrl Pts',(3.33067938429338,-1.19866546298495,-3.76931675601108));
#49421=CARTESIAN_POINT('Ctrl Pts',(3.26522815424471,-1.38039271933565,-3.7758301659727));
#49422=CARTESIAN_POINT('Ctrl Pts',(3.18498800540492,-1.55679625758723,-3.7823435759343));
#49423=CARTESIAN_POINT('Ctrl Pts',(3.09091242647188,-1.72550011744132,-3.78885698589592));
#49424=CARTESIAN_POINT('Ctrl Pts',(3.05151811292345,-1.79614515441368,-3.79158448773229));
#49425=CARTESIAN_POINT('Ctrl Pts',(3.00969732231895,-1.86543959636863,-3.79431198956866));
#49426=CARTESIAN_POINT('Ctrl Pts',(2.965524256836,-1.9332009419914,-3.79703949140504));
#49427=CARTESIAN_POINT('Ctrl Pts',(2.90420984622655,-2.02725705794212,-3.80082539953039));
#49428=CARTESIAN_POINT('Ctrl Pts',(2.83836319021171,-2.11835920742328,-3.80461130765574));
#49429=CARTESIAN_POINT('Ctrl Pts',(2.76835115646748,-2.20612920640356,-3.80839721578109));
#49430=CARTESIAN_POINT('Ctrl Pts',(2.64789998255489,-2.35713181047166,-3.81491062574273));
#49431=CARTESIAN_POINT('Ctrl Pts',(2.5151152522304,-2.49828401989007,-3.82142403570437));
#49432=CARTESIAN_POINT('Ctrl Pts',(2.37177668926012,-2.62775728359333,-3.827937445666));
#49433=CARTESIAN_POINT('Ctrl Pts',(2.26068970700779,-2.7280986979979,-3.83298532002595));
#49434=CARTESIAN_POINT('Ctrl Pts',(2.14325235121661,-2.82143218116641,-3.83803319438591));
#49435=CARTESIAN_POINT('Ctrl Pts',(2.02032602960248,-2.90686820033367,-3.84308106874586));
#49436=CARTESIAN_POINT('Ctrl Pts',(1.98463716576339,-2.93167260686741,-3.84454660434754));
#49437=CARTESIAN_POINT('Ctrl Pts',(1.94848569380674,-2.95581139752882,-3.84601213994922));
#49438=CARTESIAN_POINT('Ctrl Pts',(1.91189931312508,-2.97927230421048,-3.84747767555091));
#49439=CARTESIAN_POINT('Ctrl Pts',(1.7492952138987,-3.08354169426571,-3.85399108551264));
#49440=CARTESIAN_POINT('Ctrl Pts',(1.57811819344313,-3.17441162854151,-3.86050449547437));
#49441=CARTESIAN_POINT('Ctrl Pts',(1.40073455162058,-3.25085348915537,-3.8670179054361));
#49442=CARTESIAN_POINT('Ctrl Pts',(1.22335090980063,-3.32729534976811,-3.87353131539773));
#49443=CARTESIAN_POINT('Ctrl Pts',(1.03973833991381,-3.38931797648445,-3.88004472535937));
#49444=CARTESIAN_POINT('Ctrl Pts',(0.852266212883417,-3.43586620221265,
-3.88655813532117));
#49445=CARTESIAN_POINT('Ctrl Pts',(0.827660202824008,-3.44197572968566,
-3.88741303057189));
#49446=CARTESIAN_POINT('Ctrl Pts',(0.802988161574587,-3.44781855384957,
-3.88826792582262));
#49447=CARTESIAN_POINT('Ctrl Pts',(0.778255563408939,-3.4533922855685,-3.88912282107334));
#49448=CARTESIAN_POINT('Ctrl Pts',(0.614551565234618,-3.49028457488758,
-3.89478133578446));
#49449=CARTESIAN_POINT('Ctrl Pts',(0.448194483402658,-3.51538663874368,
-3.90043985049566));
#49450=CARTESIAN_POINT('Ctrl Pts',(0.280916493409238,-3.52865236474662,
-3.90609836520674));
#49451=CARTESIAN_POINT('Ctrl Pts',(0.0883659422379453,-3.54392229268905,
-3.91261177516864));
#49452=CARTESIAN_POINT('Ctrl Pts',(-0.105427797081422,-3.54351519011934,
-3.91912518513037));
#49453=CARTESIAN_POINT('Ctrl Pts',(-0.297910355108321,-3.52735115969274,
-3.92563859509208));
#49454=CARTESIAN_POINT('Ctrl Pts',(-0.39174565726025,-3.51947119023151,
-3.92881388431341));
#49455=CARTESIAN_POINT('Ctrl Pts',(-0.485270507195668,-3.50784551008206,
-3.93198917353473));
#49456=CARTESIAN_POINT('Ctrl Pts',(-0.578173906335351,-3.49246545208883,
-3.93516446275606));
#49457=CARTESIAN_POINT('Ctrl Pts',(-0.675841470420018,-3.47629669170343,
-3.93850258349635));
#49458=CARTESIAN_POINT('Ctrl Pts',(-0.772822162007415,-3.45597860468362,
-3.94184070423663));
#49459=CARTESIAN_POINT('Ctrl Pts',(-0.868777181623859,-3.43163722187875,
-3.94517882497692));
#49460=CARTESIAN_POINT('Ctrl Pts',(-1.05600659280207,-3.38414181425924,
-3.95169223493864));
#49461=CARTESIAN_POINT('Ctrl Pts',(-1.23933903044262,-3.32133059983808,
-3.95820564490036));
#49462=CARTESIAN_POINT('Ctrl Pts',(-1.41638310527089,-3.24410123108816,
-3.96471905486209));
#49463=CARTESIAN_POINT('Ctrl Pts',(-1.56576369723281,-3.17893910221207,
-3.97021473178163));
#49464=CARTESIAN_POINT('Ctrl Pts',(-1.71068137496023,-3.10350315118168,
-3.97571040870116));
#49465=CARTESIAN_POINT('Ctrl Pts',(-1.8496449190945,-3.0183461818135,-3.98120608562069));
#49466=CARTESIAN_POINT('Ctrl Pts',(-1.87537929041651,-3.00257613878509,
-3.9822238186628));
#49467=CARTESIAN_POINT('Ctrl Pts',(-1.90090948182522,-2.98647275324273,
-3.9832415517049));
#49468=CARTESIAN_POINT('Ctrl Pts',(-1.9262280359204,-2.97004283162531,-3.984259284747));
#49469=CARTESIAN_POINT('Ctrl Pts',(-2.08826475442685,-2.86489264910712,
-3.99077269470864));
#49470=CARTESIAN_POINT('Ctrl Pts',(-2.24161193500656,-2.74638268846562,
-3.99728610467027));
#49471=CARTESIAN_POINT('Ctrl Pts',(-2.38436956161414,-2.61627287473533,
-4.00379951463191));
#49472=CARTESIAN_POINT('Ctrl Pts',(-2.52712718822379,-2.48616306100314,
-4.01031292459364));
#49473=CARTESIAN_POINT('Ctrl Pts',(-2.65931321192137,-2.34443748176244,
-4.01682633455537));
#49474=CARTESIAN_POINT('Ctrl Pts',(-2.77901650300382,-2.19283463489973,
-4.0233397445171));
#49475=CARTESIAN_POINT('Ctrl Pts',(-2.80295746726397,-2.16251367792641,
-4.02464244316218));
#49476=CARTESIAN_POINT('Ctrl Pts',(-2.8263985174789,-2.13179828445587,-4.02594514180727));
#49477=CARTESIAN_POINT('Ctrl Pts',(-2.84932404264,-2.10070285857735,-4.02724784045235));
#49478=CARTESIAN_POINT('Ctrl Pts',(-2.94102467796757,-1.97632314257066,
-4.0324585517689));
#49479=CARTESIAN_POINT('Ctrl Pts',(-3.02447624802702,-1.84586260784311,
-4.03766926308545));
#49480=CARTESIAN_POINT('Ctrl Pts',(-3.09909838196629,-1.71055094354732,
-4.042879974402));
#49481=CARTESIAN_POINT('Ctrl Pts',(-3.19237634749372,-1.54141082262935,
-4.04939338436364));
#49482=CARTESIAN_POINT('Ctrl Pts',(-3.27187296306989,-1.36467341810391,
-4.05590679432527));
#49483=CARTESIAN_POINT('Ctrl Pts',(-3.33649164232266,-1.18264363939907,
-4.06242020428691));
#49484=CARTESIAN_POINT('Ctrl Pts',(-3.37243570168691,-1.08138980308597,
-4.06604328041647));
#49485=CARTESIAN_POINT('Ctrl Pts',(-3.40377624648734,-0.978494886681129,
-4.06966635654604));
#49486=CARTESIAN_POINT('Ctrl Pts',(-3.43031568918,-0.874376505038574,-4.0732894326756));
#49487=CARTESIAN_POINT('Ctrl Pts',(-3.45148771161571,-0.791315351960366,
-4.07617976650776));
#49488=CARTESIAN_POINT('Ctrl Pts',(-3.4696043187652,-0.707475623527939,
-4.07907010033992));
#49489=CARTESIAN_POINT('Ctrl Pts',(-3.48465193556905,-0.623091478798857,
-4.08196043417208));
#49490=CARTESIAN_POINT('Ctrl Pts',(-3.51856196218893,-0.432930562863846,
-4.0884738441337));
#49491=CARTESIAN_POINT('Ctrl Pts',(-3.5368901719826,-0.240004247211696,
-4.0949872540953));
#49492=CARTESIAN_POINT('Ctrl Pts',(-3.539499078369,-0.0468671734762678,
-4.10150066405692));
#49493=CARTESIAN_POINT('Ctrl Pts',(-3.5418797031369,0.129370235321772,-4.10744414488054));
#49494=CARTESIAN_POINT('Ctrl Pts',(-3.53116871553553,0.305802937702781,
-4.11338762570416));
#49495=CARTESIAN_POINT('Ctrl Pts',(-3.50724735526867,0.480433126417416,
-4.11933110652779));
#49496=CARTESIAN_POINT('Ctrl Pts',(-3.50495350076762,0.497178672654429,
-4.11990103566589));
#49497=CARTESIAN_POINT('Ctrl Pts',(-3.50253818434456,0.513907643630247,
-4.12047096480399));
#49498=CARTESIAN_POINT('Ctrl Pts',(-3.50000197035076,0.530618368380382,
-4.12104089394209));
#49499=CARTESIAN_POINT('Ctrl Pts',(-3.47101696083347,0.72159614750572,-4.12755430390373));
#49500=CARTESIAN_POINT('Ctrl Pts',(-3.42624638929545,0.910161095558849,
-4.13406771386537));
#49501=CARTESIAN_POINT('Ctrl Pts',(-3.36654108656219,1.09385548621155,-4.140581123827));
#49502=CARTESIAN_POINT('Ctrl Pts',(-3.30683578382893,1.27754987686425,-4.14709453378864));
#49503=CARTESIAN_POINT('Ctrl Pts',(-3.23218964468241,1.45639693625083,-4.15360794375027));
#49504=CARTESIAN_POINT('Ctrl Pts',(-3.14342402551079,1.62795644980454,-4.16012135371191));
#49505=CARTESIAN_POINT('Ctrl Pts',(-3.11956799202827,1.67406359734405,-4.16187185269541));
#49506=CARTESIAN_POINT('Ctrl Pts',(-3.09469253710093,1.71964329765716,-4.16362235167892));
#49507=CARTESIAN_POINT('Ctrl Pts',(-3.06881449123183,1.76464659872848,-4.16537285066242));
#49508=CARTESIAN_POINT('Ctrl Pts',(-2.99840323711153,1.88709552257745,-4.17013576164065));
#49509=CARTESIAN_POINT('Ctrl Pts',(-2.92056891533613,2.00527672011598,-4.17489867261887));
#49510=CARTESIAN_POINT('Ctrl Pts',(-2.83599569248695,2.11840306211022,-4.17966158359708));
#49511=CARTESIAN_POINT('Ctrl Pts',(-2.72033951610409,2.27310640345701,-4.1861749935587));
#49512=CARTESIAN_POINT('Ctrl Pts',(-2.59207227250994,2.4183755860845,-4.1926884035203));
#49513=CARTESIAN_POINT('Ctrl Pts',(-2.45286430442405,2.55228290197142,-4.19920181348192));
#49514=CARTESIAN_POINT('Ctrl Pts',(-2.36585966860048,2.63597464327796,-4.20327267860173));
#49515=CARTESIAN_POINT('Ctrl Pts',(-2.27457583085879,2.71523107830464,-4.20734354372155));
#49516=CARTESIAN_POINT('Ctrl Pts',(-2.17944162265286,2.78955806776767,-4.2114144088414));
#49517=CARTESIAN_POINT('Ctrl Pts',(-2.12236049549604,2.83415473196168,-4.21385695368334));
#49518=CARTESIAN_POINT('Ctrl Pts',(-2.06389331379296,2.87697685360123,-4.21629949852529));
#49519=CARTESIAN_POINT('Ctrl Pts',(-2.00416594676152,2.91796018932203,-4.21874204336726));
#49520=CARTESIAN_POINT('Ctrl Pts',(-1.84489401826728,3.02724836391952,-4.22525545332906));
#49521=CARTESIAN_POINT('Ctrl Pts',(-1.67666686505147,3.12346020277471,-4.23176886329103));
#49522=CARTESIAN_POINT('Ctrl Pts',(-1.50177399217723,3.20544206238398,-4.23828227325283));
#49523=CARTESIAN_POINT('Ctrl Pts',(-1.33016037878431,3.28588675363412,-4.24467355610321));
#49524=CARTESIAN_POINT('Ctrl Pts',(-1.15210659968557,3.35263728831822,-4.25106483895343));
#49525=CARTESIAN_POINT('Ctrl Pts',(-0.969815634171214,3.40456423580433,
-4.25745612180364));
#49526=CARTESIAN_POINT('Ctrl Pts',(-0.966332347704576,3.40555647605564,
-4.25757824891506));
#49527=CARTESIAN_POINT('Ctrl Pts',(-0.962847514285249,3.40654330398007,
-4.25770037602648));
#49528=CARTESIAN_POINT('Ctrl Pts',(-0.959361151106016,3.4075247180546,-4.25782250313791));
#49529=CARTESIAN_POINT('Ctrl Pts',(-0.773422808690397,3.45986651288758,
-4.26433591309964));
#49530=CARTESIAN_POINT('Ctrl Pts',(-0.583164165584344,3.49679998871353,
-4.27084932306137));
#49531=CARTESIAN_POINT('Ctrl Pts',(-0.391189760153187,3.51811400704572,
-4.27736273302309));
#49532=CARTESIAN_POINT('Ctrl Pts',(-0.199215354724813,3.53942802537761,
-4.28387614298473));
#49533=CARTESIAN_POINT('Ctrl Pts',(-0.00550164725985493,3.54512763200719,
-4.29038955294637));
#49534=CARTESIAN_POINT('Ctrl Pts',(0.187394174250291,3.53498576596323,-4.296902962908));
#49535=CARTESIAN_POINT('Ctrl Pts',(0.25249707115236,3.53156285688057,-4.29910125758278));
#49536=CARTESIAN_POINT('Ctrl Pts',(0.317505759619646,3.52633524440815,-4.30129955225756));
#49537=CARTESIAN_POINT('Ctrl Pts',(0.382317719199291,3.519294412462,-4.30349784693234));
#49538=CARTESIAN_POINT('Ctrl Pts',(0.509539551996122,3.50547369865527,-4.3078129622192));
#49539=CARTESIAN_POINT('Ctrl Pts',(0.636003219410405,3.48466589220727,-4.31212807750605));
#49540=CARTESIAN_POINT('Ctrl Pts',(0.760965615923843,3.45710192869036,-4.31644319279291));
#49541=CARTESIAN_POINT('Ctrl Pts',(0.949588923572606,3.41549576463196,-4.32295660275463));
#49542=CARTESIAN_POINT('Ctrl Pts',(1.13480966416368,3.35849703359421,-4.32947001271637));
#49543=CARTESIAN_POINT('Ctrl Pts',(1.31419238471769,3.28686253261049,-4.33598342267808));
#49544=CARTESIAN_POINT('Ctrl Pts',(1.43863859651384,3.23716631742433,-4.34050208084709));
#49545=CARTESIAN_POINT('Ctrl Pts',(1.56028265268397,3.18042068936791,-4.34502073901609));
#49546=CARTESIAN_POINT('Ctrl Pts',(1.67827226002658,3.1168898314225,-4.3495393971851));
#49547=CARTESIAN_POINT('Ctrl Pts',(1.73035851482898,3.08884427275604,-4.3515341489777));
#49548=CARTESIAN_POINT('Ctrl Pts',(1.78173265010367,3.05947655931791,-4.35352890077031));
#49549=CARTESIAN_POINT('Ctrl Pts',(1.83233522030034,3.02883524024529,-4.35552365256292));
#49550=CARTESIAN_POINT('Ctrl Pts',(1.99756644657541,2.92878295623329,-4.36203706252464));
#49551=CARTESIAN_POINT('Ctrl Pts',(2.15456198585818,2.81515968928226,-4.36855047248637));
#49552=CARTESIAN_POINT('Ctrl Pts',(2.30134084431348,2.68960344508741,-4.37506388244809));
#49553=CARTESIAN_POINT('Ctrl Pts',(2.44811970276666,2.56404720089438,-4.38157729240973));
#49554=CARTESIAN_POINT('Ctrl Pts',(2.58469882886557,2.42654092551998,-4.38809070237137));
#49555=CARTESIAN_POINT('Ctrl Pts',(2.70905533377063,2.2787296820682,-4.394604112333));
#49556=CARTESIAN_POINT('Ctrl Pts',(2.71527320777415,2.2713390619411,-4.39492978538489));
#49557=CARTESIAN_POINT('Ctrl Pts',(2.72146047398848,2.26392273951171,-4.39525545843678));
#49558=CARTESIAN_POINT('Ctrl Pts',(2.72761687942599,2.25648092371001,-4.39558113148867));
#49559=CARTESIAN_POINT('Ctrl Pts',(2.84458761721353,2.1150875905972,-4.40176886839842));
#49560=CARTESIAN_POINT('Ctrl Pts',(2.95041694207574,1.96449093844901,-4.40795660530816));
#49561=CARTESIAN_POINT('Ctrl Pts',(3.04403466981377,1.80667228922409,-4.4141443422179));
#49562=CARTESIAN_POINT('Ctrl Pts',(3.14257968705312,1.64054732673751,-4.42065775217963));
#49563=CARTESIAN_POINT('Ctrl Pts',(3.2276089004457,1.4664013198912,-4.42717116214137));
#49564=CARTESIAN_POINT('Ctrl Pts',(3.29789079596611,1.2864798567823,-4.4336845721031));
#49565=CARTESIAN_POINT('Ctrl Pts',(3.32644295523914,1.21338640599696,-4.43633065780213));
#49566=CARTESIAN_POINT('Ctrl Pts',(3.35256060096538,1.13933993490305,-4.43897674350117));
#49567=CARTESIAN_POINT('Ctrl Pts',(3.37615800564866,1.06449853024478,-4.44162282920021));
#49568=CARTESIAN_POINT('Ctrl Pts',(3.410646236963,0.955115837089003,-4.44549015346281));
#49569=CARTESIAN_POINT('Ctrl Pts',(3.43975080156849,0.844035097395934,-4.4493574777254));
#49570=CARTESIAN_POINT('Ctrl Pts',(3.46340847798809,0.731814199250707,-4.453224801988));
#49571=CARTESIAN_POINT('Ctrl Pts',(3.50325311857094,0.542809950770156,-4.45973821194964));
#49572=CARTESIAN_POINT('Ctrl Pts',(3.52765418600473,0.350559382295599,-4.46625162191127));
#49573=CARTESIAN_POINT('Ctrl Pts',(3.53632795873358,0.157598006434378,-4.47276503187291));
#49574=CARTESIAN_POINT('Ctrl Pts',(3.54294168510181,0.0104655210122198,
-4.47773148794191));
#49575=CARTESIAN_POINT('Ctrl Pts',(3.54040940290031,-0.137092750504991,
-4.48269794401091));
#49576=CARTESIAN_POINT('Ctrl Pts',(3.52859722973483,-0.283904192124258,
-4.4876644000799));
#49577=CARTESIAN_POINT('Ctrl Pts',(3.52491796890859,-0.329633083703001,
-4.48921135397263));
#49578=CARTESIAN_POINT('Ctrl Pts',(3.52033846393456,-0.375289512400935,
-4.49075830786536));
#49579=CARTESIAN_POINT('Ctrl Pts',(3.5148682535165,-0.420839119723915,-4.49230526175808));
#49580=CARTESIAN_POINT('Ctrl Pts',(3.49183607188734,-0.612624581126916,
-4.4988186717197));
#49581=CARTESIAN_POINT('Ctrl Pts',(3.4530172602035,-0.80249780061272,-4.5053320816813));
#49582=CARTESIAN_POINT('Ctrl Pts',(3.3991184205719,-0.987978897271879,-4.51184549164292));
#49583=CARTESIAN_POINT('Ctrl Pts',(3.34521958093952,-1.17345999393373,-4.51835890160464));
#49584=CARTESIAN_POINT('Ctrl Pts',(3.2762331580479,-1.35457174622048,-4.52487231156637));
#49585=CARTESIAN_POINT('Ctrl Pts',(3.19284833403879,-1.52881164096968,-4.5313857215281));
#49586=CARTESIAN_POINT('Ctrl Pts',(3.18294627225166,-1.5495028665505,-4.5321591978609));
#49587=CARTESIAN_POINT('Ctrl Pts',(3.17284133069424,-1.57009682188359,-4.5329326741937));
#49588=CARTESIAN_POINT('Ctrl Pts',(3.1625347146805,-1.5905892551004,-4.5337061505265));
#49589=CARTESIAN_POINT('Ctrl Pts',(3.08604977345116,-1.74266269493216,-4.53944608415534));
#49590=CARTESIAN_POINT('Ctrl Pts',(2.99845761324308,-1.88914457163618,-4.54518601778417));
#49591=CARTESIAN_POINT('Ctrl Pts',(2.90086776956525,-2.02860868265436,-4.550925951413));
#49592=CARTESIAN_POINT('Ctrl Pts',(2.79012734971569,-2.18686607528926,-4.55743936137464));
#49593=CARTESIAN_POINT('Ctrl Pts',(2.6665030824214,-2.33610851677235,-4.56395277133627));
#49594=CARTESIAN_POINT('Ctrl Pts',(2.53155468743157,-2.47431060311237,-4.57046618129807));
#49595=CARTESIAN_POINT('Ctrl Pts',(2.46745412259722,-2.53995667319974,-4.57356005475674));
#49596=CARTESIAN_POINT('Ctrl Pts',(2.40079731960751,-2.60311185453884,-4.57665392821545));
#49597=CARTESIAN_POINT('Ctrl Pts',(2.33176068881981,-2.66354877749069,-4.57974780167416));
#49598=CARTESIAN_POINT('Ctrl Pts',(2.25545721933669,-2.7303473285424,-4.58316733817743));
#49599=CARTESIAN_POINT('Ctrl Pts',(2.17624654724241,-2.79382517537667,-4.5865868746807));
#49600=CARTESIAN_POINT('Ctrl Pts',(2.09446454668198,-2.85378693812754,-4.59000641118393));
#49601=CARTESIAN_POINT('Ctrl Pts',(1.93868913775044,-2.96799994403061,-4.59651982114573));
#49602=CARTESIAN_POINT('Ctrl Pts',(1.77358024536384,-3.06946424600634,-4.60303323110737));
#49603=CARTESIAN_POINT('Ctrl Pts',(1.60134875634575,-3.15690183524312,-4.609546641069));
#49604=CARTESIAN_POINT('Ctrl Pts',(1.45818170002382,-3.22958414400259,-4.61496089914771));
#49605=CARTESIAN_POINT('Ctrl Pts',(1.31007763847309,-3.29257884054208,-4.62037515722643));
#49606=CARTESIAN_POINT('Ctrl Pts',(1.15835136238572,-3.34511914903784,-4.62578941530514));
#49607=CARTESIAN_POINT('Ctrl Pts',(1.12754931718851,-3.35578538957768,-4.62688856718806));
#49608=CARTESIAN_POINT('Ctrl Pts',(1.09659801000313,-3.36602081032388,-4.62798771907099));
#49609=CARTESIAN_POINT('Ctrl Pts',(1.06551003781568,-3.37582359101795,-4.62908687095391));
#49610=CARTESIAN_POINT('Ctrl Pts',(0.8812873558714,-3.43391340591755,-4.63560028091563));
#49611=CARTESIAN_POINT('Ctrl Pts',(0.692289542666389,-3.47680428037546,
-4.64211369087736));
#49612=CARTESIAN_POINT('Ctrl Pts',(0.501080685143525,-3.50414476472143,
-4.64862710083908));
#49613=CARTESIAN_POINT('Ctrl Pts',(0.309871827623432,-3.53148524906699,
-4.6551405108007));
#49614=CARTESIAN_POINT('Ctrl Pts',(0.116428217970221,-3.54327886708705,
-4.6616539207623));
#49615=CARTESIAN_POINT('Ctrl Pts',(-0.0766918204989502,-3.53915174526628,
-4.66816733072392));
#49616=CARTESIAN_POINT('Ctrl Pts',(-0.112902286566704,-3.53837790011881,
-4.66938861056764));
#49617=CARTESIAN_POINT('Ctrl Pts',(-0.149100544630311,-3.53704430365368,
-4.67060989041136));
#49618=CARTESIAN_POINT('Ctrl Pts',(-0.185269285100072,-3.53514855303133,
-4.67183117025508));
#49619=CARTESIAN_POINT('Ctrl Pts',(-0.341998049399606,-3.52693376178892,
-4.67712330037308));
#49620=CARTESIAN_POINT('Ctrl Pts',(-0.49817233969735,-3.50816226468903,
-4.68241543049107));
#49621=CARTESIAN_POINT('Ctrl Pts',(-0.652411741910373,-3.47918285964478,
-4.687707560609));
#49622=CARTESIAN_POINT('Ctrl Pts',(-0.842245399180027,-3.44351579684425,
-4.69422097028656));
#49623=CARTESIAN_POINT('Ctrl Pts',(-1.02917125682124,-3.39238617446652,
-4.70073437996402));
#49624=CARTESIAN_POINT('Ctrl Pts',(-1.21071388767511,-3.32640898762537,
-4.70724778964203));
#49625=CARTESIAN_POINT('',(-3.939231012049,0.6945927106677,-1.608333333333));
#49626=CARTESIAN_POINT('Ctrl Pts',(-1.507124460135,-3.179723940534,0.3249781788769));
#49627=CARTESIAN_POINT('Ctrl Pts',(-1.847411431725,-3.018434838732,0.3122038733214));
#49628=CARTESIAN_POINT('Ctrl Pts',(-2.475686234802,-2.585698153946,0.2866552622103));
#49629=CARTESIAN_POINT('Ctrl Pts',(-3.165156557639,-1.672326772638,0.2483323455436));
#49630=CARTESIAN_POINT('Ctrl Pts',(-3.531155462695,-0.588062549222,0.2100094288769));
#49631=CARTESIAN_POINT('Ctrl Pts',(-3.53629937207,0.5562993812307,0.1716865122103));
#49632=CARTESIAN_POINT('Ctrl Pts',(-3.180057548144,1.643810961166,0.1333635955436));
#49633=CARTESIAN_POINT('Ctrl Pts',(-2.498836731037,2.563336879767,0.09504067887693));
#49634=CARTESIAN_POINT('Ctrl Pts',(-1.56225248291,3.220907950999,0.05671776221027));
#49635=CARTESIAN_POINT('Ctrl Pts',(-0.466017154887,3.54932513108,0.0183948455436));
#49636=CARTESIAN_POINT('Ctrl Pts',(0.6778418198014,3.515026505956,-0.01992807112307));
#49637=CARTESIAN_POINT('Ctrl Pts',(1.752430176593,3.121517154665,-0.05825098778973));
#49638=CARTESIAN_POINT('Ctrl Pts',(2.647932624627,2.409010935266,-0.0965739044564));
#49639=CARTESIAN_POINT('Ctrl Pts',(3.272835177738,1.450320919686,-0.1348968211231));
#49640=CARTESIAN_POINT('Ctrl Pts',(3.563277236448,0.3434184138391,-0.1732197377897));
#49641=CARTESIAN_POINT('Ctrl Pts',(3.489577686554,-0.7985790131506,-0.2115426544564));
#49642=CARTESIAN_POINT('Ctrl Pts',(3.059268098266,-1.858967340668,-0.2498655711231));
#49643=CARTESIAN_POINT('Ctrl Pts',(2.316323053204,-2.729382418045,-0.2881884877897));
#49644=CARTESIAN_POINT('Ctrl Pts',(1.336666254706,-3.320874010599,-0.3265114044564));
#49645=CARTESIAN_POINT('Ctrl Pts',(0.2204116649468,-3.572995881427,-0.3648343211231));
#49646=CARTESIAN_POINT('Ctrl Pts',(-0.9183674304569,-3.459982967215,-0.4031572377897));
#49647=CARTESIAN_POINT('Ctrl Pts',(-1.9632959015,-2.993384384588,-0.4414801544564));
#49648=CARTESIAN_POINT('Ctrl Pts',(-2.807589484972,-2.220883192474,-0.4798030711231));
#49649=CARTESIAN_POINT('Ctrl Pts',(-3.364967377215,-1.221423522379,-0.5181259877897));
#49650=CARTESIAN_POINT('Ctrl Pts',(-3.578469519044,-0.09714304921396,-0.5564489044564));
#49651=CARTESIAN_POINT('Ctrl Pts',(-3.426277508971,1.037064753165,-0.5947718211231));
#49652=CARTESIAN_POINT('Ctrl Pts',(-2.923944288764,2.06529190841,-0.6330947377897));
#49653=CARTESIAN_POINT('Ctrl Pts',(-2.122804743339,2.882460909084,-0.6714176544564));
#49654=CARTESIAN_POINT('Ctrl Pts',(-1.104729640369,3.405062891112,-0.7097405711231));
#49655=CARTESIAN_POINT('Ctrl Pts',(0.02624098029853,3.579691646175,-0.7480634877897));
#49656=CARTESIAN_POINT('Ctrl Pts',(1.15452995928,3.388501356628,-0.7863864044564));
#49657=CARTESIAN_POINT('Ctrl Pts',(2.164834181912,2.851030311232,-0.8247093211231));
#49658=CARTESIAN_POINT('Ctrl Pts',(2.95390773709,2.022204230908,-0.8630322377897));
#49659=CARTESIAN_POINT('Ctrl Pts',(3.441112915587,0.9867232504197,-0.9013551544564));
#49660=CARTESIAN_POINT('Ctrl Pts',(3.576660810833,-0.1495938334094,-0.9396780711231));
#49661=CARTESIAN_POINT('Ctrl Pts',(3.3466993913,-1.270623490659,-0.9780009877897));
#49662=CARTESIAN_POINT('Ctrl Pts',(2.77472907968,-2.261804457755,-1.016323904456));
#49663=CARTESIAN_POINT('Ctrl Pts',(1.919201176706,-3.021845084393,-1.054646821123));
#49664=CARTESIAN_POINT('Ctrl Pts',(0.8675445536438,-3.473074620302,-1.09296973779));
#49665=CARTESIAN_POINT('Ctrl Pts',(-0.2727689569774,-3.569380613895,-1.131292654456));
#49666=CARTESIAN_POINT('Ctrl Pts',(-1.385207418822,-3.300921277095,-1.169615571123));
#49667=CARTESIAN_POINT('Ctrl Pts',(-2.356087527427,-2.695131246125,-1.20793848779));
#49668=CARTESIAN_POINT('Ctrl Pts',(-3.086192235944,-1.813917956672,-1.246261404456));
#49669=CARTESIAN_POINT('Ctrl Pts',(-3.500910032172,-0.7473351439477,-1.284584321123));
#49670=CARTESIAN_POINT('Ctrl Pts',(-3.557859704823,0.3956200090186,-1.32290723779));
#49671=CARTESIAN_POINT('Ctrl Pts',(-3.251221402107,1.498145608819,-1.361230154456));
#49672=CARTESIAN_POINT('Ctrl Pts',(-2.612331379217,2.447571375037,-1.399553071123));
#49673=CARTESIAN_POINT('Ctrl Pts',(-1.706479655765,3.146872742136,-1.43787598779));
#49674=CARTESIAN_POINT('Ctrl Pts',(-0.6262378398082,3.524586080483,-1.476198904456));
#49675=CARTESIAN_POINT('Ctrl Pts',(0.5180010325718,3.542111771387,-1.514521821123));
#49676=CARTESIAN_POINT('Ctrl Pts',(1.609303880967,3.197658813796,-1.55284473779));
#49677=CARTESIAN_POINT('Ctrl Pts',(2.536147310391,2.526427851876,-1.591167654456));
#49678=CARTESIAN_POINT('Ctrl Pts',(3.203814509633,1.597013919356,-1.629490571123));
#49679=CARTESIAN_POINT('Ctrl Pts',(3.544074636176,0.504396514588,-1.66781348779));
#49680=CARTESIAN_POINT('Ctrl Pts',(3.522155523411,-0.639766629091,-1.706136404456));
#49681=CARTESIAN_POINT('Ctrl Pts',(3.140297148798,-1.718550170333,-1.744459321123));
#49682=CARTESIAN_POINT('Ctrl Pts',(2.437522724574,-2.6217100979,-1.78278223779));
#49683=CARTESIAN_POINT('Ctrl Pts',(1.485650801008,-3.25694988789,-1.821105154456));
#49684=CARTESIAN_POINT('Ctrl Pts',(0.3819559277091,-3.55935254203,-1.859428071123));
#49685=CARTESIAN_POINT('Ctrl Pts',(-0.7607721390542,-3.498014682644,-1.89775098779));
#49686=CARTESIAN_POINT('Ctrl Pts',(-1.825754654292,-3.07920451219,-1.936073904456));
#49687=CARTESIAN_POINT('Ctrl Pts',(-2.704158191128,-2.345721792501,-1.974396821123));
#49688=CARTESIAN_POINT('Ctrl Pts',(-3.306215340777,-1.372521979396,-2.01271973779));
#49689=CARTESIAN_POINT('Ctrl Pts',(-3.570403165657,-0.2590638985198,-2.051042654456));
#49690=CARTESIAN_POINT('Ctrl Pts',(-3.469712261373,0.8808825686702,-2.089365571123));
#49691=CARTESIAN_POINT('Ctrl Pts',(-3.166220516368,1.580799011723,-2.114914182234));
#49692=CARTESIAN_POINT('Ctrl Pts',(-2.963111000121,1.897904549051,-2.12768848779));
#49693=CARTESIAN_POINT('Ctrl Pts',(-1.57884649994,-3.331042755313,0.2282975453458));
#49694=CARTESIAN_POINT('Ctrl Pts',(-1.935327273944,-3.16207812061,0.2155232397903));
#49695=CARTESIAN_POINT('Ctrl Pts',(-2.593500835636,-2.708748075055,0.1899746286792));
#49696=CARTESIAN_POINT('Ctrl Pts',(-3.315782130125,-1.751910569814,0.1516517120125));
#49697=CARTESIAN_POINT('Ctrl Pts',(-3.699198434163,-0.6160476603915,0.1133287953458));
#49698=CARTESIAN_POINT('Ctrl Pts',(-3.704587135314,0.5827729256655,0.07500587867917));
#49699=CARTESIAN_POINT('Ctrl Pts',(-3.331392238863,1.722037728966,0.0366829620125));
#49700=CARTESIAN_POINT('Ctrl Pts',(-2.617753033062,2.685322657708,-0.001639954654168));
#49701=CARTESIAN_POINT('Ctrl Pts',(-1.636597991677,3.374186657821,-0.03996287132083));
#49702=CARTESIAN_POINT('Ctrl Pts',(-0.4881942887712,3.718232772795,-0.0782857879875));
#49703=CARTESIAN_POINT('Ctrl Pts',(0.7100994065285,3.682301921918,-0.1166087046542));
#49704=CARTESIAN_POINT('Ctrl Pts',(1.835825987759,3.270065986259,-0.1549316213208));
#49705=CARTESIAN_POINT('Ctrl Pts',(2.773944201061,2.523652547661,-0.1932545379875));
#49706=CARTESIAN_POINT('Ctrl Pts',(3.428585031915,1.51933975488,-0.2315774546542));
#49707=CARTESIAN_POINT('Ctrl Pts',(3.73284884022,0.3597612374072,-0.2699003713208));
#49708=CARTESIAN_POINT('Ctrl Pts',(3.655642027196,-0.8365823216256,-0.3082232879875));
#49709=CARTESIAN_POINT('Ctrl Pts',(3.20485458042,-1.947433113158,-0.3465462046542));
#49710=CARTESIAN_POINT('Ctrl Pts',(2.426553773107,-2.859270081346,-0.3848691213208));
#49711=CARTESIAN_POINT('Ctrl Pts',(1.400276416216,-3.478909968661,-0.4231920379875));
#49712=CARTESIAN_POINT('Ctrl Pts',(0.2309007616505,-3.743029982531,-0.4615149546542));
#49713=CARTESIAN_POINT('Ctrl Pts',(-0.9620713096952,-3.624638934697,-0.4998378713208));
#49714=CARTESIAN_POINT('Ctrl Pts',(-2.056726530835,-3.135835548816,-0.5381607879875));
#49715=CARTESIAN_POINT('Ctrl Pts',(-2.941198918117,-2.326572056896,-0.5764837046542));
#49716=CARTESIAN_POINT('Ctrl Pts',(-3.525101679693,-1.279549436203,-0.6148066213208));
#49717=CARTESIAN_POINT('Ctrl Pts',(-3.748764103251,-0.10176595716,-0.6531295379875));
#49718=CARTESIAN_POINT('Ctrl Pts',(-3.58932947872,1.086417279432,-0.6914524546542));
#49719=CARTESIAN_POINT('Ctrl Pts',(-3.063090891592,2.163576391465,-0.7297753713208));
#49720=CARTESIAN_POINT('Ctrl Pts',(-2.223826185381,3.019633373288,-0.7680982879875));
#49721=CARTESIAN_POINT('Ctrl Pts',(-1.15730224823,3.567105285536,-0.8064212046542));
#49722=CARTESIAN_POINT('Ctrl Pts',(0.02748975349761,3.750044389779,-0.8447441213208));
#49723=CARTESIAN_POINT('Ctrl Pts',(1.209472497793,3.549755609749,-0.8830670379875));
#49724=CARTESIAN_POINT('Ctrl Pts',(2.267855748792,2.98670703527,-0.9213899546542));
#49725=CARTESIAN_POINT('Ctrl Pts',(3.094480260398,2.118438228948,-0.9597128713208));
#49726=CARTESIAN_POINT('Ctrl Pts',(3.60487088252,1.033680091819,-0.9980357879875));
#49727=CARTESIAN_POINT('Ctrl Pts',(3.746869321032,-0.1567128041103,-1.036358704654));
#49728=CARTESIAN_POINT('Ctrl Pts',(3.505964344731,-1.331090765251,-1.074681621321));
#49729=CARTESIAN_POINT('Ctrl Pts',(2.906774730033,-2.369440710527,-1.113004537988));
#49730=CARTESIAN_POINT('Ctrl Pts',(2.010533396991,-3.165650655307,-1.151327454654));
#49731=CARTESIAN_POINT('Ctrl Pts',(0.908829840065,-3.638353602066,-1.189650371321));
#49732=CARTESIAN_POINT('Ctrl Pts',(-0.2857496672687,-3.739242669247,-1.227973287988));
#49733=CARTESIAN_POINT('Ctrl Pts',(-1.451127589491,-3.458007711223,-1.266296204654));
#49734=CARTESIAN_POINT('Ctrl Pts',(-2.46821058554,-2.823388941908,-1.304619121321));
#49735=CARTESIAN_POINT('Ctrl Pts',(-3.233060001844,-1.900239889155,-1.342942037988));
#49736=CARTESIAN_POINT('Ctrl Pts',(-3.667513664004,-0.7828998251401,-1.381264954654));
#49737=CARTESIAN_POINT('Ctrl Pts',(-3.727173495502,0.4144470367691,-1.419587871321));
#49738=CARTESIAN_POINT('Ctrl Pts',(-3.405942685574,1.569440357084,-1.457910787988));
#49739=CARTESIAN_POINT('Ctrl Pts',(-2.736648739939,2.564048027251,-1.496233704654));
#49740=CARTESIAN_POINT('Ctrl Pts',(-1.787688743027,3.296628212267,-1.534556621321));
#49741=CARTESIAN_POINT('Ctrl Pts',(-0.6560396620613,3.692316423827,-1.572879537988));
#49742=CARTESIAN_POINT('Ctrl Pts',(0.5426520097537,3.71067613895,-1.611202454654));
#49743=CARTESIAN_POINT('Ctrl Pts',(1.685888502915,3.349831125236,-1.649525371321));
#49744=CARTESIAN_POINT('Ctrl Pts',(2.656839173046,2.646657178484,-1.687848287988));
#49745=CARTESIAN_POINT('Ctrl Pts',(3.356279762414,1.673013678449,-1.726171204654));
#49746=CARTESIAN_POINT('Ctrl Pts',(3.712732413852,0.5284000709324,-1.764494121321));
#49747=CARTESIAN_POINT('Ctrl Pts',(3.689770199791,-0.670212268354,-1.802817037988));
#49748=CARTESIAN_POINT('Ctrl Pts',(3.289739695226,-1.800333677259,-1.841139954654));
#49749=CARTESIAN_POINT('Ctrl Pts',(2.553521174936,-2.746473779316,-1.879462871321));
#49750=CARTESIAN_POINT('Ctrl Pts',(1.55635093806,-3.411943782343,-1.917785787988));
#49751=CARTESIAN_POINT('Ctrl Pts',(0.4001327000829,-3.728737374837,-1.956108704654));
#49752=CARTESIAN_POINT('Ctrl Pts',(-0.7969762688943,-3.66448052866,-1.994431621321));
#49753=CARTESIAN_POINT('Ctrl Pts',(-1.912639879403,-3.22573974165,-2.032754537988));
#49754=CARTESIAN_POINT('Ctrl Pts',(-2.832845467165,-2.457351559135,-2.071077454654));
#49755=CARTESIAN_POINT('Ctrl Pts',(-3.463553712324,-1.437838466947,-2.109400371321));
#49756=CARTESIAN_POINT('Ctrl Pts',(-3.740313882881,-0.2713924033866,-2.147723287988));
#49757=CARTESIAN_POINT('Ctrl Pts',(-3.634831232967,0.9228025934093,-2.186046204654));
#49758=CARTESIAN_POINT('Ctrl Pts',(-3.31689672123,1.656027125022,-2.211594815765));
#49759=CARTESIAN_POINT('Ctrl Pts',(-3.104121494422,1.988223291274,-2.224369121321));
#49760=CARTESIAN_POINT('Ctrl Pts',(-1.650568539745,-3.482361570092,0.1316169118147));
#49761=CARTESIAN_POINT('Ctrl Pts',(-2.023243116164,-3.305721402488,0.1188426062592));
#49762=CARTESIAN_POINT('Ctrl Pts',(-2.711315436469,-2.831797996164,0.09329399514806));
#49763=CARTESIAN_POINT('Ctrl Pts',(-3.466407702612,-1.83149436699,0.0549710784814));
#49764=CARTESIAN_POINT('Ctrl Pts',(-3.867241405631,-0.644032771561,0.01664816181473));
#49765=CARTESIAN_POINT('Ctrl Pts',(-3.872874898558,0.6092464701004,-0.02167475485194));
#49766=CARTESIAN_POINT('Ctrl Pts',(-3.482726929583,1.800264496766,-0.0599976715186));
#49767=CARTESIAN_POINT('Ctrl Pts',(-2.736669335086,2.80730843565,-0.09832058818527));
#49768=CARTESIAN_POINT('Ctrl Pts',(-1.710943500445,3.527465364644,-0.1366435048519));
#49769=CARTESIAN_POINT('Ctrl Pts',(-0.5103714226555,3.88714041451,-0.1749664215186));
#49770=CARTESIAN_POINT('Ctrl Pts',(0.7423569932556,3.849577337881,-0.2132893381853));
#49771=CARTESIAN_POINT('Ctrl Pts',(1.919221798925,3.418614817852,-0.2516122548519));
#49772=CARTESIAN_POINT('Ctrl Pts',(2.899955777496,2.638294160056,-0.2899351715186));
#49773=CARTESIAN_POINT('Ctrl Pts',(3.584334886092,1.588358590075,-0.3282580881853));
#49774=CARTESIAN_POINT('Ctrl Pts',(3.902420443991,0.3761040609753,-0.3665810048519));
#49775=CARTESIAN_POINT('Ctrl Pts',(3.821706367838,-0.8745856301006,-0.4049039215186));
#49776=CARTESIAN_POINT('Ctrl Pts',(3.350441062573,-2.035898885647,-0.4432268381853));
#49777=CARTESIAN_POINT('Ctrl Pts',(2.536784493009,-2.989157744647,-0.4815497548519));
#49778=CARTESIAN_POINT('Ctrl Pts',(1.463886577727,-3.636945926723,-0.5198726715186));
#49779=CARTESIAN_POINT('Ctrl Pts',(0.2413898583541,-3.913064083635,-0.5581955881853));
#49780=CARTESIAN_POINT('Ctrl Pts',(-1.005775188934,-3.789294902179,-0.5965185048519));
#49781=CARTESIAN_POINT('Ctrl Pts',(-2.15015716017,-3.278286713044,-0.6348414215186));
#49782=CARTESIAN_POINT('Ctrl Pts',(-3.074808351262,-2.432260921317,-0.6731643381853));
#49783=CARTESIAN_POINT('Ctrl Pts',(-3.685235982171,-1.337675350026,-0.7114872548519));
#49784=CARTESIAN_POINT('Ctrl Pts',(-3.919058687457,-0.1063888651061,-0.7498101715186));
#49785=CARTESIAN_POINT('Ctrl Pts',(-3.752381448469,1.1357698057,-0.7881330881853));
#49786=CARTESIAN_POINT('Ctrl Pts',(-3.20223749442,2.26186087452,-0.8264560048519));
#49787=CARTESIAN_POINT('Ctrl Pts',(-2.324847627423,3.156805837491,-0.8647789215186));
#49788=CARTESIAN_POINT('Ctrl Pts',(-1.209874856091,3.72914767996,-0.9031018381853));
#49789=CARTESIAN_POINT('Ctrl Pts',(0.02873852669669,3.920397133383,-0.9414247548519));
#49790=CARTESIAN_POINT('Ctrl Pts',(1.264415036307,3.71100986287,-0.9797476715186));
#49791=CARTESIAN_POINT('Ctrl Pts',(2.370877315672,3.122383759307,-1.018070588185));
#49792=CARTESIAN_POINT('Ctrl Pts',(3.235052783705,2.214672226988,-1.056393504852));
#49793=CARTESIAN_POINT('Ctrl Pts',(3.768628849452,1.080636933218,-1.094716421519));
#49794=CARTESIAN_POINT('Ctrl Pts',(3.91707783123,-0.1638317748112,-1.133039338185));
#49795=CARTESIAN_POINT('Ctrl Pts',(3.665229298162,-1.391558039842,-1.171362254852));
#49796=CARTESIAN_POINT('Ctrl Pts',(3.038820380385,-2.477076963299,-1.209685171519));
#49797=CARTESIAN_POINT('Ctrl Pts',(2.101865617276,-3.30945622622,-1.248008088185));
#49798=CARTESIAN_POINT('Ctrl Pts',(0.9501151264862,-3.80363258383,-1.286331004852));
#49799=CARTESIAN_POINT('Ctrl Pts',(-0.29873037756,-3.909104724598,-1.324653921519));
#49800=CARTESIAN_POINT('Ctrl Pts',(-1.51704776016,-3.615094145351,-1.362976838185));
#49801=CARTESIAN_POINT('Ctrl Pts',(-2.580333643652,-2.951646637691,-1.401299754852));
#49802=CARTESIAN_POINT('Ctrl Pts',(-3.379927767743,-1.986561821639,-1.439622671519));
#49803=CARTESIAN_POINT('Ctrl Pts',(-3.834117295836,-0.8184645063324,-1.477945588185));
#49804=CARTESIAN_POINT('Ctrl Pts',(-3.896487286181,0.4332740645197,-1.516268504852));
#49805=CARTESIAN_POINT('Ctrl Pts',(-3.560663969041,1.640735105349,-1.554591421519));
#49806=CARTESIAN_POINT('Ctrl Pts',(-2.860966100662,2.680524679464,-1.592914338185));
#49807=CARTESIAN_POINT('Ctrl Pts',(-1.868897830289,3.446383682398,-1.631237254852));
#49808=CARTESIAN_POINT('Ctrl Pts',(-0.6858414843143,3.860046767171,-1.669560171519));
#49809=CARTESIAN_POINT('Ctrl Pts',(0.5673029869357,3.879240506513,-1.707883088185));
#49810=CARTESIAN_POINT('Ctrl Pts',(1.762473124864,3.502003436675,-1.746206004852));
#49811=CARTESIAN_POINT('Ctrl Pts',(2.777531035702,2.766886505093,-1.784528921519));
#49812=CARTESIAN_POINT('Ctrl Pts',(3.508745015196,1.749013437542,-1.822851838185));
#49813=CARTESIAN_POINT('Ctrl Pts',(3.881390191529,0.5524036272767,-1.861174754852));
#49814=CARTESIAN_POINT('Ctrl Pts',(3.857384876171,-0.7006579076169,-1.899497671519));
#49815=CARTESIAN_POINT('Ctrl Pts',(3.439182241653,-1.882117184185,-1.937820588185));
#49816=CARTESIAN_POINT('Ctrl Pts',(2.669519625297,-2.871237460732,-1.976143504852));
#49817=CARTESIAN_POINT('Ctrl Pts',(1.627051075112,-3.566937676797,-2.014466421519));
#49818=CARTESIAN_POINT('Ctrl Pts',(0.4183094724568,-3.898122207644,-2.052789338185));
#49819=CARTESIAN_POINT('Ctrl Pts',(-0.8331803987343,-3.830946374675,-2.091112254852));
#49820=CARTESIAN_POINT('Ctrl Pts',(-1.999525104514,-3.37227497111,-2.129435171519));
#49821=CARTESIAN_POINT('Ctrl Pts',(-2.961532743202,-2.56898132577,-2.167758088185));
#49822=CARTESIAN_POINT('Ctrl Pts',(-3.62089208387,-1.503154954499,-2.206081004852));
#49823=CARTESIAN_POINT('Ctrl Pts',(-3.910224600105,-0.2837209082534,-2.244403921519));
#49824=CARTESIAN_POINT('Ctrl Pts',(-3.799950204561,0.9647226181484,-2.282726838185));
#49825=CARTESIAN_POINT('Ctrl Pts',(-3.467572926091,1.731255238321,-2.308275449296));
#49826=CARTESIAN_POINT('Ctrl Pts',(-3.245131988724,2.078542033497,-2.321049754852));
#49827=CARTESIAN_POINT('Ctrl Pts',(-1.72229057955,-3.633680384871,0.03493627828363));
#49828=CARTESIAN_POINT('Ctrl Pts',(-2.111158958383,-3.449364684366,0.02216197272807));
#49829=CARTESIAN_POINT('Ctrl Pts',(-2.829130037303,-2.954847917273,-0.003386638383041));
#49830=CARTESIAN_POINT('Ctrl Pts',(-3.617033275098,-1.911078164166,-0.04170955504971));
#49831=CARTESIAN_POINT('Ctrl Pts',(-4.035284377099,-0.6720178827305,-0.08003247171637));
#49832=CARTESIAN_POINT('Ctrl Pts',(-4.041162661802,0.6357200145352,-0.118355388383));
#49833=CARTESIAN_POINT('Ctrl Pts',(-3.634061620302,1.878491264566,-0.1566783050497));
#49834=CARTESIAN_POINT('Ctrl Pts',(-2.855585637111,2.929294213592,-0.1950012217164));
#49835=CARTESIAN_POINT('Ctrl Pts',(-1.785289009212,3.680744071466,-0.233324138383));
#49836=CARTESIAN_POINT('Ctrl Pts',(-0.5325485565397,4.056048056224,-0.2716470550497));
#49837=CARTESIAN_POINT('Ctrl Pts',(0.7746145799827,4.016852753843,-0.3099699717164));
#49838=CARTESIAN_POINT('Ctrl Pts',(2.002617610091,3.567163649446,-0.348292888383));
#49839=CARTESIAN_POINT('Ctrl Pts',(3.02596735393,2.752935772451,-0.3866158050497));
#49840=CARTESIAN_POINT('Ctrl Pts',(3.74008474027,1.65737742527,-0.4249387217164));
#49841=CARTESIAN_POINT('Ctrl Pts',(4.071992047763,0.3924468845434,-0.463261638383));
#49842=CARTESIAN_POINT('Ctrl Pts',(3.98777070848,-0.9125889385755,-0.5015845550497));
#49843=CARTESIAN_POINT('Ctrl Pts',(3.496027544726,-2.124364658137,-0.5399074717164));
#49844=CARTESIAN_POINT('Ctrl Pts',(2.647015212912,-3.119045407947,-0.578230388383));
#49845=CARTESIAN_POINT('Ctrl Pts',(1.527496739238,-3.794981884784,-0.6165533050497));
#49846=CARTESIAN_POINT('Ctrl Pts',(0.2518789550578,-4.08309818474,-0.6548762217164));
#49847=CARTESIAN_POINT('Ctrl Pts',(-1.049479068172,-3.953950869661,-0.693199138383));
#49848=CARTESIAN_POINT('Ctrl Pts',(-2.243587789505,-3.420737877273,-0.7315220550497));
#49849=CARTESIAN_POINT('Ctrl Pts',(-3.208417784407,-2.537949785738,-0.7698449717164));
#49850=CARTESIAN_POINT('Ctrl Pts',(-3.845370284649,-1.39580126385,-0.808167888383));
#49851=CARTESIAN_POINT('Ctrl Pts',(-4.089353271664,-0.1110117730522,-0.8464908050497));
#49852=CARTESIAN_POINT('Ctrl Pts',(-3.915433418218,1.185122331967,-0.8848137217164));
#49853=CARTESIAN_POINT('Ctrl Pts',(-3.341384097248,2.360145357575,-0.923136638383));
#49854=CARTESIAN_POINT('Ctrl Pts',(-2.425869069466,3.293978301694,-0.9614595550497));
#49855=CARTESIAN_POINT('Ctrl Pts',(-1.262447463952,3.891190074384,-0.9997824717164));
#49856=CARTESIAN_POINT('Ctrl Pts',(0.02998729989577,4.090749876987,-1.038105388383));
#49857=CARTESIAN_POINT('Ctrl Pts',(1.31935757482,3.872264115991,-1.07642830505));
#49858=CARTESIAN_POINT('Ctrl Pts',(2.473898882552,3.258060483344,-1.114751221716));
#49859=CARTESIAN_POINT('Ctrl Pts',(3.375625307013,2.310906225029,-1.153074138383));
#49860=CARTESIAN_POINT('Ctrl Pts',(3.932386816384,1.127593774617,-1.19139705505));
#49861=CARTESIAN_POINT('Ctrl Pts',(4.087286341429,-0.1709507455122,-1.229719971716));
#49862=CARTESIAN_POINT('Ctrl Pts',(3.824494251593,-1.452025314433,-1.268042888383));
#49863=CARTESIAN_POINT('Ctrl Pts',(3.170866030738,-2.584713216072,-1.30636580505));
#49864=CARTESIAN_POINT('Ctrl Pts',(2.19319783756,-3.453261797134,-1.344688721716));
#49865=CARTESIAN_POINT('Ctrl Pts',(0.9914004129074,-3.968911565595,-1.383011638383));
#49866=CARTESIAN_POINT('Ctrl Pts',(-0.3117110878513,-4.07896677995,-1.42133455505));
#49867=CARTESIAN_POINT('Ctrl Pts',(-1.582967930829,-3.772180579478,-1.459657471716));
#49868=CARTESIAN_POINT('Ctrl Pts',(-2.692456701765,-3.079904333473,-1.497980388383));
#49869=CARTESIAN_POINT('Ctrl Pts',(-3.526795533643,-2.072883754122,-1.53630330505));
#49870=CARTESIAN_POINT('Ctrl Pts',(-4.000720927668,-0.8540291875248,-1.574626221716));
#49871=CARTESIAN_POINT('Ctrl Pts',(-4.06580107686,0.4521010922702,-1.612949138383));
#49872=CARTESIAN_POINT('Ctrl Pts',(-3.715385252509,1.712029853614,-1.65127205505));
#49873=CARTESIAN_POINT('Ctrl Pts',(-2.985283461384,2.797001331678,-1.689594971716));
#49874=CARTESIAN_POINT('Ctrl Pts',(-1.95010691755,3.596139152528,-1.727917888383));
#49875=CARTESIAN_POINT('Ctrl Pts',(-0.7156433065674,4.027777110515,-1.76624080505));
#49876=CARTESIAN_POINT('Ctrl Pts',(0.5919539641177,4.047804874075,-1.804563721716));
#49877=CARTESIAN_POINT('Ctrl Pts',(1.839057746813,3.654175748115,-1.842886638383));
#49878=CARTESIAN_POINT('Ctrl Pts',(2.898222898357,2.887115831701,-1.88120955505));
#49879=CARTESIAN_POINT('Ctrl Pts',(3.661210267978,1.825013196635,-1.919532471716));
#49880=CARTESIAN_POINT('Ctrl Pts',(4.050047969205,0.5764071836211,-1.957855388383));
#49881=CARTESIAN_POINT('Ctrl Pts',(4.024999552551,-0.7311035468799,-1.99617830505));
#49882=CARTESIAN_POINT('Ctrl Pts',(3.588624788081,-1.963900691111,-2.034501221716));
#49883=CARTESIAN_POINT('Ctrl Pts',(2.785518075659,-2.996001142148,-2.072824138383));
#49884=CARTESIAN_POINT('Ctrl Pts',(1.697751212165,-3.72193157125,-2.11114705505));
#49885=CARTESIAN_POINT('Ctrl Pts',(0.4364862448306,-4.067507040451,-2.149469971716));
#49886=CARTESIAN_POINT('Ctrl Pts',(-0.8693845285744,-3.997412220691,-2.187792888383));
#49887=CARTESIAN_POINT('Ctrl Pts',(-2.086410329625,-3.518810200571,-2.22611580505));
#49888=CARTESIAN_POINT('Ctrl Pts',(-3.090220019238,-2.680611092404,-2.264438721716));
#49889=CARTESIAN_POINT('Ctrl Pts',(-3.778230455416,-1.568471442051,-2.302761638383));
#49890=CARTESIAN_POINT('Ctrl Pts',(-4.080135317328,-0.2960494131202,-2.34108455505));
#49891=CARTESIAN_POINT('Ctrl Pts',(-3.965069176156,1.006642642887,-2.379407471716));
#49892=CARTESIAN_POINT('Ctrl Pts',(-3.618249130952,1.80648335162,-2.404956082827));
#49893=CARTESIAN_POINT('Ctrl Pts',(-3.386142483025,2.16886077572,-2.417730388383));
#49894=CARTESIAN_POINT('Ctrl Pts',(-0.264621262814254,3.52921885147511,
9.97465998686664E-17));
#49895=CARTESIAN_POINT('Ctrl Pts',(-0.0628839596244878,3.54453750585823,
-0.00696552242425897));
#49896=CARTESIAN_POINT('Ctrl Pts',(0.140163183717197,3.5427563049603,-0.0140558818516256));
#49897=CARTESIAN_POINT('Ctrl Pts',(0.537930260474703,3.50455590115915,-0.0276799019954263));
#49898=CARTESIAN_POINT('Ctrl Pts',(0.731295751643366,3.46899592207308,-0.0341038307636699));
#49899=CARTESIAN_POINT('Ctrl Pts',(1.18992431903622,3.34465894772215,-0.0497494988331141));
#49900=CARTESIAN_POINT('Ctrl Pts',(1.45082056278735,3.23973099148587,-0.0589569369225457));
#49901=CARTESIAN_POINT('Ctrl Pts',(1.85066944756859,3.02196767273769,-0.074569370893028));
#49902=CARTESIAN_POINT('Ctrl Pts',(1.99916397088873,2.92629851593253,-0.0807773580080322));
#49903=CARTESIAN_POINT('Ctrl Pts',(2.33657049127287,2.67098235688989,-0.0953838985417922));
#49904=CARTESIAN_POINT('Ctrl Pts',(2.51563975010642,2.50232952935312,-0.103322805181874));
#49905=CARTESIAN_POINT('Ctrl Pts',(2.89132158504577,2.06707630387109,-0.122258745710041));
#49906=CARTESIAN_POINT('Ctrl Pts',(3.07220853647605,1.78722204088807,-0.133388652163895));
#49907=CARTESIAN_POINT('Ctrl Pts',(3.26863809705789,1.36506427924163,-0.149476363944854));
#49908=CARTESIAN_POINT('Ctrl Pts',(3.31886051343565,1.23867187327451,-0.15422876836737));
#49909=CARTESIAN_POINT('Ctrl Pts',(3.42440714161648,0.919690468397073,-0.165734443856275));
#49910=CARTESIAN_POINT('Ctrl Pts',(3.47036487208215,0.725128900568946,-0.172214871389973));
#49911=CARTESIAN_POINT('Ctrl Pts',(3.56835533108999,0.0691126171902604,
-0.19388016863945));
#49912=CARTESIAN_POINT('Ctrl Pts',(3.54693882903862,-0.404113247195594,
-0.210083038142292));
#49913=CARTESIAN_POINT('Ctrl Pts',(3.3815526767447,-1.07111787131278,-0.233641822018199));
#49914=CARTESIAN_POINT('Ctrl Pts',(3.30723990028449,-1.28082280745294,-0.240907680301654));
#49915=CARTESIAN_POINT('Ctrl Pts',(3.13654495041243,-1.64967350595082,-0.254212335744979));
#49916=CARTESIAN_POINT('Ctrl Pts',(3.04561017614116,-1.8117263716817,-0.260318688146977));
#49917=CARTESIAN_POINT('Ctrl Pts',(2.83566095862384,-2.12627105633583,-0.273207769133487));
#49918=CARTESIAN_POINT('Ctrl Pts',(2.71559024311982,-2.27814918203614,-0.279941531425139));
#49919=CARTESIAN_POINT('Ctrl Pts',(2.24807694153657,-2.77904914090722,-0.30358438205821));
#49920=CARTESIAN_POINT('Ctrl Pts',(1.90488533547708,-2.99649843384656,-0.316427980546006));
#49921=CARTESIAN_POINT('Ctrl Pts',(1.4395827853575,-3.24171823576112,-0.333888702007015));
#49922=CARTESIAN_POINT('Ctrl Pts',(1.2156718830087,-3.33243065426894,-0.342144528390505));
#49923=CARTESIAN_POINT('Ctrl Pts',(0.814386518254699,-3.44939286173748,
-0.356681912885287));
#49924=CARTESIAN_POINT('Ctrl Pts',(0.639761851128878,-3.48637026674257,
-0.362848739836552));
#49925=CARTESIAN_POINT('Ctrl Pts',(0.242142474236125,-3.53855715483033,
-0.376181945411191));
#49926=CARTESIAN_POINT('Ctrl Pts',(0.0189572614360934,-3.54624657594503,
-0.383406933058502));
#49927=CARTESIAN_POINT('Ctrl Pts',(-0.501721552977363,-3.51578977434586,
-0.400737723420411));
#49928=CARTESIAN_POINT('Ctrl Pts',(-0.798405890422845,-3.4608651947752,
-0.410936210186359));
#49929=CARTESIAN_POINT('Ctrl Pts',(-1.22248236323576,-3.32526349446763,
-0.426425182199499));
#49930=CARTESIAN_POINT('Ctrl Pts',(-1.35899635127016,-3.27209778442608,
-0.431497732221111));
#49931=CARTESIAN_POINT('Ctrl Pts',(-1.69319085004253,-3.11658737782817,
-0.443814152235949));
#49932=CARTESIAN_POINT('Ctrl Pts',(-1.885321005712,-3.00362704783803,-0.450919958514229));
#49933=CARTESIAN_POINT('Ctrl Pts',(-2.25657862337976,-2.73620836477243,
-0.466129897694596));
#49934=CARTESIAN_POINT('Ctrl Pts',(-2.4342404980128,-2.57956481057542,-0.474160506718203));
#49935=CARTESIAN_POINT('Ctrl Pts',(-2.70406189805077,-2.28955596887064,
-0.487792479856233));
#49936=CARTESIAN_POINT('Ctrl Pts',(-2.80544632573569,-2.16466540561564,
-0.49337996726572));
#49937=CARTESIAN_POINT('Ctrl Pts',(-2.99824473911775,-1.8903161208689,-0.504873700329334));
#49938=CARTESIAN_POINT('Ctrl Pts',(-3.08734956143078,-1.74034849548728,
-0.510607146388673));
#49939=CARTESIAN_POINT('Ctrl Pts',(-3.26280650869878,-1.38854699351263,
-0.523458372993033));
#49940=CARTESIAN_POINT('Ctrl Pts',(-3.34246103011777,-1.18313932074248,
-0.530653117795877));
#49941=CARTESIAN_POINT('Ctrl Pts',(-3.51952274767331,-0.564154050130049,
-0.55258135924146));
#49942=CARTESIAN_POINT('Ctrl Pts',(-3.56446029553434,-0.141118654756757,
-0.567315278982563));
#49943=CARTESIAN_POINT('Ctrl Pts',(-3.49980016274106,0.618806706849648,
-0.592438540955659));
#49944=CARTESIAN_POINT('Ctrl Pts',(-3.42730365233934,0.939281313760002,
-0.60307473140123));
#49945=CARTESIAN_POINT('Ctrl Pts',(-3.26608986447908,1.37020091188365,-0.618977520143229));
#49946=CARTESIAN_POINT('Ctrl Pts',(-3.21174510953929,1.49373408262001,-0.623681838734362));
#49947=CARTESIAN_POINT('Ctrl Pts',(-3.04741893366169,1.81570525962115,-0.636158761370165));
#49948=CARTESIAN_POINT('Ctrl Pts',(-2.9257895372206,2.00554947617206,-0.643596937937371));
#49949=CARTESIAN_POINT('Ctrl Pts',(-2.59971973293075,2.42026758161057,-0.660980962533989));
#49950=CARTESIAN_POINT('Ctrl Pts',(-2.38301884184684,2.63344370490353,-0.670916530448369));
#49951=CARTESIAN_POINT('Ctrl Pts',(-2.02680985593994,2.90515541357183,-0.68627707144474));
#49952=CARTESIAN_POINT('Ctrl Pts',(-1.904778192232,2.98691191652053,-0.691416716240337));
#49953=CARTESIAN_POINT('Ctrl Pts',(-1.65582899649891,3.13202153163874,-0.701409064104142));
#49954=CARTESIAN_POINT('Ctrl Pts',(-1.52943609357706,3.19578772470759,-0.706229864017868));
#49955=CARTESIAN_POINT('Ctrl Pts',(-1.2247541139607,3.32652713538526,-0.717189889421697));
#49956=CARTESIAN_POINT('Ctrl Pts',(-1.04459023891923,3.38699095830953,-0.723323530969576));
#49957=CARTESIAN_POINT('Ctrl Pts',(-0.703648151102374,3.47206498648711,
-0.734996960808483));
#49958=CARTESIAN_POINT('Ctrl Pts',(-0.54381980803693,3.50061073469892,-0.7404478038163));
#49959=CARTESIAN_POINT('Ctrl Pts',(-0.201816646292843,3.53808128149046,
-0.75216257198571));
#49960=CARTESIAN_POINT('Ctrl Pts',(-0.0192726672086005,3.54413123318279,
-0.758464403158838));
#49961=CARTESIAN_POINT('Ctrl Pts',(0.279013422284102,3.53083955973339,-0.768819141221532));
#49962=CARTESIAN_POINT('Ctrl Pts',(0.395202241640959,3.51985650823388,-0.772836829640794));
#49963=CARTESIAN_POINT('Ctrl Pts',(0.715918597103892,3.47290766543585,-0.783688019912121));
#49964=CARTESIAN_POINT('Ctrl Pts',(0.918166422680317,3.42449853694842,-0.790336205147484));
#49965=CARTESIAN_POINT('Ctrl Pts',(1.4060534825555,3.26194416863173,-0.807309072604764));
#49966=CARTESIAN_POINT('Ctrl Pts',(1.6850516524377,3.12729642735548,-0.817931124258926));
#49967=CARTESIAN_POINT('Ctrl Pts',(2.11188424682707,2.84815909807049,-0.835521831524876));
#49968=CARTESIAN_POINT('Ctrl Pts',(2.27163940152376,2.72279877301433,-0.842487526307453));
#49969=CARTESIAN_POINT('Ctrl Pts',(2.56828037414233,2.44417699117511,-0.855978783114457));
#49970=CARTESIAN_POINT('Ctrl Pts',(2.70409644770606,2.29234856385226,-0.862545586637578));
#49971=CARTESIAN_POINT('Ctrl Pts',(2.9783319322613,1.92792828456862,-0.877658875229771));
#49972=CARTESIAN_POINT('Ctrl Pts',(3.10917461242445,1.70948764113348,-0.88644525581145));
#49973=CARTESIAN_POINT('Ctrl Pts',(3.28156155473456,1.33648233396227,-0.900674479468243));
#49974=CARTESIAN_POINT('Ctrl Pts',(3.33827373145222,1.18862719992309,-0.906118956223986));
#49975=CARTESIAN_POINT('Ctrl Pts',(3.46604468842926,0.771341027127037,-0.920739709652885));
#49976=CARTESIAN_POINT('Ctrl Pts',(3.5152914165801,0.495653409739684,-0.92976852882634));
#49977=CARTESIAN_POINT('Ctrl Pts',(3.54713653941856,-0.0251639221401792,
-0.947125291843253));
#49978=CARTESIAN_POINT('Ctrl Pts',(3.53724452475388,-0.269969014214833,
-0.955525192271259));
#49979=CARTESIAN_POINT('Ctrl Pts',(3.47766425068042,-0.682888166898913,
-0.970034433472272));
#49980=CARTESIAN_POINT('Ctrl Pts',(3.44021364964715,-0.853007512381875,
-0.976029608802391));
#49981=CARTESIAN_POINT('Ctrl Pts',(3.3603394377886,-1.11773024116344,-0.985196670383434));
#49982=CARTESIAN_POINT('Ctrl Pts',(3.32660260203798,-1.2139929586542,-0.988524242567791));
#49983=CARTESIAN_POINT('Ctrl Pts',(3.16270045761105,-1.62398848765727,-1.00303684624274));
#49984=CARTESIAN_POINT('Ctrl Pts',(2.99112197174943,-1.9213472066483,-1.01437016184374));
#49985=CARTESIAN_POINT('Ctrl Pts',(2.71916743299541,-2.26801202614191,-1.02956577508448));
#49986=CARTESIAN_POINT('Ctrl Pts',(2.65345479161002,-2.34482230175402,-1.03309011572484));
#49987=CARTESIAN_POINT('Ctrl Pts',(2.51938354394797,-2.48850592178276,-1.03991233786383));
#49988=CARTESIAN_POINT('Ctrl Pts',(2.45136413252933,-2.55568782031447,-1.04320973142055));
#49989=CARTESIAN_POINT('Ctrl Pts',(2.30984422638263,-2.68428307531518,-1.04966261566972));
#49990=CARTESIAN_POINT('Ctrl Pts',(2.23634923922314,-2.74567398495228,-1.05281737552517));
#49991=CARTESIAN_POINT('Ctrl Pts',(2.03215211779958,-2.90253737468983,-1.06124771713154));
#49992=CARTESIAN_POINT('Ctrl Pts',(1.89702757004923,-2.9922375826466,-1.06650485891362));
#49993=CARTESIAN_POINT('Ctrl Pts',(1.5646930096777,-3.18182032056654,-1.07925869521061));
#49994=CARTESIAN_POINT('Ctrl Pts',(1.36273027274016,-3.27353529473883,-1.08679861770155));
#49995=CARTESIAN_POINT('Ctrl Pts',(0.945261046853487,-3.41821874298324,
-1.10200645884336));
#49996=CARTESIAN_POINT('Ctrl Pts',(0.729224280881415,-3.47132276863424,
-1.10976827570799));
#49997=CARTESIAN_POINT('Ctrl Pts',(0.382914472640594,-3.52143416142455,
-1.12149300683948));
#49998=CARTESIAN_POINT('Ctrl Pts',(0.255792931202741,-3.53272173764504,
-1.12566442134657));
#49999=CARTESIAN_POINT('Ctrl Pts',(-0.113062510410115,-3.54552346686426,
-1.1377289345704));
#50000=CARTESIAN_POINT('Ctrl Pts',(-0.355466351724561,-3.52922066711232,
-1.1457225507509));
#50001=CARTESIAN_POINT('Ctrl Pts',(-0.871408743345329,-3.44181384528943,
-1.16366965067737));
#50002=CARTESIAN_POINT('Ctrl Pts',(-1.25970345812106,-3.34412341778873,
-1.17754107965305));
#50003=CARTESIAN_POINT('Ctrl Pts',(-1.96907530071397,-2.95845149470074,
-1.20416008647879));
#50004=CARTESIAN_POINT('Ctrl Pts',(-2.23116543632206,-2.76560410716815,
-1.21467297486572));
#50005=CARTESIAN_POINT('Ctrl Pts',(-2.67889924966404,-2.3327143711385,-1.23617432834315));
#50006=CARTESIAN_POINT('Ctrl Pts',(-2.86897605883321,-2.09628119776566,
-1.24672137384146));
#50007=CARTESIAN_POINT('Ctrl Pts',(-3.23973759783859,-1.48375590216976,
-1.27035024270255));
#50008=CARTESIAN_POINT('Ctrl Pts',(-3.3907973744537,-1.09307272587653,-1.28385141224157));
#50009=CARTESIAN_POINT('Ctrl Pts',(-3.52039460900459,-0.444742011367405,
-1.30674376705023));
#50010=CARTESIAN_POINT('Ctrl Pts',(-3.54367240627609,-0.195348451110837,
-1.31550126057737));
#50011=CARTESIAN_POINT('Ctrl Pts',(-3.53684555370509,0.212912125235389,
-1.32897516991721));
#50012=CARTESIAN_POINT('Ctrl Pts',(-3.52355723814933,0.370013095177801,
-1.33406889946687));
#50013=CARTESIAN_POINT('Ctrl Pts',(-3.44969917731903,0.857382716286607,
-1.35037352970638));
#50014=CARTESIAN_POINT('Ctrl Pts',(-3.35257804579177,1.18233803551094,-1.36182222496779));
#50015=CARTESIAN_POINT('Ctrl Pts',(-3.13714253384444,1.64961323241961,-1.37965155151134));
#50016=CARTESIAN_POINT('Ctrl Pts',(-3.04995817443986,1.80621222613115,-1.38584433097576));
#50017=CARTESIAN_POINT('Ctrl Pts',(-2.86678237182935,2.08189311977124,-1.39681812337178));
#50018=CARTESIAN_POINT('Ctrl Pts',(-2.77501506247927,2.20224713487007,-1.40170864192018));
#50019=CARTESIAN_POINT('Ctrl Pts',(-2.52332435703554,2.4922024096765,-1.41429807105808));
#50020=CARTESIAN_POINT('Ctrl Pts',(-2.3533714407419,2.65319226270889,-1.42219795278603));
#50021=CARTESIAN_POINT('Ctrl Pts',(-1.94386074828543,2.97168356561673,-1.44004191719084));
#50022=CARTESIAN_POINT('Ctrl Pts',(-1.61491480619346,3.18591725044698,-1.45353899697759));
#50023=CARTESIAN_POINT('Ctrl Pts',(-0.931878180439088,3.42331584633322,
-1.47725256485255));
#50024=CARTESIAN_POINT('Ctrl Pts',(-0.687664090142368,3.48031865812463,
-1.48542548426783));
#50025=CARTESIAN_POINT('Ctrl Pts',(-0.23381657008611,3.53756006465768,-1.5011152849445));
#50026=CARTESIAN_POINT('Ctrl Pts',(-0.0250415350069334,3.54563700299522,
-1.50841344094553));
#50027=CARTESIAN_POINT('Ctrl Pts',(0.393004384983738,3.52452247866436,-1.52275874360842));
#50028=CARTESIAN_POINT('Ctrl Pts',(0.600418503567333,3.49485515022846,-1.52965062013704));
#50029=CARTESIAN_POINT('Ctrl Pts',(1.09736162060221,3.37808155014134,-1.54646887836633));
#50030=CARTESIAN_POINT('Ctrl Pts',(1.38189734762745,3.27171292848107,-1.55637931072981));
#50031=CARTESIAN_POINT('Ctrl Pts',(1.83090116723113,3.03603789251927,-1.57387390694066));
#50032=CARTESIAN_POINT('Ctrl Pts',(2.00495491799037,2.92459539548152,-1.5811428566297));
#50033=CARTESIAN_POINT('Ctrl Pts',(2.26124338011125,2.72628632279553,-1.59214069984753));
#50034=CARTESIAN_POINT('Ctrl Pts',(2.35063802083803,2.6494228731033,-1.59601970029676));
#50035=CARTESIAN_POINT('Ctrl Pts',(2.56968967832108,2.44106535281573,-1.60593120010558));
#50036=CARTESIAN_POINT('Ctrl Pts',(2.69343555017507,2.30325658977076,-1.612006418483));
#50037=CARTESIAN_POINT('Ctrl Pts',(2.90788195749299,2.02387010049144,-1.62377075774636));
#50038=CARTESIAN_POINT('Ctrl Pts',(3.00061309371375,1.88377651487001,-1.62943608992525));
#50039=CARTESIAN_POINT('Ctrl Pts',(3.18893853513039,1.55064596016399,-1.64255846538333));
#50040=CARTESIAN_POINT('Ctrl Pts',(3.27789892378502,1.35382466996276,-1.65016296159083));
#50041=CARTESIAN_POINT('Ctrl Pts',(3.38230914293851,1.05022243547603,-1.6610576833713));
#50042=CARTESIAN_POINT('Ctrl Pts',(3.41206848626365,0.948630213858275,-1.66455192322864));
#50043=CARTESIAN_POINT('Ctrl Pts',(3.47298243877771,0.699597302697179,-1.67294935037395));
#50044=CARTESIAN_POINT('Ctrl Pts',(3.4993656521765,0.550889227730839,-1.67783645953324));
#50045=CARTESIAN_POINT('Ctrl Pts',(3.53894438372914,0.200661876798343,-1.68954796717138));
#50046=CARTESIAN_POINT('Ctrl Pts',(3.54466152137657,-0.00176295551019043,
-1.69641644230088));
#50047=CARTESIAN_POINT('Ctrl Pts',(3.51829273772974,-0.470493168757712,
-1.71254294048661));
#50048=CARTESIAN_POINT('Ctrl Pts',(3.47318172667174,-0.736754365994446,
-1.72196428124109));
#50049=CARTESIAN_POINT('Ctrl Pts',(3.35537223945156,-1.1373018398422,-1.73588382755945));
#50050=CARTESIAN_POINT('Ctrl Pts',(3.30479181397498,-1.27604640284775,-1.74068350078129));
#50051=CARTESIAN_POINT('Ctrl Pts',(3.16718492377856,-1.5912926594912,-1.7519417711377));
#50052=CARTESIAN_POINT('Ctrl Pts',(3.07361638980968,-1.76497580390325,-1.75848191075209));
#50053=CARTESIAN_POINT('Ctrl Pts',(2.84022721222543,-2.12424226662904,-1.77315559437722));
#50054=CARTESIAN_POINT('Ctrl Pts',(2.69505456286334,-2.30646539287088,-1.78126768471401));
#50055=CARTESIAN_POINT('Ctrl Pts',(2.37886712768591,-2.63106917496356,-1.79674409493971));
#50056=CARTESIAN_POINT('Ctrl Pts',(2.21036711097651,-2.7735214089575,-1.80399408546808));
#50057=CARTESIAN_POINT('Ctrl Pts',(1.84475102259879,-3.02869423119426,-1.81865031742086));
#50058=CARTESIAN_POINT('Ctrl Pts',(1.64685580303852,-3.14046009135748,-1.82608516870827));
#50059=CARTESIAN_POINT('Ctrl Pts',(1.30211229096659,-3.29435184719581,-1.83898859470103));
#50060=CARTESIAN_POINT('Ctrl Pts',(1.15999346675071,-3.34730451232009,-1.84427863704171));
#50061=CARTESIAN_POINT('Ctrl Pts',(0.86236200010171,-3.43691606068077,-1.8550635325919));
#50062=CARTESIAN_POINT('Ctrl Pts',(0.70641438115456,-3.47258240326183,-1.86054104982383));
#50063=CARTESIAN_POINT('Ctrl Pts',(0.38245767886815,-3.52311089768784,-1.87141869044349));
#50064=CARTESIAN_POINT('Ctrl Pts',(0.215109285174395,-3.53692867125598,
-1.87689259850194));
#50065=CARTESIAN_POINT('Ctrl Pts',(-0.17080281501418,-3.54157104116341,
-1.88964570117501));
#50066=CARTESIAN_POINT('Ctrl Pts',(-0.389521567696692,-3.52412842824805,
-1.89693106052957));
#50067=CARTESIAN_POINT('Ctrl Pts',(-0.81192126987469,-3.45129306028026,
-1.91157065871698));
#50068=CARTESIAN_POINT('Ctrl Pts',(-1.01593935698251,-3.3973397238017,-1.91899733085867));
#50069=CARTESIAN_POINT('Ctrl Pts',(-1.37277482230161,-3.26748271910123,
-1.9320158250549));
#50070=CARTESIAN_POINT('Ctrl Pts',(-1.52685384876056,-3.19811464000463,
-1.93755148215728));
#50071=CARTESIAN_POINT('Ctrl Pts',(-1.94098593117999,-2.97477489628643,
-1.95292816354384));
#50072=CARTESIAN_POINT('Ctrl Pts',(-2.18841907487769,-2.7973238359502,-1.96302478119542));
#50073=CARTESIAN_POINT('Ctrl Pts',(-2.56405122407262,-2.44884668828753,
-1.98055727133914));
#50074=CARTESIAN_POINT('Ctrl Pts',(-2.70574308030546,-2.2920728130192,-1.98791057288492));
#50075=CARTESIAN_POINT('Ctrl Pts',(-2.93393460083031,-1.9881997954724,-2.00093313990393));
#50076=CARTESIAN_POINT('Ctrl Pts',(-3.0251948995756,-1.84580897732215,-2.00648843180739));
#50077=CARTESIAN_POINT('Ctrl Pts',(-3.22369794631868,-1.48125161922904,
-2.02004049934766));
#50078=CARTESIAN_POINT('Ctrl Pts',(-3.31897013566167,-1.25234888004105,
-2.02816089470863));
#50079=CARTESIAN_POINT('Ctrl Pts',(-3.51045751553196,-0.614887926350445,
-2.05091020117093));
#50080=CARTESIAN_POINT('Ctrl Pts',(-3.55967612642411,-0.202806351969069,
-2.06524896687874));
#50081=CARTESIAN_POINT('Ctrl Pts',(-3.52443018549891,0.351738831399751,
-2.08353960608183));
#50082=CARTESIAN_POINT('Ctrl Pts',(-3.50852296577055,0.483805038134683,
-2.08788020965693));
#50083=CARTESIAN_POINT('Ctrl Pts',(-3.48534270679742,0.614574670841336,
-2.09226952931372));
#50084=CARTESIAN_POINT('Ctrl Pts',(-3.93889502759575,0.69454040892368,-1.60816409353334));
#50085=CARTESIAN_POINT('Ctrl Pts',(-4.00744659720704,0.306810047460087,
-1.5964556824165));
#50086=CARTESIAN_POINT('Ctrl Pts',(-4.01838996798143,-0.0875683989890832,
-1.58502986037042));
#50087=CARTESIAN_POINT('Ctrl Pts',(-3.92470336328846,-0.861748316404742,
-1.56143896080034));
#50088=CARTESIAN_POINT('Ctrl Pts',(-3.82291771735831,-1.23664973539996,
-1.54999044876737));
#50089=CARTESIAN_POINT('Ctrl Pts',(-3.4330291644234,-2.13834145427003,-1.52095445657165));
#50090=CARTESIAN_POINT('Ctrl Pts',(-3.11045881151132,-2.54889752466793,
-1.50542478621335));
#50091=CARTESIAN_POINT('Ctrl Pts',(-2.63260132188013,-3.02171102766451,
-1.48532088310118));
#50092=CARTESIAN_POINT('Ctrl Pts',(-2.43650516808078,-3.18208186762214,
-1.47792778043916));
#50093=CARTESIAN_POINT('Ctrl Pts',(-2.0173198756678,-3.46319653213006,-1.46302039289925));
#50094=CARTESIAN_POINT('Ctrl Pts',(-1.79626338874197,-3.58272324890874,
-1.45544555299358));
#50095=CARTESIAN_POINT('Ctrl Pts',(-1.10823337490155,-3.87482660455011,
-1.43288939965075));
#50096=CARTESIAN_POINT('Ctrl Pts',(-0.584632652053741,-3.99691429971845,
-1.41746240937877));
#50097=CARTESIAN_POINT('Ctrl Pts',(0.233830615342959,-4.00127063912057,
-1.39303362854051));
#50098=CARTESIAN_POINT('Ctrl Pts',(0.490201285660078,-3.97777504144854,
-1.3852446142734));
#50099=CARTESIAN_POINT('Ctrl Pts',(0.995938468358567,-3.88222301582721,
-1.36976301914108));
#50100=CARTESIAN_POINT('Ctrl Pts',(1.24415481848043,-3.80995446145941,-1.36217322692837));
#50101=CARTESIAN_POINT('Ctrl Pts',(2.01616276652598,-3.50202694919009,-1.33766738862933));
#50102=CARTESIAN_POINT('Ctrl Pts',(2.44508081081143,-3.1987775444315,-1.32196010534453));
#50103=CARTESIAN_POINT('Ctrl Pts',(3.01090964362374,-2.65254240525115,-1.29850917321391));
#50104=CARTESIAN_POINT('Ctrl Pts',(3.21562175227277,-2.40092461921334,-1.28910836238346));
#50105=CARTESIAN_POINT('Ctrl Pts',(3.51776457715512,-1.91951785534438,-1.27214083111131));
#50106=CARTESIAN_POINT('Ctrl Pts',(3.62874538995318,-1.70001972408149,-1.26467049496387));
#50107=CARTESIAN_POINT('Ctrl Pts',(3.81427530798883,-1.23099921631057,-1.24950266268962));
#50108=CARTESIAN_POINT('Ctrl Pts',(3.88616447441406,-0.980605275840849,
-1.24185379598605));
#50109=CARTESIAN_POINT('Ctrl Pts',(4.04000254950994,-0.149723695797231,
-1.21688850567111));
#50110=CARTESIAN_POINT('Ctrl Pts',(4.00632467612848,0.370910426850598,-1.2013571473354));
#50111=CARTESIAN_POINT('Ctrl Pts',(3.86806721181153,1.04847228431323,-1.18068049877335));
#50112=CARTESIAN_POINT('Ctrl Pts',(3.79419777707799,1.29091995395088,-1.17327277042335));
#50113=CARTESIAN_POINT('Ctrl Pts',(3.60137912405081,1.75898868775722,-1.15832902502366));
#50114=CARTESIAN_POINT('Ctrl Pts',(3.48294709266645,1.98293492001914,-1.15069862141123));
#50115=CARTESIAN_POINT('Ctrl Pts',(3.0548197047919,2.63486504159509,-1.12714149943802));
#50116=CARTESIAN_POINT('Ctrl Pts',(2.67806842243565,3.01824425671164,-1.11173986731942));
#50117=CARTESIAN_POINT('Ctrl Pts',(2.02555902554214,3.45869156667143,-1.08823174530743));
#50118=CARTESIAN_POINT('Ctrl Pts',(1.79821101280998,3.58188217699888,-1.08041935974421));
#50119=CARTESIAN_POINT('Ctrl Pts',(1.32350112298141,3.78308453313687,-1.06491464450448));
#50120=CARTESIAN_POINT('Ctrl Pts',(1.07699975502504,3.86055113598766,-1.05732128114226));
#50121=CARTESIAN_POINT('Ctrl Pts',(0.270034970633146,4.03099324476181,-1.03301716956992));
#50122=CARTESIAN_POINT('Ctrl Pts',(-0.25521342163276,4.01927379572924,-1.01728840247899));
#50123=CARTESIAN_POINT('Ctrl Pts',(-0.969575955830072,3.88857553975101,
-0.995653688585681));
#50124=CARTESIAN_POINT('Ctrl Pts',(-1.2141204936574,3.81960306062729,-0.988196368037047));
#50125=CARTESIAN_POINT('Ctrl Pts',(-1.69005956293143,3.6345359373705,-0.973099649565625));
#50126=CARTESIAN_POINT('Ctrl Pts',(-1.91982443837823,3.51828148267251,-0.96534187309345));
#50127=CARTESIAN_POINT('Ctrl Pts',(-2.56734407205033,3.10884896953529,-0.942197836812912));
#50128=CARTESIAN_POINT('Ctrl Pts',(-2.94375611537857,2.75583749190019,-0.927474923905979));
#50129=CARTESIAN_POINT('Ctrl Pts',(-3.39474632506785,2.13146138471936,-0.904363755701564));
#50130=CARTESIAN_POINT('Ctrl Pts',(-3.52633862076298,1.90518052615191,-0.896498084751868));
#50131=CARTESIAN_POINT('Ctrl Pts',(-3.81701733888187,1.27167726524321,-0.875595295234326));
#50132=CARTESIAN_POINT('Ctrl Pts',(-3.93378242934524,0.8470632461161,-0.862985144367765));
#50133=CARTESIAN_POINT('Ctrl Pts',(-4.00531037533674,0.153415730762649,
-0.842014391062206));
#50134=CARTESIAN_POINT('Ctrl Pts',(-4.00669128945411,-0.106473790668588,
-0.834139140561101));
#50135=CARTESIAN_POINT('Ctrl Pts',(-3.95923793090611,-0.622498168961368,
-0.818673884785553));
#50136=CARTESIAN_POINT('Ctrl Pts',(-3.91077151366751,-0.87757469121337,
-0.811047443675081));
#50137=CARTESIAN_POINT('Ctrl Pts',(-3.67021024045104,-1.69994920328026,
-0.785678417398851));
#50138=CARTESIAN_POINT('Ctrl Pts',(-3.39667285554584,-2.1567657173322,-0.769744977442529));
#50139=CARTESIAN_POINT('Ctrl Pts',(-2.98848117293989,-2.66694605409314,
-0.750359967163677));
#50140=CARTESIAN_POINT('Ctrl Pts',(-2.84110394956172,-2.82358937989018,
-0.744090090057257));
#50141=CARTESIAN_POINT('Ctrl Pts',(-2.27902931600789,-3.33202863984671,
-0.721634326703568));
#50142=CARTESIAN_POINT('Ctrl Pts',(-1.84441618373233,-3.5758310320697,-0.706666416766861));
#50143=CARTESIAN_POINT('Ctrl Pts',(-1.19187027314479,-3.8268756418652,-0.685908318678602));
#50144=CARTESIAN_POINT('Ctrl Pts',(-0.940807050262362,-3.8965071798302,
-0.67830414500068));
#50145=CARTESIAN_POINT('Ctrl Pts',(-0.424690974184233,-3.9860202103712,
-0.662684597705209));
#50146=CARTESIAN_POINT('Ctrl Pts',(-0.160507741240573,-4.00514503561195,
-0.654654677364008));
#50147=CARTESIAN_POINT('Ctrl Pts',(0.575348473826228,-3.98607260123649,
-0.632522882400995));
#50148=CARTESIAN_POINT('Ctrl Pts',(1.08945400304019,-3.88946270876767,-0.61759417931966));
#50149=CARTESIAN_POINT('Ctrl Pts',(1.83869836786569,-3.56143102383145,-0.592975290336023));
#50150=CARTESIAN_POINT('Ctrl Pts',(2.06544258583032,-3.43467463037156,-0.585192721734639));
#50151=CARTESIAN_POINT('Ctrl Pts',(2.49249938480152,-3.13890819007588,-0.569691014274639));
#50152=CARTESIAN_POINT('Ctrl Pts',(2.69195657236367,-2.96992092695915,-0.562052898386223));
#50153=CARTESIAN_POINT('Ctrl Pts',(3.23006954478627,-2.41445773272655,-0.539181057923025));
#50154=CARTESIAN_POINT('Ctrl Pts',(3.51185084512747,-1.98068495502258,-0.52360957978045));
#50155=CARTESIAN_POINT('Ctrl Pts',(3.80248490305767,-1.26750730703816,-0.500829955845552));
#50156=CARTESIAN_POINT('Ctrl Pts',(3.87729712792385,-1.01744142158655,-0.493164240787644));
#50157=CARTESIAN_POINT('Ctrl Pts',(4.02178703311848,-0.270710889804952,
-0.470391292799232));
#50158=CARTESIAN_POINT('Ctrl Pts',(4.02404060158649,0.236036749392638,-0.455308717844116));
#50159=CARTESIAN_POINT('Ctrl Pts',(3.83723046698998,1.24543408126294,-0.425085309954019));
#50160=CARTESIAN_POINT('Ctrl Pts',(3.6410761923079,1.73528978493034,-0.409267017824708));
#50161=CARTESIAN_POINT('Ctrl Pts',(3.21563842321284,2.39261837548403,-0.385980583765538));
#50162=CARTESIAN_POINT('Ctrl Pts',(3.05262614733734,2.59791809202657,-0.378282010147998));
#50163=CARTESIAN_POINT('Ctrl Pts',(2.51419179749808,3.1530225884133,-0.355374898172946));
#50164=CARTESIAN_POINT('Ctrl Pts',(2.08897578758717,3.448816708814,-0.339775101775347));
#50165=CARTESIAN_POINT('Ctrl Pts',(1.38576623163163,3.76087087273643,-0.317085552566121));
#50166=CARTESIAN_POINT('Ctrl Pts',(1.1403400596281,3.8427213320877,-0.309499971617901));
#50167=CARTESIAN_POINT('Ctrl Pts',(0.640302589479629,3.95652511673326,-0.294066596827899));
#50168=CARTESIAN_POINT('Ctrl Pts',(0.387035608816613,3.98894608798221,-0.286398346866338));
#50169=CARTESIAN_POINT('Ctrl Pts',(-0.387353382741609,4.01460566729674,
-0.263207054571433));
#50170=CARTESIAN_POINT('Ctrl Pts',(-0.906894917014024,3.93085568448703,
-0.248159509078221));
#50171=CARTESIAN_POINT('Ctrl Pts',(-1.63898710819294,3.65756660871905,-0.224527674913839));
#50172=CARTESIAN_POINT('Ctrl Pts',(-1.87140434482678,3.54415532691843,-0.216784792169306));
#50173=CARTESIAN_POINT('Ctrl Pts',(-2.31212015321213,3.27387546319818,-0.201467507015652));
#50174=CARTESIAN_POINT('Ctrl Pts',(-2.51975552530336,3.11724623449951,-0.193856165457704));
#50175=CARTESIAN_POINT('Ctrl Pts',(-3.08001951418731,2.60137486340935,-0.171158479958212));
#50176=CARTESIAN_POINT('Ctrl Pts',(-3.38288713508128,2.1917199886369,-0.155880597428147));
#50177=CARTESIAN_POINT('Ctrl Pts',(-3.71095897582277,1.51361027607746,-0.133659141724757));
#50178=CARTESIAN_POINT('Ctrl Pts',(-3.79931632169689,1.27633127684376,-0.126271130958857));
#50179=CARTESIAN_POINT('Ctrl Pts',(-3.92575395302178,0.80241628054708,-0.111502977965752));
#50180=CARTESIAN_POINT('Ctrl Pts',(-3.96631179397013,0.56790459229602,-0.104302357156274));
#50181=CARTESIAN_POINT('Ctrl Pts',(-4.02113745954231,-0.095459444094893,
-0.0844081710650721));
#50182=CARTESIAN_POINT('Ctrl Pts',(-3.99676192186721,-0.62281133824077,
-0.0693130354409824));
#50183=CARTESIAN_POINT('Ctrl Pts',(-3.7320206379447,-1.46609048049094,-0.042674421078045));
#50184=CARTESIAN_POINT('Ctrl Pts',(-3.61863802768239,-1.72709802725838,
-0.034100228204948));
#50185=CARTESIAN_POINT('Ctrl Pts',(-3.33597966896508,-2.22537714393393,
-0.0171317201591535));
#50186=CARTESIAN_POINT('Ctrl Pts',(-3.16619428328731,-2.46144472839372,
-0.00869672167633724));
#50187=CARTESIAN_POINT('Ctrl Pts',(-2.97253925539568,-2.67651731155686,
-1.42199285337063E-5));
#50188=CARTESIAN_POINT('Ctrl Pts',(3.987069663918,0.522679131849,0.3152898013535));
#50189=CARTESIAN_POINT('Ctrl Pts',(4.075962269058,-0.1554061172176,0.2949890614009));
#50190=CARTESIAN_POINT('Ctrl Pts',(3.900091378894,-1.557010834613,0.2543875814958));
#50191=CARTESIAN_POINT('Ctrl Pts',(2.642948825861,-3.263519409944,0.193485361638));
#50192=CARTESIAN_POINT('Ctrl Pts',(0.7125717312084,-4.138558721235,0.1325831417803));
#50193=CARTESIAN_POINT('Ctrl Pts',(-1.399304475191,-3.959477965926,0.07168092192261));
#50194=CARTESIAN_POINT('Ctrl Pts',(-3.154752699231,-2.771828540526,0.01077870206489));
#50195=CARTESIAN_POINT('Ctrl Pts',(-4.106624282706,-0.8781447135099,-0.05012351779283));
#50196=CARTESIAN_POINT('Ctrl Pts',(-4.01245983409,1.23922042509,-0.1110257376505));
#50197=CARTESIAN_POINT('Ctrl Pts',(-2.896244687669,3.040932036188,-0.1719279575083));
#50198=CARTESIAN_POINT('Ctrl Pts',(-1.042300344905,4.068059861997,-0.232830177366));
#50199=CARTESIAN_POINT('Ctrl Pts',(1.077137937534,4.058974609329,-0.2937323972237));
#50200=CARTESIAN_POINT('Ctrl Pts',(2.922208477455,3.015990490368,-0.3546346170814));
#50201=CARTESIAN_POINT('Ctrl Pts',(4.022936335639,1.204775606403,-0.4155368369391));
#50202=CARTESIAN_POINT('Ctrl Pts',(4.098944963669,-0.9133187873028,-0.4764390567969));
#50203=CARTESIAN_POINT('Ctrl Pts',(3.130873502694,-2.798773326411,-0.5373412766546));
#50204=CARTESIAN_POINT('Ctrl Pts',(1.365308366059,-3.97132648973,-0.5982434965123));
#50205=CARTESIAN_POINT('Ctrl Pts',(-0.7480270609807,-4.132306442959,-0.65914571637));
#50206=CARTESIAN_POINT('Ctrl Pts',(-2.670825613937,-3.24070849698,-0.7200479362277));
#50207=CARTESIAN_POINT('Ctrl Pts',(-3.913313533437,-1.523639790607,-0.7809501560854));
#50208=CARTESIAN_POINT('Ctrl Pts',(-4.159005258158,0.5815292641248,-0.8418523759432));
#50209=CARTESIAN_POINT('Ctrl Pts',(-3.345318382176,2.538571634652,-0.9027545958009));
#50210=CARTESIAN_POINT('Ctrl Pts',(-1.679514596622,3.848991003293,-0.9636568156586));
#50211=CARTESIAN_POINT('Ctrl Pts',(0.4140938465922,4.178998361075,-1.024559035516));
#50212=CARTESIAN_POINT('Ctrl Pts',(2.402224628031,3.444534494857,-1.085461255374));
#50213=CARTESIAN_POINT('Ctrl Pts',(3.778462602443,1.832681451182,-1.146363475232));
#50214=CARTESIAN_POINT('Ctrl Pts',(4.192253539827,-0.2459907314392,-1.207265695089));
#50215=CARTESIAN_POINT('Ctrl Pts',(3.538196776895,-2.26200457673,-1.268167914947));
#50216=CARTESIAN_POINT('Ctrl Pts',(1.98289372813,-3.701841503134,-1.329070134805));
#50217=CARTESIAN_POINT('Ctrl Pts',(-0.07749218955726,-4.198751449836,-1.389972354663));
#50218=CARTESIAN_POINT('Ctrl Pts',(-2.118132963563,-3.626146647599,-1.45087457452));
#50219=CARTESIAN_POINT('Ctrl Pts',(-3.619268407771,-2.129937470376,-1.511776794378));
#50220=CARTESIAN_POINT('Ctrl Pts',(-4.198417559268,-0.09102472662167,-1.572679014236));
#50221=CARTESIAN_POINT('Ctrl Pts',(-3.871793425676,1.283290749965,-1.613280494141));
#50222=CARTESIAN_POINT('Ctrl Pts',(-3.550837736248,1.887185563384,-1.633581234094));
#50223=CARTESIAN_POINT('Ctrl Pts',(3.821034517157,0.5009129943895,0.2186091678224));
#50224=CARTESIAN_POINT('Ctrl Pts',(3.906225331763,-0.1489344777293,0.1983084278698));
#50225=CARTESIAN_POINT('Ctrl Pts',(3.737678303863,-1.492171605749,0.1577069479647));
#50226=CARTESIAN_POINT('Ctrl Pts',(2.532887444151,-3.127615357629,0.09680472810694));
#50227=CARTESIAN_POINT('Ctrl Pts',(0.6828978198043,-3.966215054687,0.03590250824922));
#50228=CARTESIAN_POINT('Ctrl Pts',(-1.341032675728,-3.794591831349,-0.0249997116085));
#50229=CARTESIAN_POINT('Ctrl Pts',(-3.023378062828,-2.656400168986,-0.08590193146621));
#50230=CARTESIAN_POINT('Ctrl Pts',(-3.935610474836,-0.8415757797628,-0.1468041513239));
#50231=CARTESIAN_POINT('Ctrl Pts',(-3.845367354253,1.187615070157,-0.2077063711817));
#50232=CARTESIAN_POINT('Ctrl Pts',(-2.775635204438,2.914297279467,-0.2686085910394));
#50233=CARTESIAN_POINT('Ctrl Pts',(-0.9988954121289,3.898652007819,-0.3295108108971));
#50234=CARTESIAN_POINT('Ctrl Pts',(1.032282248867,3.889945095985,-0.3904130307548));
#50235=CARTESIAN_POINT('Ctrl Pts',(2.800517773675,2.890394384479,-0.4513152506125));
#50236=CARTESIAN_POINT('Ctrl Pts',(3.855407578631,1.154604650919,-0.5122174704702));
#50237=CARTESIAN_POINT('Ctrl Pts',(3.928250948771,-0.8752850854435,-0.573119690328));
#50238=CARTESIAN_POINT('Ctrl Pts',(3.000493277283,-2.682222882307,-0.6340219101857));
#50239=CARTESIAN_POINT('Ctrl Pts',(1.308452280251,-3.805946942308,-0.6949241300434));
#50240=CARTESIAN_POINT('Ctrl Pts',(-0.7168766690086,-3.960223142552,-0.7558263499011));
#50241=CARTESIAN_POINT('Ctrl Pts',(-2.559603347921,-3.105754368695,-0.8167285697588));
#50242=CARTESIAN_POINT('Ctrl Pts',(-3.750349842903,-1.46019024556,-0.8776307896166));
#50243=CARTESIAN_POINT('Ctrl Pts',(-3.985810128244,0.5573124069205,-0.9385330094743));
#50244=CARTESIAN_POINT('Ctrl Pts',(-3.206007942338,2.432856874326,-0.999435229332));
#50245=CARTESIAN_POINT('Ctrl Pts',(-1.609573894291,3.688705921772,-1.06033744919));
#50246=CARTESIAN_POINT('Ctrl Pts',(0.3968495698709,4.004970650329,-1.121239669047));
#50247=CARTESIAN_POINT('Ctrl Pts',(2.30218782098,3.301092358505,-1.182141888905));
#50248=CARTESIAN_POINT('Ctrl Pts',(3.621114563505,1.756362359879,-1.243044108763));
#50249=CARTESIAN_POINT('Ctrl Pts',(4.017673838337,-0.2357468404016,-1.303946328621));
#50250=CARTESIAN_POINT('Ctrl Pts',(3.390854224434,-2.167807009712,-1.364848548478));
#50251=CARTESIAN_POINT('Ctrl Pts',(1.90031928652,-3.547684227473,-1.425750768336));
#50252=CARTESIAN_POINT('Ctrl Pts',(-0.07426515111787,-4.023901153264,-1.486652988194));
#50253=CARTESIAN_POINT('Ctrl Pts',(-2.029926700038,-3.475141563274,-1.547555208051));
#50254=CARTESIAN_POINT('Ctrl Pts',(-3.468549756755,-2.041239627024,-1.608457427909));
#50255=CARTESIAN_POINT('Ctrl Pts',(-4.023581167035,-0.08723414729463,-1.669359647767));
#50256=CARTESIAN_POINT('Ctrl Pts',(-3.710558773701,1.229850156756,-1.709961127672));
#50257=CARTESIAN_POINT('Ctrl Pts',(-3.402968771228,1.808596735399,-1.730261867625));
#50258=CARTESIAN_POINT('Ctrl Pts',(3.654999370396,0.4791468569299,0.1219285342913));
#50259=CARTESIAN_POINT('Ctrl Pts',(3.736488394468,-0.1424628382409,0.1016277943387));
#50260=CARTESIAN_POINT('Ctrl Pts',(3.575265228833,-1.427332376886,0.06102631443356));
#50261=CARTESIAN_POINT('Ctrl Pts',(2.422826062441,-2.991711305314,0.0001240945758373));
#50262=CARTESIAN_POINT('Ctrl Pts',(0.6532239084002,-3.79387138814,-0.06077812528188));
#50263=CARTESIAN_POINT('Ctrl Pts',(-1.282760876264,-3.629705696773,-0.1216803451396));
#50264=CARTESIAN_POINT('Ctrl Pts',(-2.892003426424,-2.540971797446,-0.1825825649973));
#50265=CARTESIAN_POINT('Ctrl Pts',(-3.764596666965,-0.8050068460156,-0.243484784855));
#50266=CARTESIAN_POINT('Ctrl Pts',(-3.678274874416,1.136009715224,-0.3043870047128));
#50267=CARTESIAN_POINT('Ctrl Pts',(-2.655025721206,2.787662522746,-0.3652892245705));
#50268=CARTESIAN_POINT('Ctrl Pts',(-0.9554904793529,3.729244153642,-0.4261914444282));
#50269=CARTESIAN_POINT('Ctrl Pts',(0.9874265601991,3.720915582642,-0.4870936642859));
#50270=CARTESIAN_POINT('Ctrl Pts',(2.678827069895,2.764798278589,-0.5479958841436));
#50271=CARTESIAN_POINT('Ctrl Pts',(3.687878821624,1.104433695434,-0.6088981040013));
#50272=CARTESIAN_POINT('Ctrl Pts',(3.757556933874,-0.8372513835842,-0.6698003238591));
#50273=CARTESIAN_POINT('Ctrl Pts',(2.870113051872,-2.565672438204,-0.7307025437168));
#50274=CARTESIAN_POINT('Ctrl Pts',(1.251596194444,-3.640567394886,-0.7916047635745));
#50275=CARTESIAN_POINT('Ctrl Pts',(-0.6857262770364,-3.788139842145,-0.8525069834322));
#50276=CARTESIAN_POINT('Ctrl Pts',(-2.448381081905,-2.97080024041,-0.9134092032899));
#50277=CARTESIAN_POINT('Ctrl Pts',(-3.58738615237,-1.396740700514,-0.9743114231477));
#50278=CARTESIAN_POINT('Ctrl Pts',(-3.81261499833,0.5330955497161,-1.035213643005));
#50279=CARTESIAN_POINT('Ctrl Pts',(-3.066697502499,2.327142114001,-1.096115862863));
#50280=CARTESIAN_POINT('Ctrl Pts',(-1.539633191959,3.52842084025,-1.157018082721));
#50281=CARTESIAN_POINT('Ctrl Pts',(0.3796052931495,3.830942939583,-1.217920302579));
#50282=CARTESIAN_POINT('Ctrl Pts',(2.202151013929,3.157650222153,-1.278822522436));
#50283=CARTESIAN_POINT('Ctrl Pts',(3.463766524566,1.680043268575,-1.339724742294));
#50284=CARTESIAN_POINT('Ctrl Pts',(3.843094136847,-0.2255029493641,-1.400626962152));
#50285=CARTESIAN_POINT('Ctrl Pts',(3.243511671973,-2.073609442694,-1.461529182009));
#50286=CARTESIAN_POINT('Ctrl Pts',(1.817744844909,-3.393526951812,-1.522431401867));
#50287=CARTESIAN_POINT('Ctrl Pts',(-0.07103811267848,-3.849050856693,-1.583333621725));
#50288=CARTESIAN_POINT('Ctrl Pts',(-1.941720436514,-3.324136478948,-1.644235841583));
#50289=CARTESIAN_POINT('Ctrl Pts',(-3.317831105739,-1.952541783671,-1.70513806144));
#50290=CARTESIAN_POINT('Ctrl Pts',(-3.848744774803,-0.08344356796759,-1.766040281298));
#50291=CARTESIAN_POINT('Ctrl Pts',(-3.549324121726,1.176409563546,-1.806641761203));
#50292=CARTESIAN_POINT('Ctrl Pts',(-3.255099806209,1.730007907414,-1.826942501156));
#50293=CARTESIAN_POINT('Ctrl Pts',(3.488964223634,0.4573807194704,0.02524790076017));
#50294=CARTESIAN_POINT('Ctrl Pts',(3.566751457173,-0.1359911987526,0.004947160807598));
#50295=CARTESIAN_POINT('Ctrl Pts',(3.412852153803,-1.362493148022,-0.03565431909755));
#50296=CARTESIAN_POINT('Ctrl Pts',(2.312764680731,-2.855807252999,-0.09655653895527));
#50297=CARTESIAN_POINT('Ctrl Pts',(0.6235499969961,-3.621527721592,-0.157458758813));
#50298=CARTESIAN_POINT('Ctrl Pts',(-1.224489076801,-3.464819562196,-0.2183609786707));
#50299=CARTESIAN_POINT('Ctrl Pts',(-2.760628790021,-2.425543425906,-0.2792631985284));
#50300=CARTESIAN_POINT('Ctrl Pts',(-3.593582859094,-0.7684379122684,-0.3401654183861));
#50301=CARTESIAN_POINT('Ctrl Pts',(-3.511182394579,1.084404360291,-0.4010676382439));
#50302=CARTESIAN_POINT('Ctrl Pts',(-2.534416237974,2.661027766025,-0.4619698581016));
#50303=CARTESIAN_POINT('Ctrl Pts',(-0.9120855465769,3.559836299465,-0.5228720779593));
#50304=CARTESIAN_POINT('Ctrl Pts',(0.9425708715315,3.551886069298,-0.583774297817));
#50305=CARTESIAN_POINT('Ctrl Pts',(2.557136366115,2.639202172699,-0.6446765176747));
#50306=CARTESIAN_POINT('Ctrl Pts',(3.520350064616,1.054262739949,-0.7055787375324));
#50307=CARTESIAN_POINT('Ctrl Pts',(3.586862918977,-0.799217681725,-0.7664809573902));
#50308=CARTESIAN_POINT('Ctrl Pts',(2.739732826461,-2.4491219941,-0.8273831772479));
#50309=CARTESIAN_POINT('Ctrl Pts',(1.194740108636,-3.475187847464,-0.8882853971056));
#50310=CARTESIAN_POINT('Ctrl Pts',(-0.6545758850643,-3.616056541738,-0.9491876169633));
#50311=CARTESIAN_POINT('Ctrl Pts',(-2.33715881589,-2.835846112125,-1.010089836821));
#50312=CARTESIAN_POINT('Ctrl Pts',(-3.424422461836,-1.333291155467,-1.070992056679));
#50313=CARTESIAN_POINT('Ctrl Pts',(-3.639419868416,0.5088786925118,-1.131894276536));
#50314=CARTESIAN_POINT('Ctrl Pts',(-2.92738706266,2.221427353675,-1.192796496394));
#50315=CARTESIAN_POINT('Ctrl Pts',(-1.469692489628,3.368135758728,-1.253698716252));
#50316=CARTESIAN_POINT('Ctrl Pts',(0.3623610164282,3.656915228838,-1.31460093611));
#50317=CARTESIAN_POINT('Ctrl Pts',(2.102114206878,3.0142080858,-1.375503155967));
#50318=CARTESIAN_POINT('Ctrl Pts',(3.306418485628,1.603724177272,-1.436405375825));
#50319=CARTESIAN_POINT('Ctrl Pts',(3.668514435358,-0.2152590583265,-1.497307595683));
#50320=CARTESIAN_POINT('Ctrl Pts',(3.096169119512,-1.979411875677,-1.558209815541));
#50321=CARTESIAN_POINT('Ctrl Pts',(1.735170403298,-3.239369676151,-1.619112035398));
#50322=CARTESIAN_POINT('Ctrl Pts',(-0.06781107423909,-3.674200560121,-1.680014255256));
#50323=CARTESIAN_POINT('Ctrl Pts',(-1.85351417299,-3.173131394623,-1.740916475114));
#50324=CARTESIAN_POINT('Ctrl Pts',(-3.167112454723,-1.863843940318,-1.801818694971));
#50325=CARTESIAN_POINT('Ctrl Pts',(-3.673908382571,-0.07965298864055,-1.862720914829));
#50326=CARTESIAN_POINT('Ctrl Pts',(-3.388089469752,1.122968970337,-1.903322394734));
#50327=CARTESIAN_POINT('Ctrl Pts',(-3.10723084119,1.651419079429,-1.923623134687));
#50328=CARTESIAN_POINT('Ctrl Pts',(3.47936545704605,-0.650670105535317,
-4.76018332824096E-10));
#50329=CARTESIAN_POINT('Ctrl Pts',(3.38968160510127,-1.13436012879633,-0.0163342927899063));
#50330=CARTESIAN_POINT('Ctrl Pts',(3.21731640401101,-1.5020431215797,-0.0305998613834371));
#50331=CARTESIAN_POINT('Ctrl Pts',(2.91462511544118,-2.03331814851161,-0.051072270408391));
#50332=CARTESIAN_POINT('Ctrl Pts',(2.71437316642751,-2.29491396340406,-0.0617505493407693));
#50333=CARTESIAN_POINT('Ctrl Pts',(2.31900078354353,-2.68463010998948,-0.0804698268472847));
#50334=CARTESIAN_POINT('Ctrl Pts',(2.14143413280956,-2.82773453209897,-0.0883278725496207));
#50335=CARTESIAN_POINT('Ctrl Pts',(1.75686408167297,-3.0810374614634,-0.103984992970782));
#50336=CARTESIAN_POINT('Ctrl Pts',(1.54943099477353,-3.19014995951601,-0.111846840226663));
#50337=CARTESIAN_POINT('Ctrl Pts',(1.00210135526143,-3.41325842701738,-0.131677489920045));
#50338=CARTESIAN_POINT('Ctrl Pts',(0.544373821935983,-3.54350905670246,
-0.147084119947701));
#50339=CARTESIAN_POINT('Ctrl Pts',(-0.357377907987189,-3.53673648881336,
-0.177838185184495));
#50340=CARTESIAN_POINT('Ctrl Pts',(-0.693343665582159,-3.48661654134669,
-0.189369643270235));
#50341=CARTESIAN_POINT('Ctrl Pts',(-1.16631985005951,-3.3457926319962,-0.205793243319711));
#50342=CARTESIAN_POINT('Ctrl Pts',(-1.31431715107854,-3.29078468383094,
-0.210902681306299));
#50343=CARTESIAN_POINT('Ctrl Pts',(-1.66823366960176,-3.13072836053275,
-0.223802193319174));
#50344=CARTESIAN_POINT('Ctrl Pts',(-1.86879091517682,-3.01462962777927,
-0.231756118939603));
#50345=CARTESIAN_POINT('Ctrl Pts',(-2.27584383075194,-2.72334336428232,
-0.249039274135891));
#50346=CARTESIAN_POINT('Ctrl Pts',(-2.47767451265281,-2.54136729640291,
-0.258366099123228));
#50347=CARTESIAN_POINT('Ctrl Pts',(-2.75400641105814,-2.22855213811819,
-0.272072041886219));
#50348=CARTESIAN_POINT('Ctrl Pts',(-2.84474988098196,-2.11194504812941,
-0.276775941565928));
#50349=CARTESIAN_POINT('Ctrl Pts',(-3.09280421483781,-1.74728848189743,
-0.291270929049092));
#50350=CARTESIAN_POINT('Ctrl Pts',(-3.22624023808558,-1.48418850547433,
-0.301617466166435));
#50351=CARTESIAN_POINT('Ctrl Pts',(-3.38896817920167,-1.03573903467768,
-0.318200875307344));
#50352=CARTESIAN_POINT('Ctrl Pts',(-3.43862282422981,-0.85697874637879,
-0.324545149882344));
#50353=CARTESIAN_POINT('Ctrl Pts',(-3.49480773816316,-0.570080244508614,
-0.334116350045796));
#50354=CARTESIAN_POINT('Ctrl Pts',(-3.510692569015,-0.463741682587342,-0.337557184422652));
#50355=CARTESIAN_POINT('Ctrl Pts',(-3.5322046936541,-0.254588229225586,
-0.344328485772883));
#50356=CARTESIAN_POINT('Ctrl Pts',(-3.53823753943844,-0.151825593456445,
-0.347657538444068));
#50357=CARTESIAN_POINT('Ctrl Pts',(-3.54240969027316,0.149585157253516,
-0.357706645183831));
#50358=CARTESIAN_POINT('Ctrl Pts',(-3.52796952112444,0.348330577797038,
-0.364700189646956));
#50359=CARTESIAN_POINT('Ctrl Pts',(-3.47646306433639,0.676052215094485,
-0.376361244191089));
#50360=CARTESIAN_POINT('Ctrl Pts',(-3.44841356490036,0.806462723056864,
-0.381034515032509));
#50361=CARTESIAN_POINT('Ctrl Pts',(-3.35560332748102,1.14522778786507,-0.393019456018703));
#50362=CARTESIAN_POINT('Ctrl Pts',(-3.27882099545358,1.35034350117479,-0.399978094827215));
#50363=CARTESIAN_POINT('Ctrl Pts',(-3.13698038924816,1.64350653400522,-0.410474690998547));
#50364=CARTESIAN_POINT('Ctrl Pts',(-3.0856854410113,1.73822072635831,-0.413968256504382));
#50365=CARTESIAN_POINT('Ctrl Pts',(-2.94369496598558,1.97346169218265,-0.42315571452732));
#50366=CARTESIAN_POINT('Ctrl Pts',(-2.84709866167595,2.10988559529324,-0.429024287845091));
#50367=CARTESIAN_POINT('Ctrl Pts',(-2.66185301320036,2.3360052457361,-0.439341131585642));
#50368=CARTESIAN_POINT('Ctrl Pts',(-2.57692823718464,2.4290949577846,-0.443787944738417));
#50369=CARTESIAN_POINT('Ctrl Pts',(-2.34801037244829,2.65495355641731,-0.454840078048012));
#50370=CARTESIAN_POINT('Ctrl Pts',(-2.19737874054907,2.78106379178483,-0.461198734534271));
#50371=CARTESIAN_POINT('Ctrl Pts',(-1.92036964617305,2.97668163812499,-0.472153358889957));
#50372=CARTESIAN_POINT('Ctrl Pts',(-1.79827836464648,3.05231368516772,-0.476773484087216));
#50373=CARTESIAN_POINT('Ctrl Pts',(-1.52170858337329,3.20088944047865,-0.487197281551584));
#50374=CARTESIAN_POINT('Ctrl Pts',(-1.36651704388717,3.26994890434684,-0.493106941951451));
#50375=CARTESIAN_POINT('Ctrl Pts',(-1.0882764766723,3.37037022818363,-0.503540441191488));
#50376=CARTESIAN_POINT('Ctrl Pts',(-0.967441676780562,3.4067930852543,-0.507995906633045));
#50377=CARTESIAN_POINT('Ctrl Pts',(-0.626060958562132,3.49033262751781,
-0.520035397606642));
#50378=CARTESIAN_POINT('Ctrl Pts',(-0.401955790064716,3.52324750995501,
-0.527362777079245));
#50379=CARTESIAN_POINT('Ctrl Pts',(0.046994536685491,3.54632696983221,-0.542004409069419));
#50380=CARTESIAN_POINT('Ctrl Pts',(0.272343911910052,3.53676804640221,-0.549351444815277));
#50381=CARTESIAN_POINT('Ctrl Pts',(0.714543154902712,3.47409220313038,-0.564808276006456));
#50382=CARTESIAN_POINT('Ctrl Pts',(0.93070998540505,3.42197040915761,-0.57268477880501));
#50383=CARTESIAN_POINT('Ctrl Pts',(1.35551282987101,3.27687017235962,-0.587857205620805));
#50384=CARTESIAN_POINT('Ctrl Pts',(1.56384301143286,3.18279217961999,-0.595311859425859));
#50385=CARTESIAN_POINT('Ctrl Pts',(1.92537900638715,2.9760312934102,-0.609037087892114));
#50386=CARTESIAN_POINT('Ctrl Pts',(2.08198624499094,2.86916473810887,-0.61529942392855));
#50387=CARTESIAN_POINT('Ctrl Pts',(2.36807079450993,2.63748467631263,-0.627871892321534));
#50388=CARTESIAN_POINT('Ctrl Pts',(2.4980622899226,2.51418367684318,-0.634131858635528));
#50389=CARTESIAN_POINT('Ctrl Pts',(2.91486188186395,2.05465451194467,-0.655285397185308));
#50390=CARTESIAN_POINT('Ctrl Pts',(3.15095910649664,1.67145041150498,-0.669813419630624));
#50391=CARTESIAN_POINT('Ctrl Pts',(3.52463613391811,0.692569723114426,-0.705052234401755));
#50392=CARTESIAN_POINT('Ctrl Pts',(3.54621633695908,0.200862879463424,-0.721539718522704));
#50393=CARTESIAN_POINT('Ctrl Pts',(3.52666383983987,-0.481879494777179,
-0.744564135163527));
#50394=CARTESIAN_POINT('Ctrl Pts',(3.45811077461403,-0.842176755564941,
-0.756420392180674));
#50395=CARTESIAN_POINT('Ctrl Pts',(3.25736628656111,-1.40358634041913,-0.776631454521696));
#50396=CARTESIAN_POINT('Ctrl Pts',(3.15865650858907,-1.61251781614335,-0.784565833919242));
#50397=CARTESIAN_POINT('Ctrl Pts',(2.92821055064976,-1.99952438504932,-0.79997664532621));
#50398=CARTESIAN_POINT('Ctrl Pts',(2.79793621469974,-2.17863074591583,-0.807458959872579));
#50399=CARTESIAN_POINT('Ctrl Pts',(2.51630386371993,-2.49830868772162,-0.821470377673543));
#50400=CARTESIAN_POINT('Ctrl Pts',(2.36755151546159,-2.64000413604234,-0.828064602662562));
#50401=CARTESIAN_POINT('Ctrl Pts',(1.99312519657172,-2.93755773356542,-0.844298502278355));
#50402=CARTESIAN_POINT('Ctrl Pts',(1.76063245456122,-3.08186847586508,-0.853877731932693));
#50403=CARTESIAN_POINT('Ctrl Pts',(1.33245049192624,-3.28478053849265,-0.87012937293106));
#50404=CARTESIAN_POINT('Ctrl Pts',(1.14252574734553,-3.35592075561169,-0.876844985832534));
#50405=CARTESIAN_POINT('Ctrl Pts',(0.835389687708069,-3.44181393966169,
-0.887141175089021));
#50406=CARTESIAN_POINT('Ctrl Pts',(0.721288461272165,-3.46769286696527,
-0.890894806446406));
#50407=CARTESIAN_POINT('Ctrl Pts',(0.387338261788605,-3.52577373228229,
-0.902111489145458));
#50408=CARTESIAN_POINT('Ctrl Pts',(0.165112110420184,-3.54257922935625,
-0.909895716810536));
#50409=CARTESIAN_POINT('Ctrl Pts',(-0.248910843267179,-3.53542029728434,
-0.924394096550147));
#50410=CARTESIAN_POINT('Ctrl Pts',(-0.441035985293887,-3.51655394379901,
-0.931113473593433));
#50411=CARTESIAN_POINT('Ctrl Pts',(-0.740628871199496,-3.46259388153705,
-0.941231187915767));
#50412=CARTESIAN_POINT('Ctrl Pts',(-0.849962403987996,-3.43756499369767,
-0.944845633418973));
#50413=CARTESIAN_POINT('Ctrl Pts',(-1.13273893727573,-3.35856256977466,
-0.954286472322189));
#50414=CARTESIAN_POINT('Ctrl Pts',(-1.30409982554882,-3.29619680482933,
-0.960120117434646));
#50415=CARTESIAN_POINT('Ctrl Pts',(-1.5789481415045,-3.17049461743956,-0.970410037395858));
#50416=CARTESIAN_POINT('Ctrl Pts',(-1.68508967793161,-3.11514817467682,
-0.974596467727152));
#50417=CARTESIAN_POINT('Ctrl Pts',(-1.97738922218214,-2.94340431585692,
-0.986528963749778));
#50418=CARTESIAN_POINT('Ctrl Pts',(-2.1563216082851,-2.81462295238,-0.994303317449499));
#50419=CARTESIAN_POINT('Ctrl Pts',(-2.41987175853691,-2.58567334603244,
-1.00589439518714));
#50420=CARTESIAN_POINT('Ctrl Pts',(-2.51312436759297,-2.49536781564739,
-1.01007085526243));
#50421=CARTESIAN_POINT('Ctrl Pts',(-2.72305745168003,-2.26857122414977,
-1.02002226516135));
#50422=CARTESIAN_POINT('Ctrl Pts',(-2.83508808087039,-2.12753626309955,
-1.02580379523761));
#50423=CARTESIAN_POINT('Ctrl Pts',(-2.99361470261002,-1.89222941309494,
-1.03545767531674));
#50424=CARTESIAN_POINT('Ctrl Pts',(-3.04776462376792,-1.80344547790966,
-1.03909359957781));
#50425=CARTESIAN_POINT('Ctrl Pts',(-3.20701043613858,-1.51431408086861,
-1.05072470901445));
#50426=CARTESIAN_POINT('Ctrl Pts',(-3.29705654279892,-1.30565120601265,
-1.05872996995417));
#50427=CARTESIAN_POINT('Ctrl Pts',(-3.41754289628483,-0.933658716688529,
-1.071713389086));
#50428=CARTESIAN_POINT('Ctrl Pts',(-3.45754212510686,-0.773364951218968,
-1.07702302189057));
#50429=CARTESIAN_POINT('Ctrl Pts',(-3.51751725536643,-0.43432930684903,
-1.08819414784575));
#50430=CARTESIAN_POINT('Ctrl Pts',(-3.5354268517809,-0.2549872896286,-1.094074769187));
#50431=CARTESIAN_POINT('Ctrl Pts',(-3.54172630457513,0.0453303041890943,
-1.10440520742965));
#50432=CARTESIAN_POINT('Ctrl Pts',(-3.53795037963495,0.165791783736955,
-1.10866306074787));
#50433=CARTESIAN_POINT('Ctrl Pts',(-3.5121208012954,0.478496558675268,-1.1197015257511));
#50434=CARTESIAN_POINT('Ctrl Pts',(-3.48036769515908,0.669956557885907,
-1.12632685190405));
#50435=CARTESIAN_POINT('Ctrl Pts',(-3.34339654372091,1.21795369627118,-1.14506294601682));
#50436=CARTESIAN_POINT('Ctrl Pts',(-3.19710898742592,1.56562609795509,-1.15692104335934));
#50437=CARTESIAN_POINT('Ctrl Pts',(-2.9010238832775,2.03669728081193,-1.17620511785791));
#50438=CARTESIAN_POINT('Ctrl Pts',(-2.79175489844723,2.1834392507992,-1.18262151021084));
#50439=CARTESIAN_POINT('Ctrl Pts',(-2.50349542827591,2.51435572427153,-1.19752854069075));
#50440=CARTESIAN_POINT('Ctrl Pts',(-2.31414992392246,2.68963315454088,-1.20598303789464));
#50441=CARTESIAN_POINT('Ctrl Pts',(-1.73142820159205,3.12306231020025,-1.23003668946368));
#50442=CARTESIAN_POINT('Ctrl Pts',(-1.30716002119752,3.32240006877921,-1.24597736898554));
#50443=CARTESIAN_POINT('Ctrl Pts',(-0.47635298230646,3.52788828947166,-1.27486413134219));
#50444=CARTESIAN_POINT('Ctrl Pts',(-0.00281208568693243,3.5803728560144,
-1.2903145799909));
#50445=CARTESIAN_POINT('Ctrl Pts',(0.962642950390408,3.43479177006313,-1.32329300622975));
#50446=CARTESIAN_POINT('Ctrl Pts',(1.38814831774985,3.28503819142457,-1.33859634255934));
#50447=CARTESIAN_POINT('Ctrl Pts',(1.95170676635034,2.96024721458227,-1.36037600144928));
#50448=CARTESIAN_POINT('Ctrl Pts',(2.12275248225467,2.84072814757798,-1.36712528274452));
#50449=CARTESIAN_POINT('Ctrl Pts',(2.43738460292837,2.57508324792456,-1.3808780636241));
#50450=CARTESIAN_POINT('Ctrl Pts',(2.58098915698118,2.43045029872562,-1.38786008447071));
#50451=CARTESIAN_POINT('Ctrl Pts',(2.8586394859375,2.09869429439186,-1.40277376981807));
#50452=CARTESIAN_POINT('Ctrl Pts',(2.98906315475086,1.90841226348734,-1.41070910726487));
#50453=CARTESIAN_POINT('Ctrl Pts',(3.19815239678626,1.5299820023293,-1.42517700597003));
#50454=CARTESIAN_POINT('Ctrl Pts',(3.28109724395731,1.34413783022801,-1.43163438273803));
#50455=CARTESIAN_POINT('Ctrl Pts',(3.39634803821763,1.00968483965148,-1.44327843029447));
#50456=CARTESIAN_POINT('Ctrl Pts',(3.43602173216469,0.864015457437118,-1.44841754354509));
#50457=CARTESIAN_POINT('Ctrl Pts',(3.53497204662554,0.381480622891467,-1.46545574416584));
#50458=CARTESIAN_POINT('Ctrl Pts',(3.55511946807515,0.0361968277201632,
-1.47760960084256));
#50459=CARTESIAN_POINT('Ctrl Pts',(3.51083616031935,-0.485201730785517,
-1.49465759219851));
#50460=CARTESIAN_POINT('Ctrl Pts',(3.48174213458368,-0.664501243521017,
-1.50037677058524));
#50461=CARTESIAN_POINT('Ctrl Pts',(3.41106750725955,-0.953956521790304,
-1.51024647323768));
#50462=CARTESIAN_POINT('Ctrl Pts',(3.37761677741219,-1.065844345292,-1.5142397706781));
#50463=CARTESIAN_POINT('Ctrl Pts',(3.28884372645565,-1.31672952124942,-1.52348839041811));
#50464=CARTESIAN_POINT('Ctrl Pts',(3.2299412503904,-1.45458962814811,-1.52878457157517));
#50465=CARTESIAN_POINT('Ctrl Pts',(3.09404276007104,-1.7245727475059,-1.53934251535052));
#50466=CARTESIAN_POINT('Ctrl Pts',(3.01668666086911,-1.85655784238407,-1.54458881634802));
#50467=CARTESIAN_POINT('Ctrl Pts',(2.85401911859892,-2.09745480011405,-1.55416499746065));
#50468=CARTESIAN_POINT('Ctrl Pts',(2.77017406232646,-2.20737978061453,-1.55857514890632));
#50469=CARTESIAN_POINT('Ctrl Pts',(2.57968153257193,-2.42891544274371,-1.56798252196686));
#50470=CARTESIAN_POINT('Ctrl Pts',(2.47142032382288,-2.53932660034174,-1.57300681173571));
#50471=CARTESIAN_POINT('Ctrl Pts',(2.26674889871784,-2.72156142954571,-1.58237779740596));
#50472=CARTESIAN_POINT('Ctrl Pts',(2.17374705006462,-2.79614947193613,-1.58656527915603));
#50473=CARTESIAN_POINT('Ctrl Pts',(1.91703885326229,-2.981587522261,-1.59773611982311));
#50474=CARTESIAN_POINT('Ctrl Pts',(1.74714305212033,-3.08391680910354,-1.60471445294895));
#50475=CARTESIAN_POINT('Ctrl Pts',(1.45057804879874,-3.23076970868732,-1.61574175119124));
#50476=CARTESIAN_POINT('Ctrl Pts',(1.32782272610411,-3.28327703514645,-1.62005309437341));
#50477=CARTESIAN_POINT('Ctrl Pts',(1.01941548265538,-3.39520141140918,-1.6306426349041));
#50478=CARTESIAN_POINT('Ctrl Pts',(0.830807073977391,-3.44665349448751,
-1.63691624518133));
#50479=CARTESIAN_POINT('Ctrl Pts',(0.537265653796465,-3.50051786116815,
-1.64709107891152));
#50480=CARTESIAN_POINT('Ctrl Pts',(0.434611008595293,-3.51460779609371,
-1.65072101263908));
#50481=CARTESIAN_POINT('Ctrl Pts',(0.225619775887951,-3.5339495654796,-1.65811986209128));
#50482=CARTESIAN_POINT('Ctrl Pts',(0.119263996534475,-3.53894775575562,
-1.66188927246119));
#50483=CARTESIAN_POINT('Ctrl Pts',(-0.162387922266383,-3.53959510891038,
-1.67168223495486));
#50484=CARTESIAN_POINT('Ctrl Pts',(-0.337739076371664,-3.52708781787918,
-1.67751988457496));
#50485=CARTESIAN_POINT('Ctrl Pts',(-0.823259525169688,-3.45652111654826,
-1.69357469929039));
#50486=CARTESIAN_POINT('Ctrl Pts',(-1.13038309976021,-3.36988303997754,
-1.70368211808393));
#50487=CARTESIAN_POINT('Ctrl Pts',(-1.57217878647256,-3.17584433311836,
-1.72045025447723));
#50488=CARTESIAN_POINT('Ctrl Pts',(-1.71819803180833,-3.09889906111367,
-1.72631027718014));
#50489=CARTESIAN_POINT('Ctrl Pts',(-2.00528096082112,-2.92123243107852,
-1.73788904679044));
#50490=CARTESIAN_POINT('Ctrl Pts',(-2.1457412982902,-2.81950204643683,-1.74364609212141));
#50491=CARTESIAN_POINT('Ctrl Pts',(-2.45175935497528,-2.56229840409746,
-1.75683120431308));
#50492=CARTESIAN_POINT('Ctrl Pts',(-2.61159360171125,-2.39988572783075,
-1.76422818059013));
#50493=CARTESIAN_POINT('Ctrl Pts',(-2.90047120263545,-2.04298664406632,
-1.77964685741253));
#50494=CARTESIAN_POINT('Ctrl Pts',(-3.02708811987471,-1.8494542979142,-1.78776396049441));
#50495=CARTESIAN_POINT('Ctrl Pts',(-3.2785531111803,-1.36838472126582,-1.80632724926333));
#50496=CARTESIAN_POINT('Ctrl Pts',(-3.38664983884328,-1.07273690227071,
-1.81667718039125));
#50497=CARTESIAN_POINT('Ctrl Pts',(-3.55709012362553,-0.311449824495371,
-1.84263604131696));
#50498=CARTESIAN_POINT('Ctrl Pts',(-3.56668710098688,0.155659841452416,
-1.85831670276059));
#50499=CARTESIAN_POINT('Ctrl Pts',(-3.48534662539474,0.614552563975331,
-1.87410368362543));
#50500=CARTESIAN_POINT('Ctrl Pts',(-1.474278984797,3.218400452862,0.2851535733017));
#50501=CARTESIAN_POINT('Ctrl Pts',(-0.8630012166369,3.498413453318,0.2624820910321));
#50502=CARTESIAN_POINT('Ctrl Pts',(0.5221776990155,3.700023104325,0.2171391264928));
#50503=CARTESIAN_POINT('Ctrl Pts',(2.435930668196,2.833759612852,0.1491246796839));
#50504=CARTESIAN_POINT('Ctrl Pts',(3.579719046399,1.071968677256,0.0811102328749));
#50505=CARTESIAN_POINT('Ctrl Pts',(3.592463812753,-1.028508980771,0.01309578606595));
#50506=CARTESIAN_POINT('Ctrl Pts',(2.470048545545,-2.804008613372,-0.05491866074299));
#50507=CARTESIAN_POINT('Ctrl Pts',(0.5671562238518,-3.693499629492,-0.1229331075519));
#50508=CARTESIAN_POINT('Ctrl Pts',(-1.514946598719,-3.415924974072,-0.1909475543609));
#50509=CARTESIAN_POINT('Ctrl Pts',(-3.118358578085,-2.058991469437,-0.2589620011698));
#50510=CARTESIAN_POINT('Ctrl Pts',(-3.736436540906,-0.05146107378251,-0.3269764479788));
#50511=CARTESIAN_POINT('Ctrl Pts',(-3.173881046339,1.972329924211,-0.3949908947877));
#50512=CARTESIAN_POINT('Ctrl Pts',(-1.608447541355,3.37290716424,-0.4630053415967));
#50513=CARTESIAN_POINT('Ctrl Pts',(0.4652207285,3.707718423233,-0.5310197884056));
#50514=CARTESIAN_POINT('Ctrl Pts',(2.391889272583,2.870970557034,-0.5990342352146));
#50515=CARTESIAN_POINT('Ctrl Pts',(3.56277234894,1.127057860763,-0.6670486820235));
#50516=CARTESIAN_POINT('Ctrl Pts',(3.607896136365,-0.972980832813,-0.7350631288325));
#50517=CARTESIAN_POINT('Ctrl Pts',(2.513002490438,-2.765578549758,-0.8030775756414));
#50518=CARTESIAN_POINT('Ctrl Pts',(0.6240542096492,-3.6843130398,-0.8710920224504));
#50519=CARTESIAN_POINT('Ctrl Pts',(-1.462081753792,-3.438884001694,-0.9391064692593));
#50520=CARTESIAN_POINT('Ctrl Pts',(-3.086231389081,-2.106841722746,-1.007120916068));
#50521=CARTESIAN_POINT('Ctrl Pts',(-3.735198409991,-0.1090828593897,-1.075135362877));
#50522=CARTESIAN_POINT('Ctrl Pts',(-3.203923222005,1.92314383741,-1.143149809686));
#50523=CARTESIAN_POINT('Ctrl Pts',(-1.660277337509,3.347698521193,-1.211164256495));
#50524=CARTESIAN_POINT('Ctrl Pts',(0.4079804125565,3.714452617722,-1.279178703304));
#50525=CARTESIAN_POINT('Ctrl Pts',(2.347325129349,2.907519704122,-1.347193150113));
#50526=CARTESIAN_POINT('Ctrl Pts',(3.544965740915,1.181873310129,-1.415207596922));
#50527=CARTESIAN_POINT('Ctrl Pts',(3.622473367692,-0.917219927648,-1.483222043731));
#50528=CARTESIAN_POINT('Ctrl Pts',(2.55535821773,-2.726490143077,-1.55123649054));
#50529=CARTESIAN_POINT('Ctrl Pts',(0.6808021457163,-3.674253040803,-1.619250937349));
#50530=CARTESIAN_POINT('Ctrl Pts',(-1.408862321174,-3.461013183469,-1.687265384158));
#50531=CARTESIAN_POINT('Ctrl Pts',(-3.053395514624,-2.154234804974,-1.755279830967));
#50532=CARTESIAN_POINT('Ctrl Pts',(-3.732976491904,-0.1665143620988,-1.823294277776));
#50533=CARTESIAN_POINT('Ctrl Pts',(-3.400031230562,1.193086510473,-1.868637242315));
#50534=CARTESIAN_POINT('Ctrl Pts',(-3.062932791185,1.774835968952,-1.891308724585));
#50535=CARTESIAN_POINT('Ctrl Pts',(-1.474278984797,3.218400452862,0.1959004713425));
#50536=CARTESIAN_POINT('Ctrl Pts',(-0.8630012166369,3.498413453318,0.1732289890729));
#50537=CARTESIAN_POINT('Ctrl Pts',(0.5221776990155,3.700023104325,0.1278860245336));
#50538=CARTESIAN_POINT('Ctrl Pts',(2.435930668196,2.833759612852,0.05987157772462));
#50539=CARTESIAN_POINT('Ctrl Pts',(3.579719046399,1.071968677256,-0.008142869084334));
#50540=CARTESIAN_POINT('Ctrl Pts',(3.592463812753,-1.028508980771,-0.07615731589328));
#50541=CARTESIAN_POINT('Ctrl Pts',(2.470048545545,-2.804008613372,-0.1441717627022));
#50542=CARTESIAN_POINT('Ctrl Pts',(0.5671562238518,-3.693499629492,-0.2121862095112));
#50543=CARTESIAN_POINT('Ctrl Pts',(-1.514946598719,-3.415924974072,-0.2802006563201));
#50544=CARTESIAN_POINT('Ctrl Pts',(-3.118358578085,-2.058991469437,-0.3482151031291));
#50545=CARTESIAN_POINT('Ctrl Pts',(-3.736436540906,-0.05146107378251,-0.416229549938));
#50546=CARTESIAN_POINT('Ctrl Pts',(-3.173881046339,1.972329924211,-0.484243996747));
#50547=CARTESIAN_POINT('Ctrl Pts',(-1.608447541355,3.37290716424,-0.5522584435559));
#50548=CARTESIAN_POINT('Ctrl Pts',(0.4652207285,3.707718423233,-0.6202728903649));
#50549=CARTESIAN_POINT('Ctrl Pts',(2.391889272583,2.870970557034,-0.6882873371738));
#50550=CARTESIAN_POINT('Ctrl Pts',(3.56277234894,1.127057860763,-0.7563017839828));
#50551=CARTESIAN_POINT('Ctrl Pts',(3.607896136365,-0.972980832813,-0.8243162307917));
#50552=CARTESIAN_POINT('Ctrl Pts',(2.513002490438,-2.765578549758,-0.8923306776007));
#50553=CARTESIAN_POINT('Ctrl Pts',(0.6240542096492,-3.6843130398,-0.9603451244096));
#50554=CARTESIAN_POINT('Ctrl Pts',(-1.462081753792,-3.438884001694,-1.028359571219));
#50555=CARTESIAN_POINT('Ctrl Pts',(-3.086231389081,-2.106841722746,-1.096374018028));
#50556=CARTESIAN_POINT('Ctrl Pts',(-3.735198409991,-0.1090828593897,-1.164388464836));
#50557=CARTESIAN_POINT('Ctrl Pts',(-3.203923222005,1.92314383741,-1.232402911645));
#50558=CARTESIAN_POINT('Ctrl Pts',(-1.660277337509,3.347698521193,-1.300417358454));
#50559=CARTESIAN_POINT('Ctrl Pts',(0.4079804125565,3.714452617722,-1.368431805263));
#50560=CARTESIAN_POINT('Ctrl Pts',(2.347325129349,2.907519704122,-1.436446252072));
#50561=CARTESIAN_POINT('Ctrl Pts',(3.544965740915,1.181873310129,-1.504460698881));
#50562=CARTESIAN_POINT('Ctrl Pts',(3.622473367692,-0.917219927648,-1.57247514569));
#50563=CARTESIAN_POINT('Ctrl Pts',(2.55535821773,-2.726490143077,-1.640489592499));
#50564=CARTESIAN_POINT('Ctrl Pts',(0.6808021457163,-3.674253040803,-1.708504039308));
#50565=CARTESIAN_POINT('Ctrl Pts',(-1.408862321174,-3.461013183469,-1.776518486117));
#50566=CARTESIAN_POINT('Ctrl Pts',(-3.053395514624,-2.154234804974,-1.844532932926));
#50567=CARTESIAN_POINT('Ctrl Pts',(-3.732976491904,-0.1665143620988,-1.912547379735));
#50568=CARTESIAN_POINT('Ctrl Pts',(-3.400031230562,1.193086510473,-1.957890344274));
#50569=CARTESIAN_POINT('Ctrl Pts',(-3.062932791185,1.774835968952,-1.980561826544));
#50570=CARTESIAN_POINT('Ctrl Pts',(-1.474278984797,3.218400452862,0.1066473693833));
#50571=CARTESIAN_POINT('Ctrl Pts',(-0.8630012166369,3.498413453318,0.08397588711363));
#50572=CARTESIAN_POINT('Ctrl Pts',(0.5221776990155,3.700023104325,0.03863292257433));
#50573=CARTESIAN_POINT('Ctrl Pts',(2.435930668196,2.833759612852,-0.02938152423462));
#50574=CARTESIAN_POINT('Ctrl Pts',(3.579719046399,1.071968677256,-0.09739597104357));
#50575=CARTESIAN_POINT('Ctrl Pts',(3.592463812753,-1.028508980771,-0.1654104178525));
#50576=CARTESIAN_POINT('Ctrl Pts',(2.470048545545,-2.804008613372,-0.2334248646615));
#50577=CARTESIAN_POINT('Ctrl Pts',(0.5671562238518,-3.693499629492,-0.3014393114704));
#50578=CARTESIAN_POINT('Ctrl Pts',(-1.514946598719,-3.415924974072,-0.3694537582794));
#50579=CARTESIAN_POINT('Ctrl Pts',(-3.118358578085,-2.058991469437,-0.4374682050883));
#50580=CARTESIAN_POINT('Ctrl Pts',(-3.736436540906,-0.05146107378252,-0.5054826518973));
#50581=CARTESIAN_POINT('Ctrl Pts',(-3.173881046339,1.972329924211,-0.5734970987062));
#50582=CARTESIAN_POINT('Ctrl Pts',(-1.608447541355,3.37290716424,-0.6415115455152));
#50583=CARTESIAN_POINT('Ctrl Pts',(0.4652207285,3.707718423233,-0.7095259923241));
#50584=CARTESIAN_POINT('Ctrl Pts',(2.391889272583,2.870970557034,-0.7775404391331));
#50585=CARTESIAN_POINT('Ctrl Pts',(3.56277234894,1.127057860763,-0.845554885942));
#50586=CARTESIAN_POINT('Ctrl Pts',(3.607896136365,-0.972980832813,-0.9135693327509));
#50587=CARTESIAN_POINT('Ctrl Pts',(2.513002490438,-2.765578549758,-0.9815837795599));
#50588=CARTESIAN_POINT('Ctrl Pts',(0.6240542096492,-3.6843130398,-1.049598226369));
#50589=CARTESIAN_POINT('Ctrl Pts',(-1.462081753792,-3.438884001694,-1.117612673178));
#50590=CARTESIAN_POINT('Ctrl Pts',(-3.086231389081,-2.106841722746,-1.185627119987));
#50591=CARTESIAN_POINT('Ctrl Pts',(-3.735198409991,-0.1090828593897,-1.253641566796));
#50592=CARTESIAN_POINT('Ctrl Pts',(-3.203923222005,1.92314383741,-1.321656013605));
#50593=CARTESIAN_POINT('Ctrl Pts',(-1.660277337509,3.347698521193,-1.389670460414));
#50594=CARTESIAN_POINT('Ctrl Pts',(0.4079804125565,3.714452617722,-1.457684907223));
#50595=CARTESIAN_POINT('Ctrl Pts',(2.347325129348,2.907519704122,-1.525699354031));
#50596=CARTESIAN_POINT('Ctrl Pts',(3.544965740915,1.181873310129,-1.59371380084));
#50597=CARTESIAN_POINT('Ctrl Pts',(3.622473367692,-0.917219927648,-1.661728247649));
#50598=CARTESIAN_POINT('Ctrl Pts',(2.55535821773,-2.726490143077,-1.729742694458));
#50599=CARTESIAN_POINT('Ctrl Pts',(0.6808021457163,-3.674253040803,-1.797757141267));
#50600=CARTESIAN_POINT('Ctrl Pts',(-1.408862321174,-3.461013183469,-1.865771588076));
#50601=CARTESIAN_POINT('Ctrl Pts',(-3.053395514624,-2.154234804974,-1.933786034885));
#50602=CARTESIAN_POINT('Ctrl Pts',(-3.732976491904,-0.1665143620988,-2.001800481694));
#50603=CARTESIAN_POINT('Ctrl Pts',(-3.400031230562,1.193086510473,-2.047143446233));
#50604=CARTESIAN_POINT('Ctrl Pts',(-3.062932791185,1.774835968952,-2.069814928503));
#50605=CARTESIAN_POINT('Ctrl Pts',(-1.474278984797,3.218400452862,0.01739426742404));
#50606=CARTESIAN_POINT('Ctrl Pts',(-0.8630012166369,3.498413453318,-0.005277214845608));
#50607=CARTESIAN_POINT('Ctrl Pts',(0.5221776990155,3.700023104325,-0.05062017938491));
#50608=CARTESIAN_POINT('Ctrl Pts',(2.435930668196,2.833759612852,-0.1186346261939));
#50609=CARTESIAN_POINT('Ctrl Pts',(3.579719046399,1.071968677256,-0.1866490730028));
#50610=CARTESIAN_POINT('Ctrl Pts',(3.592463812753,-1.028508980771,-0.2546635198118));
#50611=CARTESIAN_POINT('Ctrl Pts',(2.470048545545,-2.804008613372,-0.3226779666207));
#50612=CARTESIAN_POINT('Ctrl Pts',(0.5671562238518,-3.693499629492,-0.3906924134296));
#50613=CARTESIAN_POINT('Ctrl Pts',(-1.514946598719,-3.415924974072,-0.4587068602386));
#50614=CARTESIAN_POINT('Ctrl Pts',(-3.118358578085,-2.058991469437,-0.5267213070475));
#50615=CARTESIAN_POINT('Ctrl Pts',(-3.736436540906,-0.05146107378252,-0.5947357538565));
#50616=CARTESIAN_POINT('Ctrl Pts',(-3.173881046339,1.972329924211,-0.6627502006654));
#50617=CARTESIAN_POINT('Ctrl Pts',(-1.608447541355,3.37290716424,-0.7307646474744));
#50618=CARTESIAN_POINT('Ctrl Pts',(0.4652207285,3.707718423233,-0.7987790942833));
#50619=CARTESIAN_POINT('Ctrl Pts',(2.391889272583,2.870970557034,-0.8667935410923));
#50620=CARTESIAN_POINT('Ctrl Pts',(3.56277234894,1.127057860763,-0.9348079879012));
#50621=CARTESIAN_POINT('Ctrl Pts',(3.607896136365,-0.972980832813,-1.00282243471));
#50622=CARTESIAN_POINT('Ctrl Pts',(2.513002490438,-2.765578549758,-1.070836881519));
#50623=CARTESIAN_POINT('Ctrl Pts',(0.6240542096492,-3.6843130398,-1.138851328328));
#50624=CARTESIAN_POINT('Ctrl Pts',(-1.462081753792,-3.438884001694,-1.206865775137));
#50625=CARTESIAN_POINT('Ctrl Pts',(-3.086231389081,-2.106841722746,-1.274880221946));
#50626=CARTESIAN_POINT('Ctrl Pts',(-3.735198409991,-0.1090828593897,-1.342894668755));
#50627=CARTESIAN_POINT('Ctrl Pts',(-3.203923222005,1.92314383741,-1.410909115564));
#50628=CARTESIAN_POINT('Ctrl Pts',(-1.660277337509,3.347698521193,-1.478923562373));
#50629=CARTESIAN_POINT('Ctrl Pts',(0.4079804125565,3.714452617722,-1.546938009182));
#50630=CARTESIAN_POINT('Ctrl Pts',(2.347325129348,2.907519704122,-1.614952455991));
#50631=CARTESIAN_POINT('Ctrl Pts',(3.544965740915,1.181873310129,-1.6829669028));
#50632=CARTESIAN_POINT('Ctrl Pts',(3.622473367692,-0.917219927648,-1.750981349609));
#50633=CARTESIAN_POINT('Ctrl Pts',(2.55535821773,-2.726490143077,-1.818995796418));
#50634=CARTESIAN_POINT('Ctrl Pts',(0.6808021457163,-3.674253040803,-1.887010243227));
#50635=CARTESIAN_POINT('Ctrl Pts',(-1.408862321174,-3.461013183469,-1.955024690035));
#50636=CARTESIAN_POINT('Ctrl Pts',(-3.053395514624,-2.154234804974,-2.023039136844));
#50637=CARTESIAN_POINT('Ctrl Pts',(-3.732976491904,-0.1665143620988,-2.091053583653));
#50638=CARTESIAN_POINT('Ctrl Pts',(-3.400031230562,1.193086510473,-2.136396548193));
#50639=CARTESIAN_POINT('Ctrl Pts',(-3.062932791185,1.774835968952,-2.159068030462));
#50640=CARTESIAN_POINT('',(-3.486219445663,0.6147145489409,-1.873914457161));
#50641=CARTESIAN_POINT('Ctrl Pts',(-3.381685401913,-1.046806497156,-1.792787013728));
#50642=CARTESIAN_POINT('Ctrl Pts',(-3.516276022629,-0.6120144524515,-1.80813423595));
#50643=CARTESIAN_POINT('Ctrl Pts',(-3.615602476197,0.3099418872051,-1.838828680394));
#50644=CARTESIAN_POINT('Ctrl Pts',(-3.233351390461,1.647480520897,-1.884870347061));
#50645=CARTESIAN_POINT('Ctrl Pts',(-2.375970535719,2.742894243674,-1.930912013728));
#50646=CARTESIAN_POINT('Ctrl Pts',(-1.16946135002,3.435270189528,-1.976953680394));
#50647=CARTESIAN_POINT('Ctrl Pts',(0.2088925691034,3.622855283072,-2.022995347061));
#50648=CARTESIAN_POINT('Ctrl Pts',(1.556551006228,3.278088863066,-2.069037013728));
#50649=CARTESIAN_POINT('Ctrl Pts',(2.675485639469,2.451630885082,-2.115078680394));
#50650=CARTESIAN_POINT('Ctrl Pts',(3.401277069744,1.264923606363,-2.161120347061));
#50651=CARTESIAN_POINT('Ctrl Pts',(3.627275538361,-0.1076550254197,-2.207162013728));
#50652=CARTESIAN_POINT('Ctrl Pts',(3.320272205746,-1.464414529052,-2.253203680394));
#50653=CARTESIAN_POINT('Ctrl Pts',(2.525378983787,-2.605988952896,-2.299245347061));
#50654=CARTESIAN_POINT('Ctrl Pts',(1.359399658728,-3.364632223854,-2.345287013728));
#50655=CARTESIAN_POINT('Ctrl Pts',(-0.006333574545319,-3.628867222688,-2.391328680394));
#50656=CARTESIAN_POINT('Ctrl Pts',(-1.371136135038,-3.359866535032,-2.437370347061));
#50657=CARTESIAN_POINT('Ctrl Pts',(-2.534460197325,-2.597157858548,-2.483412013728));
#50658=CARTESIAN_POINT('Ctrl Pts',(-3.325363738216,-1.452815694643,-2.529453680394));
#50659=CARTESIAN_POINT('Ctrl Pts',(-3.627629225714,-0.09499281438667,-2.575495347061));
#50660=CARTESIAN_POINT('Ctrl Pts',(-3.396840941408,1.276788570131,-2.621537013728));
#50661=CARTESIAN_POINT('Ctrl Pts',(-2.66691154775,2.460955145979,-2.667578680394));
#50662=CARTESIAN_POINT('Ctrl Pts',(-1.545098868578,3.283502233951,-2.713620347061));
#50663=CARTESIAN_POINT('Ctrl Pts',(-0.1962451307805,3.623562512595,-2.759662013728));
#50664=CARTESIAN_POINT('Ctrl Pts',(1.181445403903,3.431166593396,-2.805703680394));
#50665=CARTESIAN_POINT('Ctrl Pts',(2.385531115837,2.73458565955,-2.851745347061));
#50666=CARTESIAN_POINT('Ctrl Pts',(3.239080353414,1.636177220892,-2.897787013728));
#50667=CARTESIAN_POINT('Ctrl Pts',(3.616670254429,0.2973444211245,-2.943828680394));
#50668=CARTESIAN_POINT('Ctrl Pts',(3.462816724887,-1.085180982088,-2.989870347061));
#50669=CARTESIAN_POINT('Ctrl Pts',(2.80012742371,-2.30824692029,-3.035912013728));
#50670=CARTESIAN_POINT('Ctrl Pts',(1.725979731427,-3.192132735452,-3.081953680394));
#50671=CARTESIAN_POINT('Ctrl Pts',(0.3982118512334,-3.606957825589,-3.127995347061));
#50672=CARTESIAN_POINT('Ctrl Pts',(-0.9880703687869,-3.491766656059,-3.174037013728));
#50673=CARTESIAN_POINT('Ctrl Pts',(-2.229162823228,-2.863485732736,-3.220078680394));
#50674=CARTESIAN_POINT('Ctrl Pts',(-3.142695988404,-1.814436374886,-3.266120347061));
#50675=CARTESIAN_POINT('Ctrl Pts',(-3.594432799537,-0.4987687677191,-3.312162013728));
#50676=CARTESIAN_POINT('Ctrl Pts',(-3.517993812628,0.8901892879335,-3.358203680394));
#50677=CARTESIAN_POINT('Ctrl Pts',(-2.924611181723,2.148340492051,-3.404245347061));
#50678=CARTESIAN_POINT('Ctrl Pts',(-1.90147817544,3.090808661559,-3.450287013728));
#50679=CARTESIAN_POINT('Ctrl Pts',(-0.598936759323,3.579104942911,-3.496328680394));
#50680=CARTESIAN_POINT('Ctrl Pts',(0.791614064251,3.541477743446,-3.542370347061));
#50681=CARTESIAN_POINT('Ctrl Pts',(2.065842949582,2.983456106884,-3.588412013728));
#50682=CARTESIAN_POINT('Ctrl Pts',(3.036511215093,1.98703726051,-3.634453680394));
#50683=CARTESIAN_POINT('Ctrl Pts',(3.560986207913,0.6986377180585,-3.680495347061));
#50684=CARTESIAN_POINT('Ctrl Pts',(3.562200136449,-0.6924215637334,-3.726537013728));
#50685=CARTESIAN_POINT('Ctrl Pts',(3.039974622718,-1.981734524923,-3.772578680394));
#50686=CARTESIAN_POINT('Ctrl Pts',(2.071046913695,-2.979845988523,-3.818620347061));
#50687=CARTESIAN_POINT('Ctrl Pts',(0.7977939001169,-3.540090722987,-3.864662013728));
#50688=CARTESIAN_POINT('Ctrl Pts',(-0.592689133709,-3.58014483294,-3.910703680394));
#50689=CARTESIAN_POINT('Ctrl Pts',(-1.896080803293,-3.094122657786,-3.956745347061));
#50690=CARTESIAN_POINT('Ctrl Pts',(-2.920857167686,-2.153441626797,-4.002787013728));
#50691=CARTESIAN_POINT('Ctrl Pts',(-3.516434781803,-0.8963279864901,-4.048828680394));
#50692=CARTESIAN_POINT('Ctrl Pts',(-3.595297840182,0.4924945425259,-4.094870347061));
#50693=CARTESIAN_POINT('Ctrl Pts',(-3.145857989081,1.808948574891,-4.140912013728));
#50694=CARTESIAN_POINT('Ctrl Pts',(-2.234157150885,2.859590750281,-4.186953680394));
#50695=CARTESIAN_POINT('Ctrl Pts',(-0.9941631432962,3.490036830591,-4.232995347061));
#50696=CARTESIAN_POINT('Ctrl Pts',(0.3919159190425,3.607647342181,-4.279037013728));
#50697=CARTESIAN_POINT('Ctrl Pts',(1.720405782322,3.195140275457,-4.325078680394));
#50698=CARTESIAN_POINT('Ctrl Pts',(2.796094511829,2.313130544526,-4.371120347061));
#50699=CARTESIAN_POINT('Ctrl Pts',(3.460917446918,1.091223088699,-4.417162013728));
#50700=CARTESIAN_POINT('Ctrl Pts',(3.617183734391,-0.2910317178534,-4.463203680394));
#50701=CARTESIAN_POINT('Ctrl Pts',(3.241930993927,-1.630521370031,-4.509245347061));
#50702=CARTESIAN_POINT('Ctrl Pts',(2.390300577984,-2.730418332625,-4.555287013728));
#50703=CARTESIAN_POINT('Ctrl Pts',(1.187430827056,-3.429097964413,-4.601328680394));
#50704=CARTESIAN_POINT('Ctrl Pts',(-0.1899157118936,-3.62390470395,-4.647370347061));
#50705=CARTESIAN_POINT('Ctrl Pts',(-1.539383690082,-3.286174537975,-4.693412013728));
#50706=CARTESIAN_POINT('Ctrl Pts',(-2.288158074621,-2.739177136089,-4.724106458172));
#50707=CARTESIAN_POINT('Ctrl Pts',(-2.59740372034,-2.405222217086,-4.739453680394));
#50708=CARTESIAN_POINT('Ctrl Pts',(-3.381685401913,-1.046806497156,-1.882040115687));
#50709=CARTESIAN_POINT('Ctrl Pts',(-3.516276022629,-0.6120144524515,-1.897387337909));
#50710=CARTESIAN_POINT('Ctrl Pts',(-3.615602476197,0.3099418872051,-1.928081782354));
#50711=CARTESIAN_POINT('Ctrl Pts',(-3.233351390461,1.647480520897,-1.97412344902));
#50712=CARTESIAN_POINT('Ctrl Pts',(-2.375970535719,2.742894243674,-2.020165115687));
#50713=CARTESIAN_POINT('Ctrl Pts',(-1.16946135002,3.435270189528,-2.066206782354));
#50714=CARTESIAN_POINT('Ctrl Pts',(0.2088925691034,3.622855283072,-2.11224844902));
#50715=CARTESIAN_POINT('Ctrl Pts',(1.556551006228,3.278088863066,-2.158290115687));
#50716=CARTESIAN_POINT('Ctrl Pts',(2.675485639469,2.451630885082,-2.204331782354));
#50717=CARTESIAN_POINT('Ctrl Pts',(3.401277069744,1.264923606363,-2.25037344902));
#50718=CARTESIAN_POINT('Ctrl Pts',(3.627275538361,-0.1076550254197,-2.296415115687));
#50719=CARTESIAN_POINT('Ctrl Pts',(3.320272205746,-1.464414529052,-2.342456782354));
#50720=CARTESIAN_POINT('Ctrl Pts',(2.525378983787,-2.605988952896,-2.38849844902));
#50721=CARTESIAN_POINT('Ctrl Pts',(1.359399658728,-3.364632223854,-2.434540115687));
#50722=CARTESIAN_POINT('Ctrl Pts',(-0.006333574545319,-3.628867222688,-2.480581782354));
#50723=CARTESIAN_POINT('Ctrl Pts',(-1.371136135038,-3.359866535032,-2.52662344902));
#50724=CARTESIAN_POINT('Ctrl Pts',(-2.534460197325,-2.597157858548,-2.572665115687));
#50725=CARTESIAN_POINT('Ctrl Pts',(-3.325363738216,-1.452815694643,-2.618706782354));
#50726=CARTESIAN_POINT('Ctrl Pts',(-3.627629225714,-0.09499281438667,-2.66474844902));
#50727=CARTESIAN_POINT('Ctrl Pts',(-3.396840941408,1.276788570131,-2.710790115687));
#50728=CARTESIAN_POINT('Ctrl Pts',(-2.66691154775,2.460955145979,-2.756831782354));
#50729=CARTESIAN_POINT('Ctrl Pts',(-1.545098868578,3.283502233951,-2.80287344902));
#50730=CARTESIAN_POINT('Ctrl Pts',(-0.1962451307805,3.623562512595,-2.848915115687));
#50731=CARTESIAN_POINT('Ctrl Pts',(1.181445403903,3.431166593396,-2.894956782354));
#50732=CARTESIAN_POINT('Ctrl Pts',(2.385531115837,2.73458565955,-2.94099844902));
#50733=CARTESIAN_POINT('Ctrl Pts',(3.239080353414,1.636177220892,-2.987040115687));
#50734=CARTESIAN_POINT('Ctrl Pts',(3.616670254429,0.2973444211245,-3.033081782354));
#50735=CARTESIAN_POINT('Ctrl Pts',(3.462816724887,-1.085180982088,-3.07912344902));
#50736=CARTESIAN_POINT('Ctrl Pts',(2.80012742371,-2.30824692029,-3.125165115687));
#50737=CARTESIAN_POINT('Ctrl Pts',(1.725979731427,-3.192132735452,-3.171206782354));
#50738=CARTESIAN_POINT('Ctrl Pts',(0.3982118512334,-3.606957825589,-3.21724844902));
#50739=CARTESIAN_POINT('Ctrl Pts',(-0.9880703687869,-3.491766656059,-3.263290115687));
#50740=CARTESIAN_POINT('Ctrl Pts',(-2.229162823228,-2.863485732736,-3.309331782354));
#50741=CARTESIAN_POINT('Ctrl Pts',(-3.142695988404,-1.814436374886,-3.35537344902));
#50742=CARTESIAN_POINT('Ctrl Pts',(-3.594432799537,-0.4987687677191,-3.401415115687));
#50743=CARTESIAN_POINT('Ctrl Pts',(-3.517993812628,0.8901892879335,-3.447456782354));
#50744=CARTESIAN_POINT('Ctrl Pts',(-2.924611181723,2.148340492051,-3.49349844902));
#50745=CARTESIAN_POINT('Ctrl Pts',(-1.90147817544,3.090808661559,-3.539540115687));
#50746=CARTESIAN_POINT('Ctrl Pts',(-0.598936759323,3.579104942911,-3.585581782354));
#50747=CARTESIAN_POINT('Ctrl Pts',(0.791614064251,3.541477743446,-3.63162344902));
#50748=CARTESIAN_POINT('Ctrl Pts',(2.065842949582,2.983456106884,-3.677665115687));
#50749=CARTESIAN_POINT('Ctrl Pts',(3.036511215093,1.98703726051,-3.723706782354));
#50750=CARTESIAN_POINT('Ctrl Pts',(3.560986207913,0.6986377180585,-3.76974844902));
#50751=CARTESIAN_POINT('Ctrl Pts',(3.562200136449,-0.6924215637334,-3.815790115687));
#50752=CARTESIAN_POINT('Ctrl Pts',(3.039974622718,-1.981734524923,-3.861831782354));
#50753=CARTESIAN_POINT('Ctrl Pts',(2.071046913695,-2.979845988523,-3.90787344902));
#50754=CARTESIAN_POINT('Ctrl Pts',(0.7977939001169,-3.540090722987,-3.953915115687));
#50755=CARTESIAN_POINT('Ctrl Pts',(-0.592689133709,-3.58014483294,-3.999956782354));
#50756=CARTESIAN_POINT('Ctrl Pts',(-1.896080803293,-3.094122657786,-4.04599844902));
#50757=CARTESIAN_POINT('Ctrl Pts',(-2.920857167686,-2.153441626797,-4.092040115687));
#50758=CARTESIAN_POINT('Ctrl Pts',(-3.516434781803,-0.8963279864901,-4.138081782354));
#50759=CARTESIAN_POINT('Ctrl Pts',(-3.595297840182,0.4924945425259,-4.18412344902));
#50760=CARTESIAN_POINT('Ctrl Pts',(-3.145857989081,1.808948574891,-4.230165115687));
#50761=CARTESIAN_POINT('Ctrl Pts',(-2.234157150885,2.859590750281,-4.276206782354));
#50762=CARTESIAN_POINT('Ctrl Pts',(-0.9941631432962,3.490036830591,-4.32224844902));
#50763=CARTESIAN_POINT('Ctrl Pts',(0.3919159190425,3.607647342181,-4.368290115687));
#50764=CARTESIAN_POINT('Ctrl Pts',(1.720405782322,3.195140275457,-4.414331782354));
#50765=CARTESIAN_POINT('Ctrl Pts',(2.796094511829,2.313130544526,-4.46037344902));
#50766=CARTESIAN_POINT('Ctrl Pts',(3.460917446918,1.091223088699,-4.506415115687));
#50767=CARTESIAN_POINT('Ctrl Pts',(3.617183734391,-0.2910317178534,-4.552456782354));
#50768=CARTESIAN_POINT('Ctrl Pts',(3.241930993927,-1.630521370031,-4.59849844902));
#50769=CARTESIAN_POINT('Ctrl Pts',(2.390300577984,-2.730418332625,-4.644540115687));
#50770=CARTESIAN_POINT('Ctrl Pts',(1.187430827056,-3.429097964413,-4.690581782354));
#50771=CARTESIAN_POINT('Ctrl Pts',(-0.1899157118936,-3.62390470395,-4.73662344902));
#50772=CARTESIAN_POINT('Ctrl Pts',(-1.539383690082,-3.286174537975,-4.782665115687));
#50773=CARTESIAN_POINT('Ctrl Pts',(-2.288158074621,-2.739177136089,-4.813359560131));
#50774=CARTESIAN_POINT('Ctrl Pts',(-2.59740372034,-2.405222217086,-4.828706782354));
#50775=CARTESIAN_POINT('Ctrl Pts',(-3.381685401913,-1.046806497156,-1.971293217646));
#50776=CARTESIAN_POINT('Ctrl Pts',(-3.516276022629,-0.6120144524515,-1.986640439869));
#50777=CARTESIAN_POINT('Ctrl Pts',(-3.615602476197,0.3099418872051,-2.017334884313));
#50778=CARTESIAN_POINT('Ctrl Pts',(-3.233351390461,1.647480520897,-2.06337655098));
#50779=CARTESIAN_POINT('Ctrl Pts',(-2.375970535719,2.742894243674,-2.109418217646));
#50780=CARTESIAN_POINT('Ctrl Pts',(-1.16946135002,3.435270189528,-2.155459884313));
#50781=CARTESIAN_POINT('Ctrl Pts',(0.2088925691034,3.622855283072,-2.20150155098));
#50782=CARTESIAN_POINT('Ctrl Pts',(1.556551006228,3.278088863066,-2.247543217646));
#50783=CARTESIAN_POINT('Ctrl Pts',(2.675485639469,2.451630885082,-2.293584884313));
#50784=CARTESIAN_POINT('Ctrl Pts',(3.401277069744,1.264923606363,-2.33962655098));
#50785=CARTESIAN_POINT('Ctrl Pts',(3.627275538361,-0.1076550254197,-2.385668217646));
#50786=CARTESIAN_POINT('Ctrl Pts',(3.320272205746,-1.464414529052,-2.431709884313));
#50787=CARTESIAN_POINT('Ctrl Pts',(2.525378983787,-2.605988952896,-2.47775155098));
#50788=CARTESIAN_POINT('Ctrl Pts',(1.359399658728,-3.364632223854,-2.523793217646));
#50789=CARTESIAN_POINT('Ctrl Pts',(-0.006333574545318,-3.628867222688,-2.569834884313));
#50790=CARTESIAN_POINT('Ctrl Pts',(-1.371136135038,-3.359866535032,-2.61587655098));
#50791=CARTESIAN_POINT('Ctrl Pts',(-2.534460197325,-2.597157858548,-2.661918217646));
#50792=CARTESIAN_POINT('Ctrl Pts',(-3.325363738216,-1.452815694643,-2.707959884313));
#50793=CARTESIAN_POINT('Ctrl Pts',(-3.627629225714,-0.09499281438668,-2.75400155098));
#50794=CARTESIAN_POINT('Ctrl Pts',(-3.396840941408,1.276788570131,-2.800043217646));
#50795=CARTESIAN_POINT('Ctrl Pts',(-2.66691154775,2.460955145979,-2.846084884313));
#50796=CARTESIAN_POINT('Ctrl Pts',(-1.545098868578,3.283502233951,-2.89212655098));
#50797=CARTESIAN_POINT('Ctrl Pts',(-0.1962451307805,3.623562512595,-2.938168217646));
#50798=CARTESIAN_POINT('Ctrl Pts',(1.181445403903,3.431166593396,-2.984209884313));
#50799=CARTESIAN_POINT('Ctrl Pts',(2.385531115837,2.73458565955,-3.03025155098));
#50800=CARTESIAN_POINT('Ctrl Pts',(3.239080353414,1.636177220892,-3.076293217646));
#50801=CARTESIAN_POINT('Ctrl Pts',(3.616670254429,0.2973444211246,-3.122334884313));
#50802=CARTESIAN_POINT('Ctrl Pts',(3.462816724887,-1.085180982089,-3.16837655098));
#50803=CARTESIAN_POINT('Ctrl Pts',(2.80012742371,-2.30824692029,-3.214418217646));
#50804=CARTESIAN_POINT('Ctrl Pts',(1.725979731427,-3.192132735452,-3.260459884313));
#50805=CARTESIAN_POINT('Ctrl Pts',(0.3982118512334,-3.606957825589,-3.30650155098));
#50806=CARTESIAN_POINT('Ctrl Pts',(-0.9880703687869,-3.491766656059,-3.352543217646));
#50807=CARTESIAN_POINT('Ctrl Pts',(-2.229162823228,-2.863485732736,-3.398584884313));
#50808=CARTESIAN_POINT('Ctrl Pts',(-3.142695988404,-1.814436374886,-3.44462655098));
#50809=CARTESIAN_POINT('Ctrl Pts',(-3.594432799537,-0.4987687677191,-3.490668217646));
#50810=CARTESIAN_POINT('Ctrl Pts',(-3.517993812628,0.8901892879335,-3.536709884313));
#50811=CARTESIAN_POINT('Ctrl Pts',(-2.924611181723,2.148340492051,-3.58275155098));
#50812=CARTESIAN_POINT('Ctrl Pts',(-1.90147817544,3.090808661559,-3.628793217646));
#50813=CARTESIAN_POINT('Ctrl Pts',(-0.598936759323,3.579104942911,-3.674834884313));
#50814=CARTESIAN_POINT('Ctrl Pts',(0.791614064251,3.541477743446,-3.72087655098));
#50815=CARTESIAN_POINT('Ctrl Pts',(2.065842949582,2.983456106884,-3.766918217646));
#50816=CARTESIAN_POINT('Ctrl Pts',(3.036511215093,1.98703726051,-3.812959884313));
#50817=CARTESIAN_POINT('Ctrl Pts',(3.560986207913,0.6986377180585,-3.85900155098));
#50818=CARTESIAN_POINT('Ctrl Pts',(3.562200136449,-0.6924215637334,-3.905043217646));
#50819=CARTESIAN_POINT('Ctrl Pts',(3.039974622718,-1.981734524923,-3.951084884313));
#50820=CARTESIAN_POINT('Ctrl Pts',(2.071046913695,-2.979845988523,-3.99712655098));
#50821=CARTESIAN_POINT('Ctrl Pts',(0.7977939001169,-3.540090722987,-4.043168217646));
#50822=CARTESIAN_POINT('Ctrl Pts',(-0.592689133709,-3.58014483294,-4.089209884313));
#50823=CARTESIAN_POINT('Ctrl Pts',(-1.896080803293,-3.094122657786,-4.13525155098));
#50824=CARTESIAN_POINT('Ctrl Pts',(-2.920857167686,-2.153441626797,-4.181293217646));
#50825=CARTESIAN_POINT('Ctrl Pts',(-3.516434781803,-0.8963279864901,-4.227334884313));
#50826=CARTESIAN_POINT('Ctrl Pts',(-3.595297840182,0.4924945425259,-4.27337655098));
#50827=CARTESIAN_POINT('Ctrl Pts',(-3.145857989081,1.808948574891,-4.319418217646));
#50828=CARTESIAN_POINT('Ctrl Pts',(-2.234157150885,2.859590750281,-4.365459884313));
#50829=CARTESIAN_POINT('Ctrl Pts',(-0.9941631432962,3.490036830591,-4.41150155098));
#50830=CARTESIAN_POINT('Ctrl Pts',(0.3919159190425,3.607647342181,-4.457543217646));
#50831=CARTESIAN_POINT('Ctrl Pts',(1.720405782322,3.195140275457,-4.503584884313));
#50832=CARTESIAN_POINT('Ctrl Pts',(2.796094511829,2.313130544526,-4.54962655098));
#50833=CARTESIAN_POINT('Ctrl Pts',(3.460917446918,1.091223088699,-4.595668217646));
#50834=CARTESIAN_POINT('Ctrl Pts',(3.617183734391,-0.2910317178534,-4.641709884313));
#50835=CARTESIAN_POINT('Ctrl Pts',(3.241930993927,-1.630521370031,-4.68775155098));
#50836=CARTESIAN_POINT('Ctrl Pts',(2.390300577984,-2.730418332625,-4.733793217646));
#50837=CARTESIAN_POINT('Ctrl Pts',(1.187430827056,-3.429097964413,-4.779834884313));
#50838=CARTESIAN_POINT('Ctrl Pts',(-0.1899157118936,-3.62390470395,-4.82587655098));
#50839=CARTESIAN_POINT('Ctrl Pts',(-1.539383690082,-3.286174537975,-4.871918217646));
#50840=CARTESIAN_POINT('Ctrl Pts',(-2.288158074621,-2.739177136089,-4.902612662091));
#50841=CARTESIAN_POINT('Ctrl Pts',(-2.59740372034,-2.405222217086,-4.917959884313));
#50842=CARTESIAN_POINT('Ctrl Pts',(-3.381685401913,-1.046806497156,-2.060546319606));
#50843=CARTESIAN_POINT('Ctrl Pts',(-3.516276022629,-0.6120144524515,-2.075893541828));
#50844=CARTESIAN_POINT('Ctrl Pts',(-3.615602476197,0.3099418872051,-2.106587986272));
#50845=CARTESIAN_POINT('Ctrl Pts',(-3.233351390461,1.647480520897,-2.152629652939));
#50846=CARTESIAN_POINT('Ctrl Pts',(-2.375970535719,2.742894243674,-2.198671319606));
#50847=CARTESIAN_POINT('Ctrl Pts',(-1.16946135002,3.435270189528,-2.244712986272));
#50848=CARTESIAN_POINT('Ctrl Pts',(0.2088925691034,3.622855283072,-2.290754652939));
#50849=CARTESIAN_POINT('Ctrl Pts',(1.556551006228,3.278088863066,-2.336796319606));
#50850=CARTESIAN_POINT('Ctrl Pts',(2.675485639469,2.451630885082,-2.382837986272));
#50851=CARTESIAN_POINT('Ctrl Pts',(3.401277069744,1.264923606363,-2.428879652939));
#50852=CARTESIAN_POINT('Ctrl Pts',(3.627275538361,-0.1076550254197,-2.474921319606));
#50853=CARTESIAN_POINT('Ctrl Pts',(3.320272205746,-1.464414529052,-2.520962986272));
#50854=CARTESIAN_POINT('Ctrl Pts',(2.525378983787,-2.605988952896,-2.567004652939));
#50855=CARTESIAN_POINT('Ctrl Pts',(1.359399658728,-3.364632223854,-2.613046319606));
#50856=CARTESIAN_POINT('Ctrl Pts',(-0.006333574545318,-3.628867222688,-2.659087986272));
#50857=CARTESIAN_POINT('Ctrl Pts',(-1.371136135038,-3.359866535032,-2.705129652939));
#50858=CARTESIAN_POINT('Ctrl Pts',(-2.534460197325,-2.597157858548,-2.751171319606));
#50859=CARTESIAN_POINT('Ctrl Pts',(-3.325363738216,-1.452815694643,-2.797212986272));
#50860=CARTESIAN_POINT('Ctrl Pts',(-3.627629225714,-0.09499281438668,-2.843254652939));
#50861=CARTESIAN_POINT('Ctrl Pts',(-3.396840941408,1.276788570131,-2.889296319606));
#50862=CARTESIAN_POINT('Ctrl Pts',(-2.66691154775,2.460955145979,-2.935337986272));
#50863=CARTESIAN_POINT('Ctrl Pts',(-1.545098868578,3.283502233951,-2.981379652939));
#50864=CARTESIAN_POINT('Ctrl Pts',(-0.1962451307805,3.623562512595,-3.027421319606));
#50865=CARTESIAN_POINT('Ctrl Pts',(1.181445403903,3.431166593396,-3.073462986272));
#50866=CARTESIAN_POINT('Ctrl Pts',(2.385531115837,2.73458565955,-3.119504652939));
#50867=CARTESIAN_POINT('Ctrl Pts',(3.239080353414,1.636177220892,-3.165546319606));
#50868=CARTESIAN_POINT('Ctrl Pts',(3.616670254429,0.2973444211246,-3.211587986272));
#50869=CARTESIAN_POINT('Ctrl Pts',(3.462816724887,-1.085180982089,-3.257629652939));
#50870=CARTESIAN_POINT('Ctrl Pts',(2.80012742371,-2.30824692029,-3.303671319606));
#50871=CARTESIAN_POINT('Ctrl Pts',(1.725979731427,-3.192132735452,-3.349712986272));
#50872=CARTESIAN_POINT('Ctrl Pts',(0.3982118512334,-3.606957825589,-3.395754652939));
#50873=CARTESIAN_POINT('Ctrl Pts',(-0.9880703687869,-3.491766656059,-3.441796319606));
#50874=CARTESIAN_POINT('Ctrl Pts',(-2.229162823228,-2.863485732736,-3.487837986272));
#50875=CARTESIAN_POINT('Ctrl Pts',(-3.142695988404,-1.814436374886,-3.533879652939));
#50876=CARTESIAN_POINT('Ctrl Pts',(-3.594432799537,-0.4987687677191,-3.579921319606));
#50877=CARTESIAN_POINT('Ctrl Pts',(-3.517993812628,0.8901892879335,-3.625962986272));
#50878=CARTESIAN_POINT('Ctrl Pts',(-2.924611181723,2.148340492051,-3.672004652939));
#50879=CARTESIAN_POINT('Ctrl Pts',(-1.90147817544,3.090808661559,-3.718046319606));
#50880=CARTESIAN_POINT('Ctrl Pts',(-0.598936759323,3.579104942911,-3.764087986272));
#50881=CARTESIAN_POINT('Ctrl Pts',(0.791614064251,3.541477743446,-3.810129652939));
#50882=CARTESIAN_POINT('Ctrl Pts',(2.065842949582,2.983456106884,-3.856171319606));
#50883=CARTESIAN_POINT('Ctrl Pts',(3.036511215093,1.98703726051,-3.902212986272));
#50884=CARTESIAN_POINT('Ctrl Pts',(3.560986207913,0.6986377180585,-3.948254652939));
#50885=CARTESIAN_POINT('Ctrl Pts',(3.562200136449,-0.6924215637334,-3.994296319606));
#50886=CARTESIAN_POINT('Ctrl Pts',(3.039974622718,-1.981734524923,-4.040337986272));
#50887=CARTESIAN_POINT('Ctrl Pts',(2.071046913695,-2.979845988523,-4.086379652939));
#50888=CARTESIAN_POINT('Ctrl Pts',(0.7977939001169,-3.540090722987,-4.132421319606));
#50889=CARTESIAN_POINT('Ctrl Pts',(-0.592689133709,-3.58014483294,-4.178462986272));
#50890=CARTESIAN_POINT('Ctrl Pts',(-1.896080803293,-3.094122657786,-4.224504652939));
#50891=CARTESIAN_POINT('Ctrl Pts',(-2.920857167686,-2.153441626797,-4.270546319606));
#50892=CARTESIAN_POINT('Ctrl Pts',(-3.516434781803,-0.8963279864901,-4.316587986272));
#50893=CARTESIAN_POINT('Ctrl Pts',(-3.595297840182,0.4924945425259,-4.362629652939));
#50894=CARTESIAN_POINT('Ctrl Pts',(-3.145857989081,1.808948574891,-4.408671319606));
#50895=CARTESIAN_POINT('Ctrl Pts',(-2.234157150885,2.859590750281,-4.454712986272));
#50896=CARTESIAN_POINT('Ctrl Pts',(-0.9941631432962,3.490036830591,-4.500754652939));
#50897=CARTESIAN_POINT('Ctrl Pts',(0.3919159190425,3.607647342181,-4.546796319606));
#50898=CARTESIAN_POINT('Ctrl Pts',(1.720405782322,3.195140275457,-4.592837986272));
#50899=CARTESIAN_POINT('Ctrl Pts',(2.796094511829,2.313130544526,-4.638879652939));
#50900=CARTESIAN_POINT('Ctrl Pts',(3.460917446918,1.091223088699,-4.684921319606));
#50901=CARTESIAN_POINT('Ctrl Pts',(3.617183734391,-0.2910317178534,-4.730962986272));
#50902=CARTESIAN_POINT('Ctrl Pts',(3.241930993927,-1.630521370031,-4.777004652939));
#50903=CARTESIAN_POINT('Ctrl Pts',(2.390300577984,-2.730418332625,-4.823046319606));
#50904=CARTESIAN_POINT('Ctrl Pts',(1.187430827056,-3.429097964413,-4.869087986272));
#50905=CARTESIAN_POINT('Ctrl Pts',(-0.1899157118936,-3.62390470395,-4.915129652939));
#50906=CARTESIAN_POINT('Ctrl Pts',(-1.539383690082,-3.286174537975,-4.961171319606));
#50907=CARTESIAN_POINT('Ctrl Pts',(-2.288158074621,-2.739177136089,-4.99186576405));
#50908=CARTESIAN_POINT('Ctrl Pts',(-2.59740372034,-2.405222217086,-5.007212986272));
#50909=CARTESIAN_POINT('',(-1.210751307373,-3.326511877582,-4.707247790494));
#50910=CARTESIAN_POINT('Ctrl Pts',(0.4436796468176,-3.512086042653,-4.626120347061));
#50911=CARTESIAN_POINT('Ctrl Pts',(-0.007878345773629,-3.56913108319,-4.641467569283));
#50912=CARTESIAN_POINT('Ctrl Pts',(-0.9330759546625,-3.506852506473,-4.672162013728));
#50913=CARTESIAN_POINT('Ctrl Pts',(-2.183917166627,-2.898147527343,-4.718203680394));
#50914=CARTESIAN_POINT('Ctrl Pts',(-3.113806470581,-1.863575617557,-4.764245347061));
#50915=CARTESIAN_POINT('Ctrl Pts',(-3.586155548622,-0.555166196143,-4.810287013728));
#50916=CARTESIAN_POINT('Ctrl Pts',(-3.531542156858,0.8348212394562,-4.856328680394));
#50917=CARTESIAN_POINT('Ctrl Pts',(-2.957995081733,2.102137656194,-4.902370347061));
#50918=CARTESIAN_POINT('Ctrl Pts',(-1.949791897485,3.060560236328,-4.948412013728));
#50919=CARTESIAN_POINT('Ctrl Pts',(-0.6550810096133,3.56925570756,-4.994453680394));
#50920=CARTESIAN_POINT('Ctrl Pts',(0.7358892908163,3.553474973509,-5.040495347061));
#50921=CARTESIAN_POINT('Ctrl Pts',(2.01872599972,3.01553689601,-5.086537013728));
#50922=CARTESIAN_POINT('Ctrl Pts',(3.004925583529,2.034487569837,-5.132578680394));
#50923=CARTESIAN_POINT('Ctrl Pts',(3.549573173545,0.754485069166,-5.178620347061));
#50924=CARTESIAN_POINT('Ctrl Pts',(3.572636761877,-0.6363835335316,-5.224662013728));
#50925=CARTESIAN_POINT('Ctrl Pts',(3.070727321603,-1.933740197233,-5.270703680394));
#50926=CARTESIAN_POINT('Ctrl Pts',(2.11759680026,-2.946947781277,-5.316745347061));
#50927=CARTESIAN_POINT('Ctrl Pts',(0.8533008065619,-3.527122788841,-5.362787013728));
#50928=CARTESIAN_POINT('Ctrl Pts',(-0.5363815442081,-3.589012715647,-5.408828680394));
#50929=CARTESIAN_POINT('Ctrl Pts',(-1.847246522122,-3.123523286379,-5.454870347061));
#50930=CARTESIAN_POINT('Ctrl Pts',(-2.886672037841,-2.199054792402,-5.500912013728));
#50931=CARTESIAN_POINT('Ctrl Pts',(-3.501922059872,-0.9514511656551,-5.546953680394));
#50932=CARTESIAN_POINT('Ctrl Pts',(-3.602590065264,0.4359613006909,-5.592995347061));
#50933=CARTESIAN_POINT('Ctrl Pts',(-3.173883621652,1.75931241974,-5.639037013728));
#50934=CARTESIAN_POINT('Ctrl Pts',(-2.278798027768,2.824145354383,-5.685078680394));
#50935=CARTESIAN_POINT('Ctrl Pts',(-1.04885961175,3.47399063742,-5.731120347061));
#50936=CARTESIAN_POINT('Ctrl Pts',(0.3352011076653,3.613358223518,-5.777162013728));
#50937=CARTESIAN_POINT('Ctrl Pts',(1.670006458453,3.22176905795,-5.823203680394));
#50938=CARTESIAN_POINT('Ctrl Pts',(2.75941648733,2.356764324978,-5.869245347061));
#50939=CARTESIAN_POINT('Ctrl Pts',(3.44335030157,1.145450188669,-5.915287013728));
#50940=CARTESIAN_POINT('Ctrl Pts',(3.62130879372,-0.2341795348991,-5.961328680394));
#50941=CARTESIAN_POINT('Ctrl Pts',(3.26714225565,-1.579398276366,-6.007370347061));
#50942=CARTESIAN_POINT('Ctrl Pts',(2.432892888262,-2.692535910306,-6.053412013728));
#50943=CARTESIAN_POINT('Ctrl Pts',(1.241147577988,-3.410024944732,-6.099453680394));
#50944=CARTESIAN_POINT('Ctrl Pts',(-0.1329753559758,-3.626435576257,-6.145495347061));
#50945=CARTESIAN_POINT('Ctrl Pts',(-1.487558527012,-3.309967834097,-6.191537013728));
#50946=CARTESIAN_POINT('Ctrl Pts',(-2.623555774772,-2.507124354854,-6.237578680394));
#50947=CARTESIAN_POINT('Ctrl Pts',(-3.374040553019,-1.33587715776,-6.283620347061));
#50948=CARTESIAN_POINT('Ctrl Pts',(-3.628734573418,0.03166748686997,-6.329662013728));
#50949=CARTESIAN_POINT('Ctrl Pts',(-3.350212399193,1.394558824265,-6.375703680394));
#50950=CARTESIAN_POINT('Ctrl Pts',(-2.57940084129,2.552529869363,-6.421745347061));
#50951=CARTESIAN_POINT('Ctrl Pts',(-1.429565060708,3.335425185976,-6.467787013728));
#50952=CARTESIAN_POINT('Ctrl Pts',(-0.06966507558956,3.628203992513,-6.513828680394));
#50953=CARTESIAN_POINT('Ctrl Pts',(1.300471686497,3.387844569437,-6.559870347061));
#50954=CARTESIAN_POINT('Ctrl Pts',(2.479513577945,2.649665988541,-6.605912013728));
#50955=CARTESIAN_POINT('Ctrl Pts',(3.294208954705,1.522138231824,-6.651953680394));
#50956=CARTESIAN_POINT('Ctrl Pts',(3.624844247273,0.1709433153187,-6.697995347061));
#50957=CARTESIAN_POINT('Ctrl Pts',(3.422835000394,-1.205370480026,-6.744037013728));
#50958=CARTESIAN_POINT('Ctrl Pts',(2.717865005957,-2.404563836423,-6.790078680394));
#50959=CARTESIAN_POINT('Ctrl Pts',(1.613524485334,-3.250423998384,-6.836120347061));
#50960=CARTESIAN_POINT('Ctrl Pts',(0.2720882585925,-3.618657957528,-6.882162013728));
#50961=CARTESIAN_POINT('Ctrl Pts',(-1.109329361913,-3.455156407579,-6.928203680394));
#50962=CARTESIAN_POINT('Ctrl Pts',(-2.327739088356,-2.783944714,-6.974245347061));
#50963=CARTESIAN_POINT('Ctrl Pts',(-3.204104459192,-1.70365256098,-7.020287013728));
#50964=CARTESIAN_POINT('Ctrl Pts',(-3.609649947201,-0.3730210356546,-7.066328680394));
#50965=CARTESIAN_POINT('Ctrl Pts',(-3.484783587573,1.012423222237,-7.112370347061));
#50966=CARTESIAN_POINT('Ctrl Pts',(-2.847853586283,2.249099238981,-7.158412013728));
#50967=CARTESIAN_POINT('Ctrl Pts',(-1.792452177415,3.155286457167,-7.204453680394));
#50968=CARTESIAN_POINT('Ctrl Pts',(-0.4736629503042,3.597827235041,-7.250495347061));
#50969=CARTESIAN_POINT('Ctrl Pts',(0.9147276558781,3.51169345825,-7.296537013728));
#50970=CARTESIAN_POINT('Ctrl Pts',(2.168705495876,2.909541712997,-7.342578680394));
#50971=CARTESIAN_POINT('Ctrl Pts',(3.104008482379,1.8798543735,-7.388620347061));
#50972=CARTESIAN_POINT('Ctrl Pts',(3.583197460416,0.5739344720891,-7.434662013728));
#50973=CARTESIAN_POINT('Ctrl Pts',(3.535870931347,-0.8163149133711,-7.480703680394));
#50974=CARTESIAN_POINT('Ctrl Pts',(2.968938990236,-2.086635212868,-7.526745347061));
#50975=CARTESIAN_POINT('Ctrl Pts',(2.300228400622,-2.729048929993,-7.557439791506));
#50976=CARTESIAN_POINT('Ctrl Pts',(1.917647064401,-2.975605776375,-7.572787013728));
#50977=CARTESIAN_POINT('Ctrl Pts',(0.4436796468176,-3.512086042653,-4.71537344902));
#50978=CARTESIAN_POINT('Ctrl Pts',(-0.007878345773629,-3.56913108319,-4.730720671243));
#50979=CARTESIAN_POINT('Ctrl Pts',(-0.9330759546625,-3.506852506473,-4.761415115687));
#50980=CARTESIAN_POINT('Ctrl Pts',(-2.183917166627,-2.898147527343,-4.807456782354));
#50981=CARTESIAN_POINT('Ctrl Pts',(-3.113806470581,-1.863575617557,-4.85349844902));
#50982=CARTESIAN_POINT('Ctrl Pts',(-3.586155548622,-0.555166196143,-4.899540115687));
#50983=CARTESIAN_POINT('Ctrl Pts',(-3.531542156858,0.8348212394562,-4.945581782354));
#50984=CARTESIAN_POINT('Ctrl Pts',(-2.957995081733,2.102137656194,-4.99162344902));
#50985=CARTESIAN_POINT('Ctrl Pts',(-1.949791897485,3.060560236328,-5.037665115687));
#50986=CARTESIAN_POINT('Ctrl Pts',(-0.6550810096133,3.56925570756,-5.083706782354));
#50987=CARTESIAN_POINT('Ctrl Pts',(0.7358892908163,3.553474973509,-5.12974844902));
#50988=CARTESIAN_POINT('Ctrl Pts',(2.01872599972,3.01553689601,-5.175790115687));
#50989=CARTESIAN_POINT('Ctrl Pts',(3.004925583529,2.034487569837,-5.221831782354));
#50990=CARTESIAN_POINT('Ctrl Pts',(3.549573173545,0.754485069166,-5.26787344902));
#50991=CARTESIAN_POINT('Ctrl Pts',(3.572636761877,-0.6363835335316,-5.313915115687));
#50992=CARTESIAN_POINT('Ctrl Pts',(3.070727321603,-1.933740197233,-5.359956782354));
#50993=CARTESIAN_POINT('Ctrl Pts',(2.11759680026,-2.946947781277,-5.40599844902));
#50994=CARTESIAN_POINT('Ctrl Pts',(0.8533008065619,-3.527122788841,-5.452040115687));
#50995=CARTESIAN_POINT('Ctrl Pts',(-0.5363815442081,-3.589012715647,-5.498081782354));
#50996=CARTESIAN_POINT('Ctrl Pts',(-1.847246522122,-3.123523286379,-5.54412344902));
#50997=CARTESIAN_POINT('Ctrl Pts',(-2.886672037841,-2.199054792402,-5.590165115687));
#50998=CARTESIAN_POINT('Ctrl Pts',(-3.501922059872,-0.9514511656551,-5.636206782354));
#50999=CARTESIAN_POINT('Ctrl Pts',(-3.602590065264,0.4359613006909,-5.68224844902));
#51000=CARTESIAN_POINT('Ctrl Pts',(-3.173883621652,1.75931241974,-5.728290115687));
#51001=CARTESIAN_POINT('Ctrl Pts',(-2.278798027768,2.824145354383,-5.774331782354));
#51002=CARTESIAN_POINT('Ctrl Pts',(-1.04885961175,3.47399063742,-5.82037344902));
#51003=CARTESIAN_POINT('Ctrl Pts',(0.3352011076653,3.613358223518,-5.866415115687));
#51004=CARTESIAN_POINT('Ctrl Pts',(1.670006458453,3.22176905795,-5.912456782354));
#51005=CARTESIAN_POINT('Ctrl Pts',(2.75941648733,2.356764324978,-5.95849844902));
#51006=CARTESIAN_POINT('Ctrl Pts',(3.44335030157,1.145450188669,-6.004540115687));
#51007=CARTESIAN_POINT('Ctrl Pts',(3.62130879372,-0.2341795348991,-6.050581782354));
#51008=CARTESIAN_POINT('Ctrl Pts',(3.26714225565,-1.579398276366,-6.09662344902));
#51009=CARTESIAN_POINT('Ctrl Pts',(2.432892888262,-2.692535910306,-6.142665115687));
#51010=CARTESIAN_POINT('Ctrl Pts',(1.241147577988,-3.410024944732,-6.188706782354));
#51011=CARTESIAN_POINT('Ctrl Pts',(-0.1329753559758,-3.626435576257,-6.23474844902));
#51012=CARTESIAN_POINT('Ctrl Pts',(-1.487558527012,-3.309967834097,-6.280790115687));
#51013=CARTESIAN_POINT('Ctrl Pts',(-2.623555774772,-2.507124354854,-6.326831782354));
#51014=CARTESIAN_POINT('Ctrl Pts',(-3.374040553019,-1.33587715776,-6.37287344902));
#51015=CARTESIAN_POINT('Ctrl Pts',(-3.628734573418,0.03166748686997,-6.418915115687));
#51016=CARTESIAN_POINT('Ctrl Pts',(-3.350212399193,1.394558824265,-6.464956782354));
#51017=CARTESIAN_POINT('Ctrl Pts',(-2.57940084129,2.552529869363,-6.51099844902));
#51018=CARTESIAN_POINT('Ctrl Pts',(-1.429565060708,3.335425185976,-6.557040115687));
#51019=CARTESIAN_POINT('Ctrl Pts',(-0.06966507558956,3.628203992513,-6.603081782354));
#51020=CARTESIAN_POINT('Ctrl Pts',(1.300471686497,3.387844569437,-6.64912344902));
#51021=CARTESIAN_POINT('Ctrl Pts',(2.479513577945,2.649665988541,-6.695165115687));
#51022=CARTESIAN_POINT('Ctrl Pts',(3.294208954705,1.522138231824,-6.741206782354));
#51023=CARTESIAN_POINT('Ctrl Pts',(3.624844247273,0.1709433153187,-6.78724844902));
#51024=CARTESIAN_POINT('Ctrl Pts',(3.422835000394,-1.205370480026,-6.833290115687));
#51025=CARTESIAN_POINT('Ctrl Pts',(2.717865005957,-2.404563836423,-6.879331782354));
#51026=CARTESIAN_POINT('Ctrl Pts',(1.613524485334,-3.250423998384,-6.92537344902));
#51027=CARTESIAN_POINT('Ctrl Pts',(0.2720882585925,-3.618657957528,-6.971415115687));
#51028=CARTESIAN_POINT('Ctrl Pts',(-1.109329361913,-3.455156407579,-7.017456782354));
#51029=CARTESIAN_POINT('Ctrl Pts',(-2.327739088356,-2.783944714,-7.06349844902));
#51030=CARTESIAN_POINT('Ctrl Pts',(-3.204104459192,-1.70365256098,-7.109540115687));
#51031=CARTESIAN_POINT('Ctrl Pts',(-3.609649947201,-0.3730210356546,-7.155581782354));
#51032=CARTESIAN_POINT('Ctrl Pts',(-3.484783587573,1.012423222237,-7.20162344902));
#51033=CARTESIAN_POINT('Ctrl Pts',(-2.847853586283,2.249099238981,-7.247665115687));
#51034=CARTESIAN_POINT('Ctrl Pts',(-1.792452177415,3.155286457167,-7.293706782354));
#51035=CARTESIAN_POINT('Ctrl Pts',(-0.4736629503042,3.597827235041,-7.33974844902));
#51036=CARTESIAN_POINT('Ctrl Pts',(0.9147276558781,3.51169345825,-7.385790115687));
#51037=CARTESIAN_POINT('Ctrl Pts',(2.168705495876,2.909541712997,-7.431831782354));
#51038=CARTESIAN_POINT('Ctrl Pts',(3.104008482379,1.8798543735,-7.47787344902));
#51039=CARTESIAN_POINT('Ctrl Pts',(3.583197460416,0.5739344720891,-7.523915115687));
#51040=CARTESIAN_POINT('Ctrl Pts',(3.535870931347,-0.8163149133711,-7.569956782354));
#51041=CARTESIAN_POINT('Ctrl Pts',(2.968938990236,-2.086635212868,-7.61599844902));
#51042=CARTESIAN_POINT('Ctrl Pts',(2.300228400622,-2.729048929993,-7.646692893465));
#51043=CARTESIAN_POINT('Ctrl Pts',(1.917647064401,-2.975605776375,-7.662040115687));
#51044=CARTESIAN_POINT('Ctrl Pts',(0.4436796468176,-3.512086042653,-4.80462655098));
#51045=CARTESIAN_POINT('Ctrl Pts',(-0.007878345773629,-3.56913108319,-4.819973773202));
#51046=CARTESIAN_POINT('Ctrl Pts',(-0.9330759546625,-3.506852506473,-4.850668217646));
#51047=CARTESIAN_POINT('Ctrl Pts',(-2.183917166627,-2.898147527343,-4.896709884313));
#51048=CARTESIAN_POINT('Ctrl Pts',(-3.113806470581,-1.863575617557,-4.94275155098));
#51049=CARTESIAN_POINT('Ctrl Pts',(-3.586155548622,-0.555166196143,-4.988793217646));
#51050=CARTESIAN_POINT('Ctrl Pts',(-3.531542156858,0.8348212394562,-5.034834884313));
#51051=CARTESIAN_POINT('Ctrl Pts',(-2.957995081733,2.102137656194,-5.08087655098));
#51052=CARTESIAN_POINT('Ctrl Pts',(-1.949791897485,3.060560236328,-5.126918217646));
#51053=CARTESIAN_POINT('Ctrl Pts',(-0.6550810096133,3.56925570756,-5.172959884313));
#51054=CARTESIAN_POINT('Ctrl Pts',(0.7358892908163,3.553474973509,-5.21900155098));
#51055=CARTESIAN_POINT('Ctrl Pts',(2.01872599972,3.01553689601,-5.265043217646));
#51056=CARTESIAN_POINT('Ctrl Pts',(3.004925583529,2.034487569837,-5.311084884313));
#51057=CARTESIAN_POINT('Ctrl Pts',(3.549573173545,0.754485069166,-5.35712655098));
#51058=CARTESIAN_POINT('Ctrl Pts',(3.572636761877,-0.6363835335316,-5.403168217646));
#51059=CARTESIAN_POINT('Ctrl Pts',(3.070727321603,-1.933740197233,-5.449209884313));
#51060=CARTESIAN_POINT('Ctrl Pts',(2.11759680026,-2.946947781277,-5.49525155098));
#51061=CARTESIAN_POINT('Ctrl Pts',(0.8533008065619,-3.527122788841,-5.541293217646));
#51062=CARTESIAN_POINT('Ctrl Pts',(-0.5363815442082,-3.589012715647,-5.587334884313));
#51063=CARTESIAN_POINT('Ctrl Pts',(-1.847246522122,-3.123523286379,-5.63337655098));
#51064=CARTESIAN_POINT('Ctrl Pts',(-2.886672037841,-2.199054792402,-5.679418217646));
#51065=CARTESIAN_POINT('Ctrl Pts',(-3.501922059872,-0.9514511656551,-5.725459884313));
#51066=CARTESIAN_POINT('Ctrl Pts',(-3.602590065264,0.4359613006909,-5.77150155098));
#51067=CARTESIAN_POINT('Ctrl Pts',(-3.173883621652,1.75931241974,-5.817543217646));
#51068=CARTESIAN_POINT('Ctrl Pts',(-2.278798027768,2.824145354383,-5.863584884313));
#51069=CARTESIAN_POINT('Ctrl Pts',(-1.04885961175,3.47399063742,-5.90962655098));
#51070=CARTESIAN_POINT('Ctrl Pts',(0.3352011076653,3.613358223518,-5.955668217646));
#51071=CARTESIAN_POINT('Ctrl Pts',(1.670006458453,3.22176905795,-6.001709884313));
#51072=CARTESIAN_POINT('Ctrl Pts',(2.75941648733,2.356764324978,-6.04775155098));
#51073=CARTESIAN_POINT('Ctrl Pts',(3.44335030157,1.145450188669,-6.093793217646));
#51074=CARTESIAN_POINT('Ctrl Pts',(3.62130879372,-0.2341795348991,-6.139834884313));
#51075=CARTESIAN_POINT('Ctrl Pts',(3.26714225565,-1.579398276366,-6.18587655098));
#51076=CARTESIAN_POINT('Ctrl Pts',(2.432892888262,-2.692535910306,-6.231918217646));
#51077=CARTESIAN_POINT('Ctrl Pts',(1.241147577988,-3.410024944732,-6.277959884313));
#51078=CARTESIAN_POINT('Ctrl Pts',(-0.1329753559758,-3.626435576257,-6.32400155098));
#51079=CARTESIAN_POINT('Ctrl Pts',(-1.487558527012,-3.309967834097,-6.370043217646));
#51080=CARTESIAN_POINT('Ctrl Pts',(-2.623555774772,-2.507124354854,-6.416084884313));
#51081=CARTESIAN_POINT('Ctrl Pts',(-3.374040553019,-1.33587715776,-6.46212655098));
#51082=CARTESIAN_POINT('Ctrl Pts',(-3.628734573418,0.03166748686998,-6.508168217646));
#51083=CARTESIAN_POINT('Ctrl Pts',(-3.350212399193,1.394558824265,-6.554209884313));
#51084=CARTESIAN_POINT('Ctrl Pts',(-2.57940084129,2.552529869363,-6.60025155098));
#51085=CARTESIAN_POINT('Ctrl Pts',(-1.429565060708,3.335425185976,-6.646293217646));
#51086=CARTESIAN_POINT('Ctrl Pts',(-0.06966507558957,3.628203992513,-6.692334884313));
#51087=CARTESIAN_POINT('Ctrl Pts',(1.300471686497,3.387844569437,-6.73837655098));
#51088=CARTESIAN_POINT('Ctrl Pts',(2.479513577945,2.649665988541,-6.784418217646));
#51089=CARTESIAN_POINT('Ctrl Pts',(3.294208954705,1.522138231824,-6.830459884313));
#51090=CARTESIAN_POINT('Ctrl Pts',(3.624844247273,0.1709433153187,-6.87650155098));
#51091=CARTESIAN_POINT('Ctrl Pts',(3.422835000394,-1.205370480026,-6.922543217646));
#51092=CARTESIAN_POINT('Ctrl Pts',(2.717865005957,-2.404563836423,-6.968584884313));
#51093=CARTESIAN_POINT('Ctrl Pts',(1.613524485334,-3.250423998384,-7.01462655098));
#51094=CARTESIAN_POINT('Ctrl Pts',(0.2720882585925,-3.618657957528,-7.060668217646));
#51095=CARTESIAN_POINT('Ctrl Pts',(-1.109329361913,-3.455156407579,-7.106709884313));
#51096=CARTESIAN_POINT('Ctrl Pts',(-2.327739088356,-2.783944714,-7.15275155098));
#51097=CARTESIAN_POINT('Ctrl Pts',(-3.204104459192,-1.70365256098,-7.198793217646));
#51098=CARTESIAN_POINT('Ctrl Pts',(-3.609649947201,-0.3730210356546,-7.244834884313));
#51099=CARTESIAN_POINT('Ctrl Pts',(-3.484783587573,1.012423222237,-7.29087655098));
#51100=CARTESIAN_POINT('Ctrl Pts',(-2.847853586283,2.249099238981,-7.336918217646));
#51101=CARTESIAN_POINT('Ctrl Pts',(-1.792452177415,3.155286457167,-7.382959884313));
#51102=CARTESIAN_POINT('Ctrl Pts',(-0.4736629503042,3.597827235041,-7.42900155098));
#51103=CARTESIAN_POINT('Ctrl Pts',(0.9147276558781,3.51169345825,-7.475043217646));
#51104=CARTESIAN_POINT('Ctrl Pts',(2.168705495876,2.909541712997,-7.521084884313));
#51105=CARTESIAN_POINT('Ctrl Pts',(3.104008482379,1.8798543735,-7.56712655098));
#51106=CARTESIAN_POINT('Ctrl Pts',(3.583197460416,0.5739344720891,-7.613168217646));
#51107=CARTESIAN_POINT('Ctrl Pts',(3.535870931347,-0.8163149133711,-7.659209884313));
#51108=CARTESIAN_POINT('Ctrl Pts',(2.968938990236,-2.086635212868,-7.70525155098));
#51109=CARTESIAN_POINT('Ctrl Pts',(2.300228400622,-2.729048929993,-7.735945995424));
#51110=CARTESIAN_POINT('Ctrl Pts',(1.917647064401,-2.975605776375,-7.751293217646));
#51111=CARTESIAN_POINT('Ctrl Pts',(0.4436796468176,-3.512086042653,-4.893879652939));
#51112=CARTESIAN_POINT('Ctrl Pts',(-0.007878345773629,-3.56913108319,-4.909226875161));
#51113=CARTESIAN_POINT('Ctrl Pts',(-0.9330759546625,-3.506852506473,-4.939921319606));
#51114=CARTESIAN_POINT('Ctrl Pts',(-2.183917166627,-2.898147527343,-4.985962986272));
#51115=CARTESIAN_POINT('Ctrl Pts',(-3.113806470581,-1.863575617557,-5.032004652939));
#51116=CARTESIAN_POINT('Ctrl Pts',(-3.586155548622,-0.555166196143,-5.078046319606));
#51117=CARTESIAN_POINT('Ctrl Pts',(-3.531542156858,0.8348212394562,-5.124087986272));
#51118=CARTESIAN_POINT('Ctrl Pts',(-2.957995081733,2.102137656194,-5.170129652939));
#51119=CARTESIAN_POINT('Ctrl Pts',(-1.949791897485,3.060560236328,-5.216171319606));
#51120=CARTESIAN_POINT('Ctrl Pts',(-0.6550810096133,3.56925570756,-5.262212986272));
#51121=CARTESIAN_POINT('Ctrl Pts',(0.7358892908163,3.553474973509,-5.308254652939));
#51122=CARTESIAN_POINT('Ctrl Pts',(2.01872599972,3.01553689601,-5.354296319606));
#51123=CARTESIAN_POINT('Ctrl Pts',(3.004925583529,2.034487569837,-5.400337986272));
#51124=CARTESIAN_POINT('Ctrl Pts',(3.549573173545,0.754485069166,-5.446379652939));
#51125=CARTESIAN_POINT('Ctrl Pts',(3.572636761877,-0.6363835335316,-5.492421319606));
#51126=CARTESIAN_POINT('Ctrl Pts',(3.070727321603,-1.933740197233,-5.538462986272));
#51127=CARTESIAN_POINT('Ctrl Pts',(2.11759680026,-2.946947781277,-5.584504652939));
#51128=CARTESIAN_POINT('Ctrl Pts',(0.8533008065619,-3.527122788841,-5.630546319606));
#51129=CARTESIAN_POINT('Ctrl Pts',(-0.5363815442082,-3.589012715647,-5.676587986272));
#51130=CARTESIAN_POINT('Ctrl Pts',(-1.847246522122,-3.123523286379,-5.722629652939));
#51131=CARTESIAN_POINT('Ctrl Pts',(-2.886672037841,-2.199054792402,-5.768671319606));
#51132=CARTESIAN_POINT('Ctrl Pts',(-3.501922059872,-0.9514511656551,-5.814712986272));
#51133=CARTESIAN_POINT('Ctrl Pts',(-3.602590065264,0.4359613006909,-5.860754652939));
#51134=CARTESIAN_POINT('Ctrl Pts',(-3.173883621652,1.75931241974,-5.906796319606));
#51135=CARTESIAN_POINT('Ctrl Pts',(-2.278798027768,2.824145354383,-5.952837986272));
#51136=CARTESIAN_POINT('Ctrl Pts',(-1.04885961175,3.47399063742,-5.998879652939));
#51137=CARTESIAN_POINT('Ctrl Pts',(0.3352011076653,3.613358223518,-6.044921319606));
#51138=CARTESIAN_POINT('Ctrl Pts',(1.670006458453,3.22176905795,-6.090962986272));
#51139=CARTESIAN_POINT('Ctrl Pts',(2.75941648733,2.356764324978,-6.137004652939));
#51140=CARTESIAN_POINT('Ctrl Pts',(3.44335030157,1.145450188669,-6.183046319606));
#51141=CARTESIAN_POINT('Ctrl Pts',(3.62130879372,-0.2341795348991,-6.229087986272));
#51142=CARTESIAN_POINT('Ctrl Pts',(3.26714225565,-1.579398276366,-6.275129652939));
#51143=CARTESIAN_POINT('Ctrl Pts',(2.432892888262,-2.692535910306,-6.321171319606));
#51144=CARTESIAN_POINT('Ctrl Pts',(1.241147577988,-3.410024944732,-6.367212986272));
#51145=CARTESIAN_POINT('Ctrl Pts',(-0.1329753559758,-3.626435576257,-6.413254652939));
#51146=CARTESIAN_POINT('Ctrl Pts',(-1.487558527012,-3.309967834097,-6.459296319606));
#51147=CARTESIAN_POINT('Ctrl Pts',(-2.623555774772,-2.507124354854,-6.505337986272));
#51148=CARTESIAN_POINT('Ctrl Pts',(-3.374040553019,-1.33587715776,-6.551379652939));
#51149=CARTESIAN_POINT('Ctrl Pts',(-3.628734573418,0.03166748686998,-6.597421319606));
#51150=CARTESIAN_POINT('Ctrl Pts',(-3.350212399193,1.394558824265,-6.643462986272));
#51151=CARTESIAN_POINT('Ctrl Pts',(-2.57940084129,2.552529869363,-6.689504652939));
#51152=CARTESIAN_POINT('Ctrl Pts',(-1.429565060708,3.335425185976,-6.735546319606));
#51153=CARTESIAN_POINT('Ctrl Pts',(-0.06966507558957,3.628203992513,-6.781587986272));
#51154=CARTESIAN_POINT('Ctrl Pts',(1.300471686497,3.387844569437,-6.827629652939));
#51155=CARTESIAN_POINT('Ctrl Pts',(2.479513577945,2.649665988541,-6.873671319606));
#51156=CARTESIAN_POINT('Ctrl Pts',(3.294208954705,1.522138231824,-6.919712986272));
#51157=CARTESIAN_POINT('Ctrl Pts',(3.624844247273,0.1709433153187,-6.965754652939));
#51158=CARTESIAN_POINT('Ctrl Pts',(3.422835000394,-1.205370480026,-7.011796319606));
#51159=CARTESIAN_POINT('Ctrl Pts',(2.717865005957,-2.404563836423,-7.057837986272));
#51160=CARTESIAN_POINT('Ctrl Pts',(1.613524485334,-3.250423998384,-7.103879652939));
#51161=CARTESIAN_POINT('Ctrl Pts',(0.2720882585925,-3.618657957528,-7.149921319606));
#51162=CARTESIAN_POINT('Ctrl Pts',(-1.109329361913,-3.455156407579,-7.195962986272));
#51163=CARTESIAN_POINT('Ctrl Pts',(-2.327739088356,-2.783944714,-7.242004652939));
#51164=CARTESIAN_POINT('Ctrl Pts',(-3.204104459192,-1.70365256098,-7.288046319606));
#51165=CARTESIAN_POINT('Ctrl Pts',(-3.609649947201,-0.3730210356546,-7.334087986272));
#51166=CARTESIAN_POINT('Ctrl Pts',(-3.484783587573,1.012423222237,-7.380129652939));
#51167=CARTESIAN_POINT('Ctrl Pts',(-2.847853586283,2.249099238981,-7.426171319606));
#51168=CARTESIAN_POINT('Ctrl Pts',(-1.792452177415,3.155286457167,-7.472212986272));
#51169=CARTESIAN_POINT('Ctrl Pts',(-0.4736629503042,3.597827235041,-7.518254652939));
#51170=CARTESIAN_POINT('Ctrl Pts',(0.9147276558781,3.51169345825,-7.564296319606));
#51171=CARTESIAN_POINT('Ctrl Pts',(2.168705495876,2.909541712997,-7.610337986272));
#51172=CARTESIAN_POINT('Ctrl Pts',(3.104008482379,1.8798543735,-7.656379652939));
#51173=CARTESIAN_POINT('Ctrl Pts',(3.583197460416,0.5739344720891,-7.702421319606));
#51174=CARTESIAN_POINT('Ctrl Pts',(3.535870931347,-0.8163149133711,-7.748462986272));
#51175=CARTESIAN_POINT('Ctrl Pts',(2.968938990236,-2.086635212868,-7.794504652939));
#51176=CARTESIAN_POINT('Ctrl Pts',(2.300228400622,-2.729048929993,-7.825199097383));
#51177=CARTESIAN_POINT('Ctrl Pts',(1.917647064401,-2.975605776375,-7.840546319606));
#51178=CARTESIAN_POINT('Ctrl Pts',(-1.2107138361353,-3.32640900638413,-4.92608554369097));
#51179=CARTESIAN_POINT('Ctrl Pts',(-1.39219287791354,-3.26025710999361,
-4.93259895336898));
#51180=CARTESIAN_POINT('Ctrl Pts',(-1.56825188018812,-3.17927104787258,
-4.93911236304649));
#51181=CARTESIAN_POINT('Ctrl Pts',(-1.73659924449935,-3.08457088033829,
-4.94562577272425));
#51182=CARTESIAN_POINT('Ctrl Pts',(-1.87338108397249,-3.00762721586959,
-4.9509179028423));
#51183=CARTESIAN_POINT('Ctrl Pts',(-2.00508361696359,-2.92162011815734,
-4.95621003296051));
#51184=CARTESIAN_POINT('Ctrl Pts',(-2.13042518195858,-2.827169705567,-4.96150216307867));
#51185=CARTESIAN_POINT('Ctrl Pts',(-2.15935060962041,-2.80537311656542,
-4.9627234429224));
#51186=CARTESIAN_POINT('Ctrl Pts',(-2.18793730334398,-2.78312691895196,
-4.96394472276613));
#51187=CARTESIAN_POINT('Ctrl Pts',(-2.21617354772985,-2.76044407979828,
-4.96516600260984));
#51188=CARTESIAN_POINT('Ctrl Pts',(-2.36676494282521,-2.63947047062431,
-4.97167941257167));
#51189=CARTESIAN_POINT('Ctrl Pts',(-2.50737055352154,-2.50609287961651,
-4.97819282253333));
#51190=CARTESIAN_POINT('Ctrl Pts',(-2.63627091172052,-2.36224216903429,
-4.98470623249499));
#51191=CARTESIAN_POINT('Ctrl Pts',(-2.76517126991969,-2.21839145845186,
-4.99121964245666));
#51192=CARTESIAN_POINT('Ctrl Pts',(-2.88238227181575,-2.06404968982843,
-4.99773305241833));
#51193=CARTESIAN_POINT('Ctrl Pts',(-2.98616562034842,-1.90113425254753,
-5.00424646238));
#51194=CARTESIAN_POINT('Ctrl Pts',(-3.0036792827206,-1.87364192353623,-5.00534561426297));
#51195=CARTESIAN_POINT('Ctrl Pts',(-3.02081015796238,-1.84590601958711,
-5.00644476614593));
#51196=CARTESIAN_POINT('Ctrl Pts',(-3.03754976626217,-1.81793603228567,
-5.0075439180289));
#51197=CARTESIAN_POINT('Ctrl Pts',(-3.12000657762367,-1.6801600505903,-5.0129581761076));
#51198=CARTESIAN_POINT('Ctrl Pts',(-3.1929686605663,-1.53670385765163,-5.0183724341863));
#51199=CARTESIAN_POINT('Ctrl Pts',(-3.25592170098541,-1.38899996899466,
-5.023786692265));
#51200=CARTESIAN_POINT('Ctrl Pts',(-3.3316548770961,-1.21131062250045,-5.03030010222667));
#51201=CARTESIAN_POINT('Ctrl Pts',(-3.39291563048331,-1.0274545075206,-5.03681351218833));
#51202=CARTESIAN_POINT('Ctrl Pts',(-3.4388318118105,-0.839831766260492,
-5.04332692215));
#51203=CARTESIAN_POINT('Ctrl Pts',(-3.46293778073547,-0.741329934450789,
-5.04674645865311));
#51204=CARTESIAN_POINT('Ctrl Pts',(-3.48281390249413,-0.641787444045981,
-5.05016599515622));
#51205=CARTESIAN_POINT('Ctrl Pts',(-3.49832847032117,-0.541569860445466,
-5.05358553165932));
#51206=CARTESIAN_POINT('Ctrl Pts',(-3.51236549246657,-0.450896600574981,
-5.05667940511788));
#51207=CARTESIAN_POINT('Ctrl Pts',(-3.52283219794054,-0.359670757793759,
-5.05977327857645));
#51208=CARTESIAN_POINT('Ctrl Pts',(-3.52973959895587,-0.268179901742102,
-5.06286715203501));
#51209=CARTESIAN_POINT('Ctrl Pts',(-3.54428147831359,-0.0755678052264873,
-5.06938056199667));
#51210=CARTESIAN_POINT('Ctrl Pts',(-3.54305196908429,0.118222685023444,
-5.07589397195833));
#51211=CARTESIAN_POINT('Ctrl Pts',(-3.52615816121155,0.3106374510054,-5.08240738191999));
#51212=CARTESIAN_POINT('Ctrl Pts',(-3.51127051610728,0.480202700612879,
-5.08814731554883));
#51213=CARTESIAN_POINT('Ctrl Pts',(-3.48421326830643,0.648717483567016,
-5.09388724917767));
#51214=CARTESIAN_POINT('Ctrl Pts',(-3.44505320963117,0.814376069645967,
-5.0996271828065));
#51215=CARTESIAN_POINT('Ctrl Pts',(-3.43977625339156,0.836699149309945,
-5.10040065913933));
#51216=CARTESIAN_POINT('Ctrl Pts',(-3.4342795483969,0.85897036558526,-5.10117413547217));
#51217=CARTESIAN_POINT('Ctrl Pts',(-3.42856490437154,0.881185686590716,
-5.101947611805));
#51218=CARTESIAN_POINT('Ctrl Pts',(-3.38044213998663,1.06825992144005,-5.10846102176667));
#51219=CARTESIAN_POINT('Ctrl Pts',(-3.31687241555554,1.25134319073251,-5.11497443172833));
#51220=CARTESIAN_POINT('Ctrl Pts',(-3.23893637138191,1.42807546042492,-5.12148784169));
#51221=CARTESIAN_POINT('Ctrl Pts',(-3.16100032720827,1.60480773011733,-5.12800125165167));
#51222=CARTESIAN_POINT('Ctrl Pts',(-3.06868910928958,1.77521130597631,-5.13451466161333));
#51223=CARTESIAN_POINT('Ctrl Pts',(-2.96305546573071,1.93693229393157,-5.141028071575));
#51224=CARTESIAN_POINT('Ctrl Pts',(-2.93796716681119,1.97534150098615,-5.1425750254677));
#51225=CARTESIAN_POINT('Ctrl Pts',(-2.91212788447957,2.01326000353812,-5.14412197936041));
#51226=CARTESIAN_POINT('Ctrl Pts',(-2.88555239687917,2.05065535009337,-5.14566893325311));
#51227=CARTESIAN_POINT('Ctrl Pts',(-2.80023247086108,2.1707121576857,-5.15063538932208));
#51228=CARTESIAN_POINT('Ctrl Pts',(-2.70732368293247,2.28537607124037,-5.15560184539104));
#51229=CARTESIAN_POINT('Ctrl Pts',(-2.60768233598873,2.39383487273625,-5.16056830146001));
#51230=CARTESIAN_POINT('Ctrl Pts',(-2.47700465903675,2.53607646881263,-5.16708171142167));
#51231=CARTESIAN_POINT('Ctrl Pts',(-2.3347360735518,2.66766424466987,-5.17359512138333));
#51232=CARTESIAN_POINT('Ctrl Pts',(-2.18272371894347,2.78683825766546,-5.18010853134499));
#51233=CARTESIAN_POINT('Ctrl Pts',(-2.09246668450921,2.85759759181515,-5.1839758556076));
#51234=CARTESIAN_POINT('Ctrl Pts',(-1.99876997137404,2.92398232168098,-5.18784317987021));
#51235=CARTESIAN_POINT('Ctrl Pts',(-1.90204061354772,2.98560571817767,-5.19171050413282));
#51236=CARTESIAN_POINT('Ctrl Pts',(-1.83585682521188,3.02776944098037,-5.19435658983187));
#51237=CARTESIAN_POINT('Ctrl Pts',(-1.7682533936754,3.06770422962763,-5.19700267553092));
#51238=CARTESIAN_POINT('Ctrl Pts',(-1.69939760621079,3.10534408721984,-5.19964876122998));
#51239=CARTESIAN_POINT('Ctrl Pts',(-1.52990726349332,3.19799559260592,-5.20616217119167));
#51240=CARTESIAN_POINT('Ctrl Pts',(-1.35283221159455,3.27674344861159,-5.21267558115337));
#51241=CARTESIAN_POINT('Ctrl Pts',(-1.1705592811959,3.34065903690989,-5.21918899111507));
#51242=CARTESIAN_POINT('Ctrl Pts',(-0.997400068785245,3.40137882073238,
-5.22537672802482));
#51243=CARTESIAN_POINT('Ctrl Pts',(-0.819528440494076,3.44871677050005,
-5.23156446493458));
#51244=CARTESIAN_POINT('Ctrl Pts',(-0.639037774186981,3.4818430066795,-5.23775220184434));
#51245=CARTESIAN_POINT('Ctrl Pts',(-0.629538187021195,3.48358650718565,
-5.23807787489622));
#51246=CARTESIAN_POINT('Ctrl Pts',(-0.62003134595265,3.48529064171064,-5.23840354794811));
#51247=CARTESIAN_POINT('Ctrl Pts',(-0.61051757907874,3.48695541282214,-5.238729221));
#51248=CARTESIAN_POINT('Ctrl Pts',(-0.420243733667227,3.52025057396201,
-5.24524263096164));
#51249=CARTESIAN_POINT('Ctrl Pts',(-0.227230723008247,3.53779512210829,
-5.25175604092327));
#51250=CARTESIAN_POINT('Ctrl Pts',(-0.0340855960367684,3.53962915369353,
-5.2582694508849));
#51251=CARTESIAN_POINT('Ctrl Pts',(0.159059530937512,3.54146318527879,-5.26478286084663));
#51252=CARTESIAN_POINT('Ctrl Pts',(0.352360719567761,3.52758887010852,-5.27129627080837));
#51253=CARTESIAN_POINT('Ctrl Pts',(0.543247550769443,3.4980247813142,-5.27780968077025));
#51254=CARTESIAN_POINT('Ctrl Pts',(0.601707228720348,3.48897068837889,-5.2798044325629));
#51255=CARTESIAN_POINT('Ctrl Pts',(0.659939301890289,3.47844500445235,-5.28179918435557));
#51256=CARTESIAN_POINT('Ctrl Pts',(0.717867025561981,3.466448749601,-5.28379393614825));
#51257=CARTESIAN_POINT('Ctrl Pts',(0.849089156932971,3.43927395262494,-5.28831259431742));
#51258=CARTESIAN_POINT('Ctrl Pts',(0.978749296819402,3.40455233357054,-5.29283125248663));
#51259=CARTESIAN_POINT('Ctrl Pts',(1.10602473720318,3.36262936004284,-5.29734991065576));
#51260=CARTESIAN_POINT('Ctrl Pts',(1.28948564313355,3.30219958129296,-5.30386332061764));
#51261=CARTESIAN_POINT('Ctrl Pts',(1.46801104029239,3.22680554536042,-5.31037673057937));
#51262=CARTESIAN_POINT('Ctrl Pts',(1.63924880370262,3.13743299108219,-5.3168901405411));
#51263=CARTESIAN_POINT('Ctrl Pts',(1.75269332737295,3.07822393200914,-5.32120525582795));
#51264=CARTESIAN_POINT('Ctrl Pts',(1.86294511722153,3.01287435802278,-5.3255203711148));
#51265=CARTESIAN_POINT('Ctrl Pts',(1.96928647887088,2.941685021231,-5.32983548640166));
#51266=CARTESIAN_POINT('Ctrl Pts',(2.02346107989141,2.90541828684098,-5.33203378107644));
#51267=CARTESIAN_POINT('Ctrl Pts',(2.07662086897177,2.86763609085749,-5.33423207575122));
#51268=CARTESIAN_POINT('Ctrl Pts',(2.12869278492199,2.82841085585619,-5.336430370426));
#51269=CARTESIAN_POINT('Ctrl Pts',(2.28297862292286,2.71218893195501,-5.34294378038764));
#51270=CARTESIAN_POINT('Ctrl Pts',(2.42770829556085,2.58330600898348,-5.34945719034927));
#51271=CARTESIAN_POINT('Ctrl Pts',(2.56106883516398,2.44357975449348,-5.35597060031091));
#51272=CARTESIAN_POINT('Ctrl Pts',(2.69442937476905,2.30385350000145,-5.36248401027264));
#51273=CARTESIAN_POINT('Ctrl Pts',(2.81643557043219,2.1532649176556,-5.36899742023437));
#51274=CARTESIAN_POINT('Ctrl Pts',(2.92522794721502,1.99364991391056,-5.3755108301961));
#51275=CARTESIAN_POINT('Ctrl Pts',(2.92726781554804,1.99065711605796,-5.37563295730751));
#51276=CARTESIAN_POINT('Ctrl Pts',(2.92930303206135,1.98766115426643,-5.37575508441893));
#51277=CARTESIAN_POINT('Ctrl Pts',(2.9313335845635,1.984662040754,-5.37587721153035));
#51278=CARTESIAN_POINT('Ctrl Pts',(3.03759856727369,1.82770931719371,-5.38226849438057));
#51279=CARTESIAN_POINT('Ctrl Pts',(3.13108925869377,1.66212467796123,-5.38865977723078));
#51280=CARTESIAN_POINT('Ctrl Pts',(3.21084406279643,1.49018936490803,-5.395051060081));
#51281=CARTESIAN_POINT('Ctrl Pts',(3.29212285262701,1.31496864521171,-5.40156447004263));
#51282=CARTESIAN_POINT('Ctrl Pts',(3.35914855060852,1.13313177099434,-5.40807788000427));
#51283=CARTESIAN_POINT('Ctrl Pts',(3.41090884185987,0.947034149938319,-5.41459128996591));
#51284=CARTESIAN_POINT('Ctrl Pts',(3.43031907907144,0.877247081862021,-5.41703383480781));
#51285=CARTESIAN_POINT('Ctrl Pts',(3.4475820095095,0.806861453565564,-5.41947637964972));
#51286=CARTESIAN_POINT('Ctrl Pts',(3.46264250659767,0.736007385494901,-5.42191892449163));
#51287=CARTESIAN_POINT('Ctrl Pts',(3.48774307025223,0.617918517950802,-5.42598978961145));
#51288=CARTESIAN_POINT('Ctrl Pts',(3.50672549247776,0.498528446452136,-5.43006065473127));
#51289=CARTESIAN_POINT('Ctrl Pts',(3.51957889593106,0.378491351196591,-5.43413151985108));
#51290=CARTESIAN_POINT('Ctrl Pts',(3.54014442282263,0.186431238913331,-5.4406449298127));
#51291=CARTESIAN_POINT('Ctrl Pts',(3.54502560134987,-0.00730000610566984,
-5.4471583397743));
#51292=CARTESIAN_POINT('Ctrl Pts',(3.53418198158554,-0.200151998238902,
-5.45367174973592));
#51293=CARTESIAN_POINT('Ctrl Pts',(3.52625261802275,-0.341174423652751,
-5.45843466071414));
#51294=CARTESIAN_POINT('Ctrl Pts',(3.50991175822703,-0.481737410954006,
-5.46319757169237));
#51295=CARTESIAN_POINT('Ctrl Pts',(3.48514125710933,-0.620798210365567,
-5.46796048267059));
#51296=CARTESIAN_POINT('Ctrl Pts',(3.47603742602251,-0.671906826320724,
-5.46971098165409));
#51297=CARTESIAN_POINT('Ctrl Pts',(3.46579506342518,-0.722812536677146,
-5.4714614806376));
#51298=CARTESIAN_POINT('Ctrl Pts',(3.45443274215295,-0.7734670235766,-5.4732119796211));
#51299=CARTESIAN_POINT('Ctrl Pts',(3.41215482182319,-0.961946675768368,
-5.47972538958273));
#51300=CARTESIAN_POINT('Ctrl Pts',(3.35437640811406,-1.1469330851341,-5.48623879954437));
#51301=CARTESIAN_POINT('Ctrl Pts',(3.28203684521707,-1.32602898115537,-5.492752209506));
#51302=CARTESIAN_POINT('Ctrl Pts',(3.20969728232009,-1.50512487717664,-5.49926561946764));
#51303=CARTESIAN_POINT('Ctrl Pts',(3.12278631763227,-1.67835197646303,-5.50577902942927));
#51304=CARTESIAN_POINT('Ctrl Pts',(3.02223197295951,-1.8432806479056,-5.51229243939091));
#51305=CARTESIAN_POINT('Ctrl Pts',(3.01343337877785,-1.85771205267151,-5.512862368529));
#51306=CARTESIAN_POINT('Ctrl Pts',(3.00453044323614,-1.8720797233967,-5.5134322976671));
#51307=CARTESIAN_POINT('Ctrl Pts',(2.9955238080915,-1.8863820172901,-5.5140022268052));
#51308=CARTESIAN_POINT('Ctrl Pts',(2.90159851161271,-2.03553285694236,-5.51994570762883));
#51309=CARTESIAN_POINT('Ctrl Pts',(2.79639484911094,-2.17757303830368,-5.52588918845246));
#51310=CARTESIAN_POINT('Ctrl Pts',(2.68128796199762,-2.31104848987915,-5.53183266927608));
#51311=CARTESIAN_POINT('Ctrl Pts',(2.55514330578951,-2.45732309927445,-5.5383460792377));
#51312=CARTESIAN_POINT('Ctrl Pts',(2.41709243724114,-2.5933320851481,-5.5448594891993));
#51313=CARTESIAN_POINT('Ctrl Pts',(2.26888276917332,-2.71720685314313,-5.55137289916092));
#51314=CARTESIAN_POINT('Ctrl Pts',(2.20311454325284,-2.77217643666326,-5.55426323299307));
#51315=CARTESIAN_POINT('Ctrl Pts',(2.13534527838208,-2.82475626413618,-5.55715356682523));
#51316=CARTESIAN_POINT('Ctrl Pts',(2.06573588820082,-2.874775685197,-5.56004390065739));
#51317=CARTESIAN_POINT('Ctrl Pts',(1.97847948994207,-2.93747576795006,-5.56366697678695));
#51318=CARTESIAN_POINT('Ctrl Pts',(1.8883316623885,-2.99615253300867,-5.56729005291652));
#51319=CARTESIAN_POINT('Ctrl Pts',(1.79571220403399,-3.05061307565962,-5.57091312904609));
#51320=CARTESIAN_POINT('Ctrl Pts',(1.62920493752531,-3.14851988974053,-5.57742653900773));
#51321=CARTESIAN_POINT('Ctrl Pts',(1.45470238311938,-3.23280915686397,-5.58393994896937));
#51322=CARTESIAN_POINT('Ctrl Pts',(1.27452614193469,-3.30242008610374,-5.590453358931));
#51323=CARTESIAN_POINT('Ctrl Pts',(1.13038560964147,-3.3581086515221,-5.59566407024755));
#51324=CARTESIAN_POINT('Ctrl Pts',(0.982599582851888,-3.40440558395331,
-5.60087478156409));
#51325=CARTESIAN_POINT('Ctrl Pts',(0.832403080383234,-3.440741942048,-5.60608549288073));
#51326=CARTESIAN_POINT('Ctrl Pts',(0.794853354755285,-3.44982617672956,
-5.60738819152584));
#51327=CARTESIAN_POINT('Ctrl Pts',(0.757152994147706,-3.45828791657968,
-5.60869089017095));
#51328=CARTESIAN_POINT('Ctrl Pts',(0.719323216056949,-3.46612616198879,
-5.60999358881607));
#51329=CARTESIAN_POINT('Ctrl Pts',(0.53017674354351,-3.50531688804249,-5.61650699877797));
#51330=CARTESIAN_POINT('Ctrl Pts',(0.337816928320247,-3.52891744226118,
-5.62302040874003));
#51331=CARTESIAN_POINT('Ctrl Pts',(0.14482526557731,-3.53682450849307,-5.62953381870193));
#51332=CARTESIAN_POINT('Ctrl Pts',(-0.0481663971628286,-3.54473157472486,
-5.63604722866373));
#51333=CARTESIAN_POINT('Ctrl Pts',(-0.241813887038626,-3.53694580387158,
-5.64256063862537));
#51334=CARTESIAN_POINT('Ctrl Pts',(-0.43353044931056,-3.51334032191244,
-5.649074048587));
#51335=CARTESIAN_POINT('Ctrl Pts',(-0.463486537026694,-3.50965191920081,
-5.6500917816291));
#51336=CARTESIAN_POINT('Ctrl Pts',(-0.493394854987646,-3.50557733750051,
-5.6511095146712));
#51337=CARTESIAN_POINT('Ctrl Pts',(-0.523245315398818,-3.50111615630133,
-5.6521272477133));
#51338=CARTESIAN_POINT('Ctrl Pts',(-0.684435410967259,-3.4770261351111,
-5.65762292463283));
#51339=CARTESIAN_POINT('Ctrl Pts',(-0.843938087347245,-3.44166213854163,
-5.66311860155237));
#51340=CARTESIAN_POINT('Ctrl Pts',(-1.00025566879186,-3.3955592316282,-5.6686142784719));
#51341=CARTESIAN_POINT('Ctrl Pts',(-1.1855213798375,-3.34091862273666,-5.67512768843364));
#51342=CARTESIAN_POINT('Ctrl Pts',(-1.36633644531484,-3.27119098514052,
-5.68164109839537));
#51343=CARTESIAN_POINT('Ctrl Pts',(-1.54029195487117,-3.18722583254679,
-5.68815450835708));
#51344=CARTESIAN_POINT('Ctrl Pts',(-1.62944410370729,-3.14419371588561,
-5.69149262909737));
#51345=CARTESIAN_POINT('Ctrl Pts',(-1.71679583817648,-3.09742028661071,
-5.69483074983765));
#51346=CARTESIAN_POINT('Ctrl Pts',(-1.80200661175621,-3.04702677559416,
-5.69816887057794));
#51347=CARTESIAN_POINT('Ctrl Pts',(-1.88306085512837,-2.99909142968991,
-5.70134415979926));
#51348=CARTESIAN_POINT('Ctrl Pts',(-1.96217788986923,-2.94788060262952,
-5.70451944902059));
#51349=CARTESIAN_POINT('Ctrl Pts',(-2.03912504838554,-2.89360083987272,
-5.70769473824192));
#51350=CARTESIAN_POINT('Ctrl Pts',(-2.19696528084022,-2.78225780217885,
-5.71420814820364));
#51351=CARTESIAN_POINT('Ctrl Pts',(-2.34568157844476,-2.65800144637074,
-5.72072155816537));
#51352=CARTESIAN_POINT('Ctrl Pts',(-2.48336853770674,-2.52253489439242,
-5.7272349681271));
#51353=CARTESIAN_POINT('Ctrl Pts',(-2.60298386808918,-2.4048485393628,-5.73289348283804));
#51354=CARTESIAN_POINT('Ctrl Pts',(-2.71428549057575,-2.27868697184984,
-5.73855199754897));
#51355=CARTESIAN_POINT('Ctrl Pts',(-2.81597612222633,-2.14519893694035,
-5.74421051225991));
#51356=CARTESIAN_POINT('Ctrl Pts',(-2.83133966592628,-2.12503140307353,
-5.74506540751061));
#51357=CARTESIAN_POINT('Ctrl Pts',(-2.84648385104755,-2.10469665766999,
-5.7459203027613));
#51358=CARTESIAN_POINT('Ctrl Pts',(-2.86140601976011,-2.08420004970933,
-5.746775198012));
#51359=CARTESIAN_POINT('Ctrl Pts',(-2.97509737816046,-1.92803727963656,
-5.75328860797363));
#51360=CARTESIAN_POINT('Ctrl Pts',(-3.07588539103572,-1.76250130618686,
-5.75980201793527));
#51361=CARTESIAN_POINT('Ctrl Pts',(-3.16263326328894,-1.58992343651983,
-5.76631542789691));
#51362=CARTESIAN_POINT('Ctrl Pts',(-3.24938113554341,-1.4173455668503,-5.77282883785864));
#51363=CARTESIAN_POINT('Ctrl Pts',(-3.32210027300758,-1.23770469083994,
-5.77934224782037));
#51364=CARTESIAN_POINT('Ctrl Pts',(-3.37963916765126,-1.05330980373386,
-5.7858556577821));
#51365=CARTESIAN_POINT('Ctrl Pts',(-3.39258558113939,-1.01182043435414,
-5.78732119338379));
#51366=CARTESIAN_POINT('Ctrl Pts',(-3.40476309979245,-0.970091329658437,
-5.78878672898548));
#51367=CARTESIAN_POINT('Ctrl Pts',(-3.41615839043217,-0.928149692388579,
-5.79025226458717));
#51368=CARTESIAN_POINT('Ctrl Pts',(-3.45540820147598,-0.783686388225696,
-5.79530013894711));
#51369=CARTESIAN_POINT('Ctrl Pts',(-3.48537682874472,-0.636701514870851,
-5.80034801330706));
#51370=CARTESIAN_POINT('Ctrl Pts',(-3.50597617628425,-0.488430196162447,
-5.805395887667));
#51371=CARTESIAN_POINT('Ctrl Pts',(-3.53255607623814,-0.297111669702389,
-5.81190929762864));
#51372=CARTESIAN_POINT('Ctrl Pts',(-3.54354418974018,-0.103630424635091,
-5.81842270759027));
#51373=CARTESIAN_POINT('Ctrl Pts',(-3.53875253925765,0.089468803271073,
-5.82493611755191));
#51374=CARTESIAN_POINT('Ctrl Pts',(-3.53596740081211,0.201707391082333,
-5.82872202567726));
#51375=CARTESIAN_POINT('Ctrl Pts',(-3.52784953284791,0.313821101074286,
-5.83250793380262));
#51376=CARTESIAN_POINT('Ctrl Pts',(-3.51436099043,0.425284409474744,-5.83629384192797));
#51377=CARTESIAN_POINT('Ctrl Pts',(-3.50464336839674,0.505586510921572,
-5.83902134376434));
#51378=CARTESIAN_POINT('Ctrl Pts',(-3.49213834393737,0.585551019147991,
-5.84174884560071));
#51379=CARTESIAN_POINT('Ctrl Pts',(-3.47690638446997,0.66499043379555,-5.84447634743708));
#51380=CARTESIAN_POINT('Ctrl Pts',(-3.44053170812434,0.854695704681691,
-5.8509897573987));
#51381=CARTESIAN_POINT('Ctrl Pts',(-3.38860921956519,1.04140602837934,-5.8575031673603));
#51382=CARTESIAN_POINT('Ctrl Pts',(-3.32193574191479,1.22268842298407,-5.86401657732192));
#51383=CARTESIAN_POINT('Ctrl Pts',(-3.25942939273935,1.3926405697123,-5.87012289563216));
#51384=CARTESIAN_POINT('Ctrl Pts',(-3.18394820657006,1.55784068731747,-5.87622921394241));
#51385=CARTESIAN_POINT('Ctrl Pts',(-3.09615376327333,1.71622605567233,-5.88233553225266));
#51386=CARTESIAN_POINT('Ctrl Pts',(-3.09030074626759,1.7267851778631,-5.88274262390414));
#51387=CARTESIAN_POINT('Ctrl Pts',(-3.08439300690686,1.73731401277661,-5.88314971555562));
#51388=CARTESIAN_POINT('Ctrl Pts',(-3.0784309562568,1.74781206796055,-5.8835568072071));
#51389=CARTESIAN_POINT('Ctrl Pts',(-2.98303897276905,1.91577949486414,-5.89007021716873));
#51390=CARTESIAN_POINT('Ctrl Pts',(-2.87375899624301,2.0758403789111,-5.89658362713037));
#51391=CARTESIAN_POINT('Ctrl Pts',(-2.75227553257105,2.22600746165049,-5.903097037092));
#51392=CARTESIAN_POINT('Ctrl Pts',(-2.63079206889909,2.37617454438987,-5.90961044705364));
#51393=CARTESIAN_POINT('Ctrl Pts',(-2.49709140537515,2.51646756267748,-5.91612385701527));
#51394=CARTESIAN_POINT('Ctrl Pts',(-2.35282015491859,2.64491088381421,-5.92263726697691));
#51395=CARTESIAN_POINT('Ctrl Pts',(-2.31044002818164,2.6826415072826,-5.92455060133001));
#51396=CARTESIAN_POINT('Ctrl Pts',(-2.26714849820321,2.71934870346318,-5.92646393568311));
#51397=CARTESIAN_POINT('Ctrl Pts',(-2.222989224079,2.754980745782,-5.92837727003622));
#51398=CARTESIAN_POINT('Ctrl Pts',(-2.11682063965784,2.84064799389807,-5.93297734564484));
#51399=CARTESIAN_POINT('Ctrl Pts',(-2.00563588372431,2.92009993133965,-5.93757742125347));
#51400=CARTESIAN_POINT('Ctrl Pts',(-1.89026706688281,2.99289754536391,-5.94217749686209));
#51401=CARTESIAN_POINT('Ctrl Pts',(-1.72691227343801,3.09597426512039,-5.94869090682373));
#51402=CARTESIAN_POINT('Ctrl Pts',(-1.55515506607057,3.18572418961666,-5.95520431678537));
#51403=CARTESIAN_POINT('Ctrl Pts',(-1.37724999191978,3.26095501036923,-5.96171772674717));
#51404=CARTESIAN_POINT('Ctrl Pts',(-1.26161218703417,3.30985483525111,-5.96595142516132));
#51405=CARTESIAN_POINT('Ctrl Pts',(-1.14336967917687,3.3526213717884,-5.97018512357555));
#51406=CARTESIAN_POINT('Ctrl Pts',(-1.02317256118378,3.3889110212635,-5.97441882198976));
#51407=CARTESIAN_POINT('Ctrl Pts',(-0.958450247245205,3.40845183992259,
-5.97669853353743));
#51408=CARTESIAN_POINT('Ctrl Pts',(-0.893161262302633,3.42611482909649,
-5.9789782450851));
#51409=CARTESIAN_POINT('Ctrl Pts',(-0.827419800164966,3.44188829366148,
-5.98125795663274));
#51410=CARTESIAN_POINT('Ctrl Pts',(-0.639588539302325,3.48695497823278,
-5.98777136659464));
#51411=CARTESIAN_POINT('Ctrl Pts',(-0.448071840368233,3.51659792381026,
-5.99428477655636));
#51412=CARTESIAN_POINT('Ctrl Pts',(-0.255423787888959,3.53056979807232,
-6.00079818651808));
#51413=CARTESIAN_POINT('Ctrl Pts',(-0.0627757354124814,3.54454167233417,
-6.0073115964797));
#51414=CARTESIAN_POINT('Ctrl Pts',(0.131027743644201,3.54284160663297,-6.0138250064413));
#51415=CARTESIAN_POINT('Ctrl Pts',(0.323385332326878,3.52519811655209,-6.02033841640292));
#51416=CARTESIAN_POINT('Ctrl Pts',(0.515742921012345,3.50755462647095,-6.02685182636464));
#51417=CARTESIAN_POINT('Ctrl Pts',(0.706621482692652,3.47396442994213,-6.03336523632637));
#51418=CARTESIAN_POINT('Ctrl Pts',(0.893511611909647,3.42517311385951,-6.03987864628809));
#51419=CARTESIAN_POINT('Ctrl Pts',(1.08040174112393,3.3763817977776,-6.04639205624973));
#51420=CARTESIAN_POINT('Ctrl Pts',(1.26332731289825,3.31238606054051,-6.05290546621136));
#51421=CARTESIAN_POINT('Ctrl Pts',(1.43982452056484,3.23389875855054,-6.059418876173));
#51422=CARTESIAN_POINT('Ctrl Pts',(1.50380522324394,3.20544690484081,-6.06178000444065));
#51423=CARTESIAN_POINT('Ctrl Pts',(1.56694025449916,3.17509076695823,-6.0641411327083));
#51424=CARTESIAN_POINT('Ctrl Pts',(1.62910723813456,3.14286646338266,-6.06650226097594));
#51425=CARTESIAN_POINT('Ctrl Pts',(1.73843413564225,3.08619678233581,-6.07065454266993));
#51426=CARTESIAN_POINT('Ctrl Pts',(1.84476690245898,3.02374911182526,-6.07480682436392));
#51427=CARTESIAN_POINT('Ctrl Pts',(1.94756203567169,2.95595504167199,-6.07895910605791));
#51428=CARTESIAN_POINT('Ctrl Pts',(2.10880996970625,2.84961096281966,-6.08547251601964));
#51429=CARTESIAN_POINT('Ctrl Pts',(2.26136901605629,2.73010640649609,-6.09198592598137));
#51430=CARTESIAN_POINT('Ctrl Pts',(2.40324259782627,2.59902847899996,-6.09849933594308));
#51431=CARTESIAN_POINT('Ctrl Pts',(2.50521379478413,2.50481662507491,-6.10318082915547));
#51432=CARTESIAN_POINT('Ctrl Pts',(2.60167081814559,2.40461726441304,-6.10786232236785));
#51433=CARTESIAN_POINT('Ctrl Pts',(2.69183711822383,2.2990460910885,-6.11254381558023));
#51434=CARTESIAN_POINT('Ctrl Pts',(2.72712012469975,2.25773499826505,-6.11437573232946));
#51435=CARTESIAN_POINT('Ctrl Pts',(2.76143995124405,2.2156014429839,-6.11620764907869));
#51436=CARTESIAN_POINT('Ctrl Pts',(2.79476729971627,2.17269706292566,-6.11803956582792));
#51437=CARTESIAN_POINT('Ctrl Pts',(2.91326323225658,2.02014983795509,-6.12455297578964));
#51438=CARTESIAN_POINT('Ctrl Pts',(3.01920517514468,1.85787088053258,-6.13106638575137));
#51439=CARTESIAN_POINT('Ctrl Pts',(3.11133748932251,1.68810632525813,-6.1375797957131));
#51440=CARTESIAN_POINT('Ctrl Pts',(3.203469803499,1.51834176998613,-6.14409320567473));
#51441=CARTESIAN_POINT('Ctrl Pts',(3.28180255010409,1.34106980168587,-6.15060661563637));
#51442=CARTESIAN_POINT('Ctrl Pts',(3.34504642056238,1.15855163970423,-6.157120025598));
#51443=CARTESIAN_POINT('Ctrl Pts',(3.34978975557038,1.14486264848577,-6.15760853595116));
#51444=CARTESIAN_POINT('Ctrl Pts',(3.35444815655005,1.1311443095087,-6.15809704630431));
#51445=CARTESIAN_POINT('Ctrl Pts',(3.35902108122167,1.11739759079248,-6.15858555665747));
#51446=CARTESIAN_POINT('Ctrl Pts',(3.41541991061322,0.94785645481421,-6.16461045626595));
#51447=CARTESIAN_POINT('Ctrl Pts',(3.45881608303693,0.773998449359656,-6.17063535587443));
#51448=CARTESIAN_POINT('Ctrl Pts',(3.48894891305953,0.597889911087293,-6.17666025548291));
#51449=CARTESIAN_POINT('Ctrl Pts',(3.52152497042123,0.407502156590185,-6.18317366544464));
#51450=CARTESIAN_POINT('Ctrl Pts',(3.53860724556339,0.214461276056274,-6.18968707540637));
#51451=CARTESIAN_POINT('Ctrl Pts',(3.53986050381078,0.021304435887652,-6.1962004853681));
#51452=CARTESIAN_POINT('Ctrl Pts',(3.54040097332149,-0.061994742963288,
-6.19900940324467));
#51453=CARTESIAN_POINT('Ctrl Pts',(3.53799699077534,-0.145315513407627,
-6.20181832112124));
#51454=CARTESIAN_POINT('Ctrl Pts',(3.53262128868333,-0.22844437121557,-6.20462723899781));
#51455=CARTESIAN_POINT('Ctrl Pts',(3.5255316382462,-0.338077407609597,-6.20833173108287));
#51456=CARTESIAN_POINT('Ctrl Pts',(3.51327303496331,-0.447376576378206,
-6.21203622316794));
#51457=CARTESIAN_POINT('Ctrl Pts',(3.49597098000898,-0.555864346356779,
-6.215740715253));
#51458=CARTESIAN_POINT('Ctrl Pts',(3.46554970375613,-0.746612579979145,
-6.22225412521464));
#51459=CARTESIAN_POINT('Ctrl Pts',(3.41953925747835,-0.934864572484402,
-6.22876753517627));
#51460=CARTESIAN_POINT('Ctrl Pts',(3.35859301744289,-1.11815333279855,-6.23528094513791));
#51461=CARTESIAN_POINT('Ctrl Pts',(3.31059801777636,-1.2624927372481,-6.24041023791716));
#51462=CARTESIAN_POINT('Ctrl Pts',(3.25333356013243,-1.40376624524555,-6.24553953069642));
#51463=CARTESIAN_POINT('Ctrl Pts',(3.18712845076366,-1.54071809177819,-6.25066882347567));
#51464=CARTESIAN_POINT('Ctrl Pts',(3.16926329207835,-1.57767394751018,-6.25205294065814));
#51465=CARTESIAN_POINT('Ctrl Pts',(3.15074717578934,-1.61431513677177,-6.25343705784061));
#51466=CARTESIAN_POINT('Ctrl Pts',(3.13159534362019,-1.65062121645643,-6.25482117502308));
#51467=CARTESIAN_POINT('Ctrl Pts',(3.04147021836802,-1.82147118788974,-6.2613345849847));
#51468=CARTESIAN_POINT('Ctrl Pts',(2.93727842881738,-1.98488223342344,-6.2678479949463));
#51469=CARTESIAN_POINT('Ctrl Pts',(2.82057762917812,-2.13879529781198,-6.27436140490792));
#51470=CARTESIAN_POINT('Ctrl Pts',(2.70387682953718,-2.29270836220275,-6.28087481486964));
#51471=CARTESIAN_POINT('Ctrl Pts',(2.57465211340251,-2.43714224335224,-6.28738822483137));
#51472=CARTESIAN_POINT('Ctrl Pts',(2.43444850641693,-2.57001604546182,-6.29390163479326));
#51473=CARTESIAN_POINT('Ctrl Pts',(2.41429399083976,-2.58911688867116,-6.2948379489535));
#51474=CARTESIAN_POINT('Ctrl Pts',(2.39391298941519,-2.60797845638822,-6.29577426311375));
#51475=CARTESIAN_POINT('Ctrl Pts',(2.37331023111434,-2.62659447705366,-6.296710577274));
#51476=CARTESIAN_POINT('Ctrl Pts',(2.25059121040597,-2.73747962127514,-6.30228767307559));
#51477=CARTESIAN_POINT('Ctrl Pts',(2.12000384287054,-2.839652015463,-6.30786476887727));
#51478=CARTESIAN_POINT('Ctrl Pts',(1.98297254939446,-2.93225806317012,-6.31344186467883));
#51479=CARTESIAN_POINT('Ctrl Pts',(1.82293567289756,-3.04041133417721,-6.31995527464063));
#51480=CARTESIAN_POINT('Ctrl Pts',(1.65409266030275,-3.13553304456699,-6.32646868460227));
#51481=CARTESIAN_POINT('Ctrl Pts',(1.47862930850234,-3.2163003073892,-6.33298209456391));
#51482=CARTESIAN_POINT('Ctrl Pts',(1.390897632601,-3.25668393880083,-6.33623879954477));
#51483=CARTESIAN_POINT('Ctrl Pts',(1.30150905535828,-3.29347875878619,-6.33949550452563));
#51484=CARTESIAN_POINT('Ctrl Pts',(1.21075130737302,-3.32651187758184,-6.34275220950649));
#51485=CARTESIAN_POINT('Ctrl Pts',(1.1199935593875,-3.35954499637758,-6.34600891448736));
#51486=CARTESIAN_POINT('Ctrl Pts',(1.02786668212491,-3.3888163988914,-6.34926561946823));
#51487=CARTESIAN_POINT('Ctrl Pts',(0.934702221409373,-3.414273576702,-6.3525223244491));
#51488=CARTESIAN_POINT('Ctrl Pts',(0.748373299981275,-3.46518793232237,
-6.35903573441073));
#51489=CARTESIAN_POINT('Ctrl Pts',(0.557888991572958,-3.50085067113629,
-6.36554914437237));
#51490=CARTESIAN_POINT('Ctrl Pts',(0.365774049088018,-3.52087018018125,
-6.372062554334));
#51491=CARTESIAN_POINT('Ctrl Pts',(0.20127596813921,-3.53801184952169,-6.37763965013542));
#51492=CARTESIAN_POINT('Ctrl Pts',(0.0355650918612497,-3.54368319654726,
-6.38321674593683));
#51493=CARTESIAN_POINT('Ctrl Pts',(-0.1297187288212,-3.53762251397617,-6.38879384173825));
#51494=CARTESIAN_POINT('Ctrl Pts',(-0.157467504755981,-3.53660501255357,
-6.38973015589847));
#51495=CARTESIAN_POINT('Ctrl Pts',(-0.185204239670332,-3.53525686860412,
-6.39066647005869));
#51496=CARTESIAN_POINT('Ctrl Pts',(-0.212921279681585,-3.53357984669696,
-6.39160278421891));
#51497=CARTESIAN_POINT('Ctrl Pts',(-0.405733107366116,-3.52191375035853,
-6.39811619418064));
#51498=CARTESIAN_POINT('Ctrl Pts',(-0.597565292296506,-3.49433502470254,
-6.40462960414237));
#51499=CARTESIAN_POINT('Ctrl Pts',(-0.785896702128393,-3.45144460505232,
-6.41114301410408));
#51500=CARTESIAN_POINT('Ctrl Pts',(-0.97422811195755,-3.40855418540273,
-6.4176564240657));
#51501=CARTESIAN_POINT('Ctrl Pts',(-1.15908224871662,-3.35034725338159,
-6.4241698340273));
#51502=CARTESIAN_POINT('Ctrl Pts',(-1.33794234485403,-3.27739989599169,
-6.43068324398892));
#51503=CARTESIAN_POINT('Ctrl Pts',(-1.37595059764031,-3.26189838581898,
-6.43206736117139));
#51504=CARTESIAN_POINT('Ctrl Pts',(-1.41368726809313,-3.24573153652599,
-6.43345147835386));
#51505=CARTESIAN_POINT('Ctrl Pts',(-1.4511275397993,-3.22890521124983,-6.43483559553633));
#51506=CARTESIAN_POINT('Ctrl Pts',(-1.58987454601214,-3.16654983423889,
-6.43996488831558));
#51507=CARTESIAN_POINT('Ctrl Pts',(-1.72455052609608,-3.09513693232657,
-6.44509418109484));
#51508=CARTESIAN_POINT('Ctrl Pts',(-1.85409640965779,-3.01541712473751,
-6.45022347387409));
#51509=CARTESIAN_POINT('Ctrl Pts',(-2.01859968229062,-2.91418527636456,
-6.45673688383573));
#51510=CARTESIAN_POINT('Ctrl Pts',(-2.17485177726832,-2.79955082838338,
-6.46325029379736));
#51511=CARTESIAN_POINT('Ctrl Pts',(-2.32076642803647,-2.67298362342837,
-6.469763703759));
#51512=CARTESIAN_POINT('Ctrl Pts',(-2.40375516543355,-2.60099871663665,
-6.47346819584406));
#51513=CARTESIAN_POINT('Ctrl Pts',(-2.48340195179236,-2.52515037406617,
-6.47717268792913));
#51514=CARTESIAN_POINT('Ctrl Pts',(-2.55930369651983,-2.44572373521217,
-6.48087718001419));
#51515=CARTESIAN_POINT('Ctrl Pts',(-2.61685592304164,-2.38549877032363,
-6.48368609789077));
#51516=CARTESIAN_POINT('Ctrl Pts',(-2.67225503938364,-2.32321660732287,
-6.48649501576734));
#51517=CARTESIAN_POINT('Ctrl Pts',(-2.72538469578074,-2.25905832714279,
-6.48930393364391));
#51518=CARTESIAN_POINT('Ctrl Pts',(-2.84858346785115,-2.11028602420789,
-6.49581734360564));
#51519=CARTESIAN_POINT('Ctrl Pts',(-2.95958197207277,-1.95142785557342,
-6.50233075356736));
#51520=CARTESIAN_POINT('Ctrl Pts',(-3.05700615397888,-1.7846428881584,-6.50884416352909));
#51521=CARTESIAN_POINT('Ctrl Pts',(-3.14712345334602,-1.63036691124576,
-6.51486906313757));
#51522=CARTESIAN_POINT('Ctrl Pts',(-3.22563382835918,-1.46928943033375,
-6.52089396274604));
#51523=CARTESIAN_POINT('Ctrl Pts',(-3.29140876004433,-1.30316091650401,
-6.52691886235452));
#51524=CARTESIAN_POINT('Ctrl Pts',(-3.29674191697551,-1.28969089970129,
-6.52740737270768));
#51525=CARTESIAN_POINT('Ctrl Pts',(-3.3019913531112,-1.2761876799283,-6.52789588306084));
#51526=CARTESIAN_POINT('Ctrl Pts',(-3.30715686163083,-1.26265234730166,
-6.528384393414));
#51527=CARTESIAN_POINT('Ctrl Pts',(-3.37602965916945,-1.08218294722828,
-6.53489780337563));
#51528=CARTESIAN_POINT('Ctrl Pts',(-3.42997151868652,-0.89603342204106,
-6.54141121333727));
#51529=CARTESIAN_POINT('Ctrl Pts',(-3.46851662407281,-0.706764717832116,
-6.54792462329891));
#51530=CARTESIAN_POINT('Ctrl Pts',(-3.50706172945967,-0.517496013620438,
-6.55443803326064));
#51531=CARTESIAN_POINT('Ctrl Pts',(-3.53021639596121,-0.32508495181709,
-6.56095144322237));
#51532=CARTESIAN_POINT('Ctrl Pts',(-3.53749871140976,-0.132059280579998,
-6.56746485318408));
#51533=CARTESIAN_POINT('Ctrl Pts',(-3.53954688521147,-0.0777702119891359,
-6.56929676993332));
#51534=CARTESIAN_POINT('Ctrl Pts',(-3.5403393000852,-0.0234336768277606,
-6.57112868668255));
#51535=CARTESIAN_POINT('Ctrl Pts',(-3.53986520764733,0.0308919356641561,
-6.57296060343179));
#51536=CARTESIAN_POINT('Ctrl Pts',(-3.53865365666892,0.169721926844386,
-6.57764209664417));
#51537=CARTESIAN_POINT('Ctrl Pts',(-3.52917019745509,0.308480469767332,
-6.58232358985654));
#51538=CARTESIAN_POINT('Ctrl Pts',(-3.51161394105595,0.446196758891985,
-6.58700508306892));
#51539=CARTESIAN_POINT('Ctrl Pts',(-3.48718773981356,0.637802857369744,
-6.59351849303064));
#51540=CARTESIAN_POINT('Ctrl Pts',(-3.4471367782153,0.827411723408665,-6.60003190299237));
#51541=CARTESIAN_POINT('Ctrl Pts',(-3.39197035063338,1.01252418815714,-6.6065453129541));
#51542=CARTESIAN_POINT('Ctrl Pts',(-3.35680189836082,1.13053289683955,-6.61069759464808));
#51543=CARTESIAN_POINT('Ctrl Pts',(-3.31548686207736,1.24671997283311,-6.61484987634206));
#51544=CARTESIAN_POINT('Ctrl Pts',(-3.26816416858,1.3604054422155,-6.61900215803608));
#51545=CARTESIAN_POINT('Ctrl Pts',(-3.2412548792897,1.42505085771546,-6.62136328630376));
#51546=CARTESIAN_POINT('Ctrl Pts',(-3.21240318873926,1.48888742428309,-6.62372441457145));
#51547=CARTESIAN_POINT('Ctrl Pts',(-3.1816796260222,1.55180881165512,-6.62608554283917));
#51548=CARTESIAN_POINT('Ctrl Pts',(-3.0969255861,1.72538379143208,-6.63259895280097));
#51549=CARTESIAN_POINT('Ctrl Pts',(-2.9979321353066,1.89198966135704,-6.63911236276294));
#51550=CARTESIAN_POINT('Ctrl Pts',(-2.88612844378586,2.04949663734564,-6.64562577272474));
#51551=CARTESIAN_POINT('Ctrl Pts',(-2.7743247522635,2.20700361333651,-6.65213918268664));
#51552=CARTESIAN_POINT('Ctrl Pts',(-2.64969465291328,2.3554295711336,-6.65865259264837));
#51553=CARTESIAN_POINT('Ctrl Pts',(-2.51368120782473,2.4925903433037,-6.66516600261008));
#51554=CARTESIAN_POINT('Ctrl Pts',(-2.37766776273814,2.62975111547182,-6.6716794125717));
#51555=CARTESIAN_POINT('Ctrl Pts',(-2.23029846571805,2.75562791640694,-6.6781928225333));
#51556=CARTESIAN_POINT('Ctrl Pts',(-2.07374054798118,2.86875662093084,-6.68470623249492));
#51557=CARTESIAN_POINT('Ctrl Pts',(-1.91718263024204,2.98188532545637,-6.69121964245664));
#51558=CARTESIAN_POINT('Ctrl Pts',(-1.75141820912731,3.08228207284204,-6.69773305241837));
#51559=CARTESIAN_POINT('Ctrl Pts',(-1.57856280904735,3.16849459675079,-6.7042464623801));
#51560=CARTESIAN_POINT('Ctrl Pts',(-1.51806293971028,3.19866921917673,-6.70652617392767));
#51561=CARTESIAN_POINT('Ctrl Pts',(-1.45669512500734,3.22710553504123,-6.70880588547525));
#51562=CARTESIAN_POINT('Ctrl Pts',(-1.39455435995192,3.25373910096334,-6.71108559702283));
#51563=CARTESIAN_POINT('Ctrl Pts',(-1.27915148859172,3.30320083480635,-6.71531929543689));
#51564=CARTESIAN_POINT('Ctrl Pts',(-1.16108267271159,3.34644458612958,-6.71955299385094));
#51565=CARTESIAN_POINT('Ctrl Pts',(-1.04106677331439,3.38331569520124,-6.723786692265));
#51566=CARTESIAN_POINT('Ctrl Pts',(-0.85642614041225,3.44004072037697,-6.73030010222663));
#51567=CARTESIAN_POINT('Ctrl Pts',(-0.667162346706339,3.48169169421644,
-6.73681351218827));
#51568=CARTESIAN_POINT('Ctrl Pts',(-0.475768876624546,3.5077327830413,-6.74332692214991));
#51569=CARTESIAN_POINT('Ctrl Pts',(-0.340597831264551,3.5261242213556,-6.74792699775853));
#51570=CARTESIAN_POINT('Ctrl Pts',(-0.20435464586928,3.53672868968354,-6.75252707336715));
#51571=CARTESIAN_POINT('Ctrl Pts',(-0.0679589460948703,3.53934762091083,
-6.75712714897577));
#51572=CARTESIAN_POINT('Ctrl Pts',(-0.0112271442293234,3.54043692715533,
-6.75904048332888));
#51573=CARTESIAN_POINT('Ctrl Pts',(0.045531022636134,3.54014484257323,-6.76095381768199));
#51574=CARTESIAN_POINT('Ctrl Pts',(0.102248860493041,3.53848292849331,-6.76286715203509));
#51575=CARTESIAN_POINT('Ctrl Pts',(0.295328825580806,3.53282540830823,-6.76938056199673));
#51576=CARTESIAN_POINT('Ctrl Pts',(0.487928089795474,3.51129585116066,-6.77589397195837));
#51577=CARTESIAN_POINT('Ctrl Pts',(0.677515362239867,3.47434925711893,-6.78240738192));
#51578=CARTESIAN_POINT('Ctrl Pts',(0.867102634684259,3.43740266307719,-6.78892079188164));
#51579=CARTESIAN_POINT('Ctrl Pts',(1.053701106507,3.38503272719013,-6.79543420184327));
#51580=CARTESIAN_POINT('Ctrl Pts',(1.23474298622044,3.31767899823506,-6.80194761180491));
#51581=CARTESIAN_POINT('Ctrl Pts',(1.24605820178868,3.31346935368399,-6.80235470345639));
#51582=CARTESIAN_POINT('Ctrl Pts',(1.25735159732433,3.30920121986826,-6.80276179510787));
#51583=CARTESIAN_POINT('Ctrl Pts',(1.26862254139057,3.30487470980033,-6.80316888675936));
#51584=CARTESIAN_POINT('Ctrl Pts',(1.43768513914876,3.2399776588513,-6.8092752050696));
#51585=CARTESIAN_POINT('Ctrl Pts',(1.60169567108907,3.16194539799143,-6.81538152337985));
#51586=CARTESIAN_POINT('Ctrl Pts',(1.75882144669102,3.07193280717094,-6.82148784169008));
#51587=CARTESIAN_POINT('Ctrl Pts',(1.92642237085479,2.97591932147712,-6.8280012516517));
#51588=CARTESIAN_POINT('Ctrl Pts',(2.08621238736183,2.86626604784555,-6.8345146616133));
#51589=CARTESIAN_POINT('Ctrl Pts',(2.23601720366442,2.74432457051421,-6.84102807157492));
#51590=CARTESIAN_POINT('Ctrl Pts',(2.29874823302859,2.6932613631756,-6.8437555734113));
#51591=CARTESIAN_POINT('Ctrl Pts',(2.3597278326295,2.64004307078317,-6.84648307524768));
#51592=CARTESIAN_POINT('Ctrl Pts',(2.41878915883033,2.5847744592375,-6.84921057708405));
#51593=CARTESIAN_POINT('Ctrl Pts',(2.50076921536961,2.50805887916477,-6.8529964852094));
#51594=CARTESIAN_POINT('Ctrl Pts',(2.57905316667217,2.42739285957258,-6.85678239333475));
#51595=CARTESIAN_POINT('Ctrl Pts',(2.65333228007531,2.34320336556039,-6.86056830146009));
#51596=CARTESIAN_POINT('Ctrl Pts',(2.78112468843889,2.19836078861232,-6.86708171142173));
#51597=CARTESIAN_POINT('Ctrl Pts',(2.89707465218622,2.04308253276765,-6.87359512138337));
#51598=CARTESIAN_POINT('Ctrl Pts',(2.9996904458398,1.87943880835007,-6.880108531345));
#51599=CARTESIAN_POINT('Ctrl Pts',(3.07921739666291,1.75261538321336,-6.88515640570495));
#51600=CARTESIAN_POINT('Ctrl Pts',(3.15074015167961,1.62075497546953,-6.8902042800649));
#51601=CARTESIAN_POINT('Ctrl Pts',(3.21353227400634,1.48486037185928,-6.89525215442485));
#51602=CARTESIAN_POINT('Ctrl Pts',(3.23176253970101,1.44540646206153,-6.89671769002653));
#51603=CARTESIAN_POINT('Ctrl Pts',(3.2492569706675,1.40561255518628,-6.89818322562822));
#51604=CARTESIAN_POINT('Ctrl Pts',(3.26600829512753,1.36550806014452,-6.89964876122991));
#51605=CARTESIAN_POINT('Ctrl Pts',(3.34045769334387,1.18726809298532,-6.90616217119164));
#51606=CARTESIAN_POINT('Ctrl Pts',(3.4002225314738,1.00291223761149,-6.91267558115337));
#51607=CARTESIAN_POINT('Ctrl Pts',(3.44470072231061,0.814949462094048,-6.91918899111509));
#51608=CARTESIAN_POINT('Ctrl Pts',(3.48917891314677,0.626986686579336,-6.92570240107673));
#51609=CARTESIAN_POINT('Ctrl Pts',(3.51837528864164,0.435393488100818,-6.93221581103837));
#51610=CARTESIAN_POINT('Ctrl Pts',(3.53166214900558,0.242686469356258,-6.938729221));
#51611=CARTESIAN_POINT('Ctrl Pts',(3.53340607022177,0.217393371567027,-6.9395841162507));
#51612=CARTESIAN_POINT('Ctrl Pts',(3.53487587375559,0.192081558293536,-6.9404390115014));
#51613=CARTESIAN_POINT('Ctrl Pts',(3.53607015736517,0.16675683551214,-6.9412939067521));
#51614=CARTESIAN_POINT('Ctrl Pts',(3.54397506895323,-0.000866409899313997,
-6.94695242146303));
#51615=CARTESIAN_POINT('Ctrl Pts',(3.53980817195322,-0.169055081500192,
-6.95261093617397));
#51616=CARTESIAN_POINT('Ctrl Pts',(3.52382484364409,-0.336095312099889,
-6.95826945088491));
#51617=CARTESIAN_POINT('Ctrl Pts',(3.50542673475007,-0.52837218290042,-6.96478286084664));
#51618=CARTESIAN_POINT('Ctrl Pts',(3.47137388730705,-0.719151067248053,
-6.97129627080837));
#51619=CARTESIAN_POINT('Ctrl Pts',(3.42203117938897,-0.905902528285193,
-6.97780968077025));
#51620=CARTESIAN_POINT('Ctrl Pts',(3.39797659515054,-0.99694391901358,-6.98098496999166));
#51621=CARTESIAN_POINT('Ctrl Pts',(3.37028711544748,-1.08702913815711,-6.9841602592131));
#51622=CARTESIAN_POINT('Ctrl Pts',(3.33900820913433,-1.17585040686805,-6.98733554843455));
#51623=CARTESIAN_POINT('Ctrl Pts',(3.30612529402972,-1.2692265054204,-6.99067366917496));
#51624=CARTESIAN_POINT('Ctrl Pts',(3.2692753640432,-1.3612056436035,-6.99401178991538));
#51625=CARTESIAN_POINT('Ctrl Pts',(3.2286413672435,-1.45147605409633,-6.99734991065576));
#51626=CARTESIAN_POINT('Ctrl Pts',(3.14935547553055,-1.62761353883595,-7.00386332061764));
#51627=CARTESIAN_POINT('Ctrl Pts',(3.05566316088876,-1.79725369188204,-7.01037673057937));
#51628=CARTESIAN_POINT('Ctrl Pts',(2.94886369882296,-1.95819733025196,-7.0168901405411));
#51629=CARTESIAN_POINT('Ctrl Pts',(2.85875186152997,-2.09399321043342,-7.02238581746063));
#51630=CARTESIAN_POINT('Ctrl Pts',(2.75929726145042,-2.22360994758072,-7.02788149438017));
#51631=CARTESIAN_POINT('Ctrl Pts',(2.65130325159267,-2.34567497068367,-7.0333771712997));
#51632=CARTESIAN_POINT('Ctrl Pts',(2.63130406426958,-2.36827993984675,-7.03439490434181));
#51633=CARTESIAN_POINT('Ctrl Pts',(2.61101205412421,-2.39062594672813,-7.0354126373839));
#51634=CARTESIAN_POINT('Ctrl Pts',(2.5904352191543,-2.41270682914795,-7.036430370426));
#51635=CARTESIAN_POINT('Ctrl Pts',(2.45874512329616,-2.55402270822995,-7.04294378038764));
#51636=CARTESIAN_POINT('Ctrl Pts',(2.3154071367893,-2.68446116186662,-7.04945719034927));
#51637=CARTESIAN_POINT('Ctrl Pts',(2.1624843817763,-2.80245664730059,-7.05597060031091));
#51638=CARTESIAN_POINT('Ctrl Pts',(2.00956162676109,-2.92045213273626,-7.06248401027264));
#51639=CARTESIAN_POINT('Ctrl Pts',(1.84703531539659,-3.02601956514964,-7.06899742023437));
#51640=CARTESIAN_POINT('Ctrl Pts',(1.67694939807015,-3.11757873618206,-7.0755108301961));
#51641=CARTESIAN_POINT('Ctrl Pts',(1.64293177974845,-3.13589080447667,-7.07681352884119));
#51642=CARTESIAN_POINT('Ctrl Pts',(1.60861252646917,-3.15364206036475,-7.07811622748629));
#51643=CARTESIAN_POINT('Ctrl Pts',(1.57400853431423,-3.17081963124785,-7.07941892613138));
#51644=CARTESIAN_POINT('Ctrl Pts',(1.43559477745792,-3.2395288168513,-7.08462963744792));
#51645=CARTESIAN_POINT('Ctrl Pts',(1.29262501833188,-3.29905833593406,-7.08984034876446));
#51646=CARTESIAN_POINT('Ctrl Pts',(1.14641104468838,-3.34905016806174,-7.095051060081));
#51647=CARTESIAN_POINT('Ctrl Pts',(0.963642993532519,-3.41154015793072,
-7.10156447004264));
#51648=CARTESIAN_POINT('Ctrl Pts',(0.775786184883246,-3.45913891306697,
-7.10807788000427));
#51649=CARTESIAN_POINT('Ctrl Pts',(0.585300931640267,-3.49116675003133,
-7.11459128996591));
#51650=CARTESIAN_POINT('Ctrl Pts',(0.479343748210392,-3.50898219421044,
-7.11821436609547));
#51651=CARTESIAN_POINT('Ctrl Pts',(0.372569808297704,-3.52197909098866,
-7.12183744222504));
#51652=CARTESIAN_POINT('Ctrl Pts',(0.265424692965157,-3.53003537267917,
-7.1254605183546));
#51653=CARTESIAN_POINT('Ctrl Pts',(0.1799489423262,-3.53646232665386,-7.12835085218676));
#51654=CARTESIAN_POINT('Ctrl Pts',(0.0942370119385343,-3.53974508577457,
-7.13124118601892));
#51655=CARTESIAN_POINT('Ctrl Pts',(0.00852186074184726,-3.53991094251116,
-7.13413151985108));
#51656=CARTESIAN_POINT('Ctrl Pts',(-0.184638497918042,-3.54028470311567,
-7.1406449298127));
#51657=CARTESIAN_POINT('Ctrl Pts',(-0.377816489562962,-3.52483316308227,
-7.1471583397743));
#51658=CARTESIAN_POINT('Ctrl Pts',(-0.568472409011395,-3.49386453342436,
-7.15367174973592));
#51659=CARTESIAN_POINT('Ctrl Pts',(-0.742445766719096,-3.46560568627825,
-7.15961523055953));
#51660=CARTESIAN_POINT('Ctrl Pts',(-0.914338116430782,-3.42442020539666,
-7.16555871138316));
#51661=CARTESIAN_POINT('Ctrl Pts',(-1.08216137956925,-3.37053805030733,
-7.17150219220678));
#51662=CARTESIAN_POINT('Ctrl Pts',(-1.09825419967799,-3.36537121102231,
-7.17207212134489));
#51663=CARTESIAN_POINT('Ctrl Pts',(-1.11430960469959,-3.3600876333587,-7.17264205048299));
#51664=CARTESIAN_POINT('Ctrl Pts',(-1.13032604705382,-3.35468816325393,
-7.17321197962109));
#51665=CARTESIAN_POINT('Ctrl Pts',(-1.31336925050718,-3.29298055784017,
-7.17972538958273));
#51666=CARTESIAN_POINT('Ctrl Pts',(-1.49129514513555,-3.21614619228149,
-7.18623879954437));
#51667=CARTESIAN_POINT('Ctrl Pts',(-1.66183108821857,-3.12544975106934,
-7.192752209506));
#51668=CARTESIAN_POINT('Ctrl Pts',(-1.83236703130161,-3.0347533098572,-7.19926561946763));
#51669=CARTESIAN_POINT('Ctrl Pts',(-1.99553483595644,-2.93018474734963,
-7.20577902942927));
#51670=CARTESIAN_POINT('Ctrl Pts',(-2.14907398699859,-2.81297668049842,
-7.21229243939091));
#51671=CARTESIAN_POINT('Ctrl Pts',(-2.19033810662407,-2.78147665162115,
-7.21404293837441));
#51672=CARTESIAN_POINT('Ctrl Pts',(-2.23090577145553,-2.74906427885111,
-7.21579343735791));
#51673=CARTESIAN_POINT('Ctrl Pts',(-2.27073169575485,-2.71576463742649,
-7.21754393634141));
#51674=CARTESIAN_POINT('Ctrl Pts',(-2.37909355934424,-2.62516005598574,
-7.22230684731964));
#51675=CARTESIAN_POINT('Ctrl Pts',(-2.48196353080434,-2.52798626286371,
-7.22706975829786));
#51676=CARTESIAN_POINT('Ctrl Pts',(-2.57868524344307,-2.42505371417111,
-7.23183266927608));
#51677=CARTESIAN_POINT('Ctrl Pts',(-2.71095480915343,-2.28429066168171,
-7.2383460792377));
#51678=CARTESIAN_POINT('Ctrl Pts',(-2.83174365337413,-2.13274635689841,
-7.2448594891993));
#51679=CARTESIAN_POINT('Ctrl Pts',(-2.93944340626971,-1.97240050926644,
-7.25137289916092));
#51680=CARTESIAN_POINT('Ctrl Pts',(-3.00675548551217,-1.8721847509957,-7.25544376428074));
#51681=CARTESIAN_POINT('Ctrl Pts',(-3.0689565651283,-1.76852498435215,-7.25951462940056));
#51682=CARTESIAN_POINT('Ctrl Pts',(-3.12563447872083,-1.66192933226244,
-7.26358549452038));
#51683=CARTESIAN_POINT('Ctrl Pts',(-3.15964158566754,-1.59797126622053,
-7.26602803936228));
#51684=CARTESIAN_POINT('Ctrl Pts',(-3.19166042350247,-1.53295634899612,
-7.26847058420419));
#51685=CARTESIAN_POINT('Ctrl Pts',(-3.22164958182273,-1.467019693314,-7.2709131290461));
#51686=CARTESIAN_POINT('Ctrl Pts',(-3.30162014334238,-1.29118977093615,
-7.27742653900773));
#51687=CARTESIAN_POINT('Ctrl Pts',(-3.36715796958855,-1.10881135569454,
-7.28393994896937));
#51688=CARTESIAN_POINT('Ctrl Pts',(-3.41752451187652,-0.92233949801837,
-7.290453358931));
#51689=CARTESIAN_POINT('Ctrl Pts',(-3.46694667627976,-0.739364006987898,
-7.29684464178121));
#51690=CARTESIAN_POINT('Ctrl Pts',(-3.50176440608703,-0.552424156172237,
-7.30323592463143));
#51691=CARTESIAN_POINT('Ctrl Pts',(-3.52124797259483,-0.363885580226897,
-7.3096272074818));
#51692=CARTESIAN_POINT('Ctrl Pts',(-3.52162027213994,-0.360282911997128,
-7.30974933459322));
#51693=CARTESIAN_POINT('Ctrl Pts',(-3.52198697295808,-0.35667966015706,
-7.30987146170465));
#51694=CARTESIAN_POINT('Ctrl Pts',(-3.52234807653483,-0.353075841902743,
-7.30999358881607));
#51695=CARTESIAN_POINT('Ctrl Pts',(-3.54160682757397,-0.160873263421083,
-7.31650699877797));
#51696=CARTESIAN_POINT('Ctrl Pts',(-3.54494113425226,0.0329083541594109,
-7.32302040874003));
#51697=CARTESIAN_POINT('Ctrl Pts',(-3.53259533909181,0.22566737745008,-7.32953381870193));
#51698=CARTESIAN_POINT('Ctrl Pts',(-3.52024954393154,0.418426400737956,
-7.33604722866373));
#51699=CARTESIAN_POINT('Ctrl Pts',(-3.49222452843905,0.610186888018826,
-7.34256063862537));
#51700=CARTESIAN_POINT('Ctrl Pts',(-3.44874073224416,0.798391072008908,
-7.349074048587));
#51701=CARTESIAN_POINT('Ctrl Pts',(-3.43406482543378,0.861910527697223,
-7.35127234326179));
#51702=CARTESIAN_POINT('Ctrl Pts',(-3.4176279918563,0.925023822733724,-7.35347063793657));
#51703=CARTESIAN_POINT('Ctrl Pts',(-3.399439647296,0.987628515379085,-7.35566893261136));
#51704=CARTESIAN_POINT('Ctrl Pts',(-3.36373706176239,1.11051762090298,-7.35998404789821));
#51705=CARTESIAN_POINT('Ctrl Pts',(-3.32128518726173,1.23144678337572,-7.36429916318506));
#51706=CARTESIAN_POINT('Ctrl Pts',(-3.27244048985516,1.34972428826295,-7.36861427847191));
#51707=CARTESIAN_POINT('Ctrl Pts',(-3.19871232327865,1.52825714946575,-7.37512768843364));
#51708=CARTESIAN_POINT('Ctrl Pts',(-3.11041628697104,1.7007662450445,-7.38164109839537));
#51709=CARTESIAN_POINT('Ctrl Pts',(-3.00872059248994,1.86498453844867,-7.38815450835708));
#51710=CARTESIAN_POINT('Ctrl Pts',(-2.9381695165832,1.97891047545466,-7.39267316652609));
#51711=CARTESIAN_POINT('Ctrl Pts',(-2.86116271344563,2.08885271017646,-7.3971918246951));
#51712=CARTESIAN_POINT('Ctrl Pts',(-2.77810835168668,2.19401777255465,-7.40171048286411));
#51713=CARTESIAN_POINT('Ctrl Pts',(-2.74144418484653,2.24044265995526,-7.40370523465671));
#51714=CARTESIAN_POINT('Ctrl Pts',(-2.70360160799484,2.2859366567572,-7.40569998644932));
#51715=CARTESIAN_POINT('Ctrl Pts',(-2.66463875530979,2.33044965099088,-7.40769473824192));
#51716=CARTESIAN_POINT('Ctrl Pts',(-2.53741438897186,2.47579674687627,-7.41420814820364));
#51717=CARTESIAN_POINT('Ctrl Pts',(-2.39825532545772,2.61067669790369,-7.42072155816537));
#51718=CARTESIAN_POINT('Ctrl Pts',(-2.24911868144474,2.73342304268973,-7.4272349681271));
#51719=CARTESIAN_POINT('Ctrl Pts',(-2.09998203743392,2.85616938747399,-7.43374837808873));
#51720=CARTESIAN_POINT('Ctrl Pts',(-1.94084807500285,2.96679585561946,-7.44026178805037));
#51721=CARTESIAN_POINT('Ctrl Pts',(-1.7736881360114,3.06359595272342,-7.446775198012));
#51722=CARTESIAN_POINT('Ctrl Pts',(-1.76533007352107,3.0684359955324,-7.44710087106389));
#51723=CARTESIAN_POINT('Ctrl Pts',(-1.75695201419097,3.07324143239533,-7.44742654411577));
#51724=CARTESIAN_POINT('Ctrl Pts',(-1.74855420770786,3.07801205044834,-7.44775221716766));
#51725=CARTESIAN_POINT('Ctrl Pts',(-1.58899720157694,3.16865304526785,-7.45393995407741));
#51726=CARTESIAN_POINT('Ctrl Pts',(-1.42231138155771,3.24672375067996,-7.46012769098716));
#51727=CARTESIAN_POINT('Ctrl Pts',(-1.25063380441199,3.31151429393604,-7.46631542789691));
#51728=CARTESIAN_POINT('Ctrl Pts',(-1.0699204907246,3.37971489393329,-7.47282883785864));
#51729=CARTESIAN_POINT('Ctrl Pts',(-0.883654985072044,3.43321218577804,
-7.47934224782037));
#51730=CARTESIAN_POINT('Ctrl Pts',(-0.69426261018899,3.47118330719089,-7.4858556577821));
#51731=CARTESIAN_POINT('Ctrl Pts',(-0.61732158273511,3.48660915047991,-7.48850174348113));
#51732=CARTESIAN_POINT('Ctrl Pts',(-0.539864762333473,3.49947197571339,
-7.49114782918016));
#51733=CARTESIAN_POINT('Ctrl Pts',(-0.462062720458959,3.5097148092635,-7.49379391487919));
#51734=CARTESIAN_POINT('Ctrl Pts',(-0.34835297767497,3.52468498151477,-7.4976612391418));
#51735=CARTESIAN_POINT('Ctrl Pts',(-0.233905849409282,3.53405841436472,
-7.5015285634044));
#51736=CARTESIAN_POINT('Ctrl Pts',(-0.119281726467647,3.53786972306194,
-7.505395887667));
#51737=CARTESIAN_POINT('Ctrl Pts',(0.0737700720151849,3.54428879070397,
-7.51190929762864));
#51738=CARTESIAN_POINT('Ctrl Pts',(0.267337123262925,3.53493519022353,-7.51842270759027));
#51739=CARTESIAN_POINT('Ctrl Pts',(0.45887316707087,3.50996979757638,-7.52493611755191));
#51740=CARTESIAN_POINT('Ctrl Pts',(0.604918840965994,3.49093375861096,-7.52990257362091));
#51741=CARTESIAN_POINT('Ctrl Pts',(0.749795644587637,3.46281672251746,-7.53486902968991));
#51742=CARTESIAN_POINT('Ctrl Pts',(0.892325528180709,3.42569046350633,-7.5398354857589));
#51743=CARTESIAN_POINT('Ctrl Pts',(0.936720798206521,3.4141263602299,-7.54138243965163));
#51744=CARTESIAN_POINT('Ctrl Pts',(0.98088838046976,3.40168827258433,-7.54292939354435));
#51745=CARTESIAN_POINT('Ctrl Pts',(1.02479609483758,3.38839156064891,-7.54447634743708));
#51746=CARTESIAN_POINT('Ctrl Pts',(1.2096684077747,3.33240609373605,-7.5509897573987));
#51747=CARTESIAN_POINT('Ctrl Pts',(1.38991621050558,3.26120588847558,-7.5575031673603));
#51748=CARTESIAN_POINT('Ctrl Pts',(1.56321999725237,3.17591743890142,-7.56401657732192));
#51749=CARTESIAN_POINT('Ctrl Pts',(1.73652378400167,3.09062898932603,-7.57052998728364));
#51750=CARTESIAN_POINT('Ctrl Pts',(1.90290467519647,2.99124089947101,-7.57704339724536));
#51751=CARTESIAN_POINT('Ctrl Pts',(2.06001785169516,2.87886643810324,-7.58355680720709));
#51752=CARTESIAN_POINT('Ctrl Pts',(2.07867525608196,2.86552181726869,-7.5843302835399));
#51753=CARTESIAN_POINT('Ctrl Pts',(2.09720163827227,2.85199428966467,-7.5851037598727));
#51754=CARTESIAN_POINT('Ctrl Pts',(2.11559302029352,2.83828578062299,-7.5858772362055));
#51755=CARTESIAN_POINT('Ctrl Pts',(2.25207465220354,2.73655554181339,-7.59161716983433));
#51756=CARTESIAN_POINT('Ctrl Pts',(2.38112092105923,2.62485779238668,-7.59735710346317));
#51757=CARTESIAN_POINT('Ctrl Pts',(2.50151996034344,2.50453286898932,-7.603097037092));
#51758=CARTESIAN_POINT('Ctrl Pts',(2.63814319548082,2.36799373711636,-7.60961044705364));
#51759=CARTESIAN_POINT('Ctrl Pts',(2.76365118020096,2.22033192223027,-7.61612385701527));
#51760=CARTESIAN_POINT('Ctrl Pts',(2.87632012344211,2.06343515614491,-7.6226372669769));
#51761=CARTESIAN_POINT('Ctrl Pts',(2.92983793594804,1.98890910248192,-7.62573114043549));
#51762=CARTESIAN_POINT('Ctrl Pts',(2.98045881580538,1.91229818395693,-7.62882501389408));
#51763=CARTESIAN_POINT('Ctrl Pts',(3.02798948096801,1.83381561318099,-7.63191888735267));
#51764=CARTESIAN_POINT('Ctrl Pts',(3.08052325350839,1.74707191819124,-7.63533842385581));
#51765=CARTESIAN_POINT('Ctrl Pts',(3.12928194035441,1.65804182176638,-7.63875796035895));
#51766=CARTESIAN_POINT('Ctrl Pts',(3.17413145383252,1.5670900227261,-7.64217749686209));
#51767=CARTESIAN_POINT('Ctrl Pts',(3.25955919165442,1.39384831194062,-7.64869090682373));
#51768=CARTESIAN_POINT('Ctrl Pts',(3.33081116461456,1.21362870349055,-7.65520431678536));
#51769=CARTESIAN_POINT('Ctrl Pts',(3.38701269619474,1.02883041976208,-7.66171772674717));
#51770=CARTESIAN_POINT('Ctrl Pts',(3.43373009893555,0.87521724225577,-7.66713198482601));
#51771=CARTESIAN_POINT('Ctrl Pts',(3.47004976409285,0.718424299931465,-7.67254624290497));
#51772=CARTESIAN_POINT('Ctrl Pts',(3.49544487589833,0.559879558080886,-7.67796050098386));
#51773=CARTESIAN_POINT('Ctrl Pts',(3.50060035326059,0.527693291929511,-7.67905965286682));
#51774=CARTESIAN_POINT('Ctrl Pts',(3.50530563687768,0.495434842487014,-7.68015880474978));
#51775=CARTESIAN_POINT('Ctrl Pts',(3.50956112158859,0.463116931447565,-7.68125795663274));
#51776=CARTESIAN_POINT('Ctrl Pts',(3.53477848866818,0.271605815489876,-7.68777136659463));
#51777=CARTESIAN_POINT('Ctrl Pts',(3.54419862852173,0.0780313815552228,
-7.69428477655637));
#51778=CARTESIAN_POINT('Ctrl Pts',(3.53792067981413,-0.115020209061044,
-7.70079818651808));
#51779=CARTESIAN_POINT('Ctrl Pts',(3.53164273110663,-0.308071799674505,
-7.7073115964797));
#51780=CARTESIAN_POINT('Ctrl Pts',(3.50966604727128,-0.500624506508935,
-7.7138250064413));
#51781=CARTESIAN_POINT('Ctrl Pts',(3.47206668295341,-0.690093950472241,
-7.72033841640292));
#51782=CARTESIAN_POINT('Ctrl Pts',(3.46501671280743,-0.725619921396251,
-7.72155969624664));
#51783=CARTESIAN_POINT('Ctrl Pts',(3.45741761512174,-0.761036669986838,
-7.72278097609036));
#51784=CARTESIAN_POINT('Ctrl Pts',(3.44927002934,-0.796326732377223,-7.72400225593407));
#51785=CARTESIAN_POINT('Ctrl Pts',(3.41396437492646,-0.949247951050361,
-7.72929438605207));
#51786=CARTESIAN_POINT('Ctrl Pts',(3.36835867813816,-1.09978996669337,-7.73458651617007));
#51787=CARTESIAN_POINT('Ctrl Pts',(3.31303614425419,-1.24665390493681,-7.739878646288));
#51788=CARTESIAN_POINT('Ctrl Pts',(3.24494668131607,-1.42741002686256,-7.74639205542224));
#51789=CARTESIAN_POINT('Ctrl Pts',(3.16213450638776,-1.60261748080289,-7.75290546455638));
#51790=CARTESIAN_POINT('Ctrl Pts',(3.06563512458071,-1.76994524026474,-7.75941887369107));
#51791=CARTESIAN_POINT('Ctrl Pts',(0.4410246309536,-3.491069428017,-4.85718848779));
#51792=CARTESIAN_POINT('Ctrl Pts',(-0.007831201098047,-3.547773106292,-4.872535710012));
#51793=CARTESIAN_POINT('Ctrl Pts',(-0.9274923506371,-3.485867209753,-4.903230154456));
#51794=CARTESIAN_POINT('Ctrl Pts',(-2.170848424879,-2.880804771784,-4.949271821123));
#51795=CARTESIAN_POINT('Ctrl Pts',(-3.09517319399,-1.85242382625,-4.99531348779));
#51796=CARTESIAN_POINT('Ctrl Pts',(-3.564695695909,-0.5518440355064,-5.041355154456));
#51797=CARTESIAN_POINT('Ctrl Pts',(-3.510409115218,0.8298255998088,-5.087396821123));
#51798=CARTESIAN_POINT('Ctrl Pts',(-2.940294193437,2.08955828983,-5.13343848779));
#51799=CARTESIAN_POINT('Ctrl Pts',(-1.938124180797,3.042245589626,-5.179480154456));
#51800=CARTESIAN_POINT('Ctrl Pts',(-0.6511609504327,3.5478969849,-5.225521821123));
#51801=CARTESIAN_POINT('Ctrl Pts',(0.7314856681681,3.532210684072,-5.27156348779));
#51802=CARTESIAN_POINT('Ctrl Pts',(2.006645775638,2.997491672717,-5.317605154456));
#51803=CARTESIAN_POINT('Ctrl Pts',(2.986943859211,2.022313027209,-5.363646821123));
#51804=CARTESIAN_POINT('Ctrl Pts',(3.528332232803,0.7499701678353,-5.40968848779));
#51805=CARTESIAN_POINT('Ctrl Pts',(3.551257806707,-0.6325753616011,-5.455730154456));
#51806=CARTESIAN_POINT('Ctrl Pts',(3.052351834218,-1.922168535253,-5.501771821123));
#51807=CARTESIAN_POINT('Ctrl Pts',(2.104924925093,-2.929313000944,-5.54781348779));
#51808=CARTESIAN_POINT('Ctrl Pts',(0.8481945836498,-3.506016193067,-5.593855154456));
#51809=CARTESIAN_POINT('Ctrl Pts',(-0.5331717924892,-3.567535765409,-5.639896821123));
#51810=CARTESIAN_POINT('Ctrl Pts',(-1.836192445479,-3.104831863555,-5.68593848779));
#51811=CARTESIAN_POINT('Ctrl Pts',(-2.869397952564,-2.185895465844,-5.731980154456));
#51812=CARTESIAN_POINT('Ctrl Pts',(-3.480966267353,-0.9457576028406,-5.778021821123));
#51813=CARTESIAN_POINT('Ctrl Pts',(-3.581031867039,0.4333524720513,-5.82406348779));
#51814=CARTESIAN_POINT('Ctrl Pts',(-3.154890838399,1.74878454807,-5.870105154456));
#51815=CARTESIAN_POINT('Ctrl Pts',(-2.265161511065,2.807245433975,-5.916146821123));
#51816=CARTESIAN_POINT('Ctrl Pts',(-1.042583148702,3.453201988854,-5.96218848779));
#51817=CARTESIAN_POINT('Ctrl Pts',(0.3331952363912,3.591735587738,-6.008230154456));
#51818=CARTESIAN_POINT('Ctrl Pts',(1.660013001075,3.202489724268,-6.054271821123));
#51819=CARTESIAN_POINT('Ctrl Pts',(2.742903909839,2.342661251476,-6.10031348779));
#51820=CARTESIAN_POINT('Ctrl Pts',(3.422745007318,1.138595719585,-6.146355154456));
#51821=CARTESIAN_POINT('Ctrl Pts',(3.599638581068,-0.2327781851084,-6.192396821123));
#51822=CARTESIAN_POINT('Ctrl Pts',(3.247591404983,-1.569947025876,-6.23843848779));
#51823=CARTESIAN_POINT('Ctrl Pts',(2.418334255113,-2.676423551744,-6.284480154456));
#51824=CARTESIAN_POINT('Ctrl Pts',(1.233720447776,-3.389619072185,-6.330521821123));
#51825=CARTESIAN_POINT('Ctrl Pts',(-0.1321796203991,-3.604734684513,-6.37656348779));
#51826=CARTESIAN_POINT('Ctrl Pts',(-1.478656853211,-3.290160711611,-6.422605154456));
#51827=CARTESIAN_POINT('Ctrl Pts',(-2.607856199071,-2.492121514442,-6.468646821123));
#51828=CARTESIAN_POINT('Ctrl Pts',(-3.353850014061,-1.327883157873,-6.51468848779));
#51829=CARTESIAN_POINT('Ctrl Pts',(-3.607019924283,0.03147798599785,-6.560730154456));
#51830=CARTESIAN_POINT('Ctrl Pts',(-3.330164449886,1.386213668412,-6.606771821123));
#51831=CARTESIAN_POINT('Ctrl Pts',(-2.563965492379,2.537255318581,-6.65281348779));
#51832=CARTESIAN_POINT('Ctrl Pts',(-1.421010424628,3.315465724582,-6.698855154456));
#51833=CARTESIAN_POINT('Ctrl Pts',(-0.06924819399,3.606492518418,-6.744896821123));
#51834=CARTESIAN_POINT('Ctrl Pts',(1.292689555892,3.367571426097,-6.79093848779));
#51835=CARTESIAN_POINT('Ctrl Pts',(2.464675962715,2.633810167152,-6.836980154456));
#51836=CARTESIAN_POINT('Ctrl Pts',(3.274496134663,1.513029630198,-6.883021821123));
#51837=CARTESIAN_POINT('Ctrl Pts',(3.603152878174,0.1699203763192,-6.92906348779));
#51838=CARTESIAN_POINT('Ctrl Pts',(3.402352471409,-1.198157442941,-6.975105154456));
#51839=CARTESIAN_POINT('Ctrl Pts',(2.701601075983,-2.390174726673,-7.021146821123));
#51840=CARTESIAN_POINT('Ctrl Pts',(1.603869020775,-3.230973191157,-7.06718848779));
#51841=CARTESIAN_POINT('Ctrl Pts',(0.2704600598501,-3.5970036077,-7.113230154456));
#51842=CARTESIAN_POINT('Ctrl Pts',(-1.102691042857,-3.434480464608,-7.159271821123));
#51843=CARTESIAN_POINT('Ctrl Pts',(-2.313809704281,-2.767285357563,-7.20531348779));
#51844=CARTESIAN_POINT('Ctrl Pts',(-3.184930831936,-1.693457762528,-7.251355154456));
#51845=CARTESIAN_POINT('Ctrl Pts',(-3.588049502055,-0.3707888467895,-7.297396821123));
#51846=CARTESIAN_POINT('Ctrl Pts',(-3.463930353097,1.00636479757,-7.34343848779));
#51847=CARTESIAN_POINT('Ctrl Pts',(-2.830811793846,2.235640442297,-7.389480154456));
#51848=CARTESIAN_POINT('Ctrl Pts',(-1.781725994683,3.136404960891,-7.435521821123));
#51849=CARTESIAN_POINT('Ctrl Pts',(-0.4708285118613,3.576297537987,-7.48156348779));
#51850=CARTESIAN_POINT('Ctrl Pts',(0.9092538495968,3.490679192871,-7.527605154456));
#51851=CARTESIAN_POINT('Ctrl Pts',(2.155727782029,2.892130773684,-7.573646821123));
#51852=CARTESIAN_POINT('Ctrl Pts',(3.085433837764,1.868605168765,-7.61968848779));
#51853=CARTESIAN_POINT('Ctrl Pts',(3.561755309148,0.5705000005301,-7.665730154456));
#51854=CARTESIAN_POINT('Ctrl Pts',(3.514711985961,-0.8114300171164,-7.711771821123));
#51855=CARTESIAN_POINT('Ctrl Pts',(2.951172612682,-2.074148614413,-7.75781348779));
#51856=CARTESIAN_POINT('Ctrl Pts',(2.286463642788,-2.712718074487,-7.788507932234));
#51857=CARTESIAN_POINT('Ctrl Pts',(1.906171705064,-2.957799504219,-7.803855154456));
#51858=CARTESIAN_POINT('Ctrl Pts',(0.4620124040095,-3.657204758643,-4.953869121321));
#51859=CARTESIAN_POINT('Ctrl Pts',(-0.008203877497198,-3.716606889221,-4.969216343543));
#51860=CARTESIAN_POINT('Ctrl Pts',(-0.9716304726375,-3.65175497376,-4.999910787988));
#51861=CARTESIAN_POINT('Ctrl Pts',(-2.274156201548,-3.017898422626,-5.045952454654));
#51862=CARTESIAN_POINT('Ctrl Pts',(-3.242468351686,-1.94057820163,-5.091994121321));
#51863=CARTESIAN_POINT('Ctrl Pts',(-3.734334802272,-0.5781055559897,-5.138035787988));
#51864=CARTESIAN_POINT('Ctrl Pts',(-3.677464795723,0.8693158916029,-5.184077454654));
#51865=CARTESIAN_POINT('Ctrl Pts',(-3.080218866387,2.188997577561,-5.230119121321));
#51866=CARTESIAN_POINT('Ctrl Pts',(-2.030356921569,3.187021993332,-5.276160787988));
#51867=CARTESIAN_POINT('Ctrl Pts',(-0.6821488302275,3.716736663046,-5.322202454654));
#51868=CARTESIAN_POINT('Ctrl Pts',(0.7662960939803,3.700303872116,-5.368244121321));
#51869=CARTESIAN_POINT('Ctrl Pts',(2.102139367575,3.140138297301,-5.414285787988));
#51870=CARTESIAN_POINT('Ctrl Pts',(3.129088527441,2.11855220272,-5.460327454654));
#51871=CARTESIAN_POINT('Ctrl Pts',(3.696240850532,0.7856602462946,-5.506369121321));
#51872=CARTESIAN_POINT('Ctrl Pts',(3.720257421874,-0.6626787780505,-5.552410787988));
#51873=CARTESIAN_POINT('Ctrl Pts',(3.197609180605,-2.013641968167,-5.598452454654));
#51874=CARTESIAN_POINT('Ctrl Pts',(2.20509549047,-3.068715093613,-5.644494121321));
#51875=CARTESIAN_POINT('Ctrl Pts',(0.8885590308471,-3.672862820275,-5.690535787988));
#51876=CARTESIAN_POINT('Ctrl Pts',(-0.5585447258702,-3.737310026886,-5.736577454654));
#51877=CARTESIAN_POINT('Ctrl Pts',(-1.92357439113,-3.252586664433,-5.782619121321));
#51878=CARTESIAN_POINT('Ctrl Pts',(-3.005948768117,-2.289919311093,-5.828660787988));
#51879=CARTESIAN_POINT('Ctrl Pts',(-3.646620802058,-0.9907649437943,-5.874702454654));
#51880=CARTESIAN_POINT('Ctrl Pts',(-3.751448389963,0.4539751373136,-5.920744121321));
#51881=CARTESIAN_POINT('Ctrl Pts',(-3.30502787902,1.832006868644,-5.966785787988));
#51882=CARTESIAN_POINT('Ctrl Pts',(-2.372957521519,2.940838494192,-6.012827454654));
#51883=CARTESIAN_POINT('Ctrl Pts',(-1.092198288041,3.617535258634,-6.058869121321));
#51884=CARTESIAN_POINT('Ctrl Pts',(0.3490515526009,3.762661486433,-6.104910787988));
#51885=CARTESIAN_POINT('Ctrl Pts',(1.739010802311,3.354891932284,-6.150952454654));
#51886=CARTESIAN_POINT('Ctrl Pts',(2.873435042872,2.454145371051,-6.196994121321));
#51887=CARTESIAN_POINT('Ctrl Pts',(3.585628870032,1.192779968917,-6.243035787988));
#51888=CARTESIAN_POINT('Ctrl Pts',(3.770940572659,-0.2438557879871,-6.289077454654));
#51889=CARTESIAN_POINT('Ctrl Pts',(3.402139941737,-1.644658707665,-6.335119121321));
#51890=CARTESIAN_POINT('Ctrl Pts',(2.533419551845,-2.803790973341,-6.381160787988));
#51891=CARTESIAN_POINT('Ctrl Pts',(1.292431555853,-3.550926515896,-6.427202454654));
#51892=CARTESIAN_POINT('Ctrl Pts',(-0.1384698719652,-3.776279192858,-6.473244121321));
#51893=CARTESIAN_POINT('Ctrl Pts',(-1.549024157631,-3.446735064802,-6.519285787988));
#51894=CARTESIAN_POINT('Ctrl Pts',(-2.731960591949,-2.610718248279,-6.565327454654));
#51895=CARTESIAN_POINT('Ctrl Pts',(-3.513455256077,-1.391075343539,-6.611369121321));
#51896=CARTESIAN_POINT('Ctrl Pts',(-3.778673184137,0.03297598130245,-6.657410787988));
#51897=CARTESIAN_POINT('Ctrl Pts',(-3.488642527544,1.452181725154,-6.703452454654));
#51898=CARTESIAN_POINT('Ctrl Pts',(-2.685981185156,2.657999909866,-6.749494121321));
#51899=CARTESIAN_POINT('Ctrl Pts',(-1.488634412516,3.473244309537,-6.795535787988));
#51900=CARTESIAN_POINT('Ctrl Pts',(-0.0725436230386,3.778120679731,-6.841577454654));
#51901=CARTESIAN_POINT('Ctrl Pts',(1.354206925051,3.527829651783,-6.887619121321));
#51902=CARTESIAN_POINT('Ctrl Pts',(2.581966599408,2.7591496747,-6.933660787988));
#51903=CARTESIAN_POINT('Ctrl Pts',(3.430325031562,1.585032689158,-6.979702454654));
#51904=CARTESIAN_POINT('Ctrl Pts',(3.774622110468,0.1780066600445,-7.025744121321));
#51905=CARTESIAN_POINT('Ctrl Pts',(3.56426588058,-1.255176155123,-7.071785787988));
#51906=CARTESIAN_POINT('Ctrl Pts',(2.830166662326,-2.503919949063,-7.117827454654));
#51907=CARTESIAN_POINT('Ctrl Pts',(1.680195004987,-3.384730889313,-7.163869121321));
#51908=CARTESIAN_POINT('Ctrl Pts',(0.2833308928114,-3.768180204427,-7.209910787988));
#51909=CARTESIAN_POINT('Ctrl Pts',(-1.155166636586,-3.597922802058,-7.255952454654));
#51910=CARTESIAN_POINT('Ctrl Pts',(-2.423920817265,-2.898976771123,-7.301994121321));
#51911=CARTESIAN_POINT('Ctrl Pts',(-3.336497435721,-1.774047155286,-7.348035787988));
#51912=CARTESIAN_POINT('Ctrl Pts',(-3.758799984856,-0.3884341926996,-7.394077454654));
#51913=CARTESIAN_POINT('Ctrl Pts',(-3.6287741714,1.054256353961,-7.440119121321));
#51914=CARTESIAN_POINT('Ctrl Pts',(-2.965526345649,2.342031584525,-7.486160787988));
#51915=CARTESIAN_POINT('Ctrl Pts',(-1.866515954698,3.285662283295,-7.532202454654));
#51916=CARTESIAN_POINT('Ctrl Pts',(-0.4932346117968,3.746488760516,-7.578244121321));
#51917=CARTESIAN_POINT('Ctrl Pts',(0.9525240256962,3.656795952728,-7.624285787988));
#51918=CARTESIAN_POINT('Ctrl Pts',(2.258315987503,3.029763413827,-7.670327454654));
#51919=CARTESIAN_POINT('Ctrl Pts',(3.232265512507,1.957529592619,-7.716369121321));
#51920=CARTESIAN_POINT('Ctrl Pts',(3.731254486433,0.5976493334679,-7.762410787988));
#51921=CARTESIAN_POINT('Ctrl Pts',(3.681972434336,-0.8500448877034,-7.808452454654));
#51922=CARTESIAN_POINT('Ctrl Pts',(3.091614975073,-2.172854576276,-7.854494121321));
#51923=CARTESIAN_POINT('Ctrl Pts',(2.395273393235,-2.841812703939,-7.885188565765));
#51924=CARTESIAN_POINT('Ctrl Pts',(1.996883870199,-3.098557231525,-7.900535787988));
#51925=CARTESIAN_POINT('Ctrl Pts',(0.4830001770654,-3.823340089268,-5.050549754852));
#51926=CARTESIAN_POINT('Ctrl Pts',(-0.008576553896349,-3.885440672149,-5.065896977074));
#51927=CARTESIAN_POINT('Ctrl Pts',(-1.015768594638,-3.817642737768,-5.096591421519));
#51928=CARTESIAN_POINT('Ctrl Pts',(-2.377463978216,-3.154992073467,-5.142633088185));
#51929=CARTESIAN_POINT('Ctrl Pts',(-3.389763509381,-2.028732577009,-5.188674754852));
#51930=CARTESIAN_POINT('Ctrl Pts',(-3.903973908634,-0.604367076473,-5.234716421519));
#51931=CARTESIAN_POINT('Ctrl Pts',(-3.844520476228,0.908806183397,-5.280758088185));
#51932=CARTESIAN_POINT('Ctrl Pts',(-3.220143539338,2.288436865292,-5.326799754852));
#51933=CARTESIAN_POINT('Ctrl Pts',(-2.12258966234,3.331798397039,-5.372841421519));
#51934=CARTESIAN_POINT('Ctrl Pts',(-0.7131367100223,3.885576341192,-5.418883088185));
#51935=CARTESIAN_POINT('Ctrl Pts',(0.8011065197924,3.86839706016,-5.464924754852));
#51936=CARTESIAN_POINT('Ctrl Pts',(2.197632959513,3.282784921885,-5.510966421519));
#51937=CARTESIAN_POINT('Ctrl Pts',(3.27123319567,2.214791378231,-5.557008088185));
#51938=CARTESIAN_POINT('Ctrl Pts',(3.864149468261,0.8213503247539,-5.603049754852));
#51939=CARTESIAN_POINT('Ctrl Pts',(3.88925703704,-0.6927821944998,-5.649091421519));
#51940=CARTESIAN_POINT('Ctrl Pts',(3.342866526991,-2.105115401081,-5.695133088185));
#51941=CARTESIAN_POINT('Ctrl Pts',(2.305266055846,-3.208117186282,-5.741174754852));
#51942=CARTESIAN_POINT('Ctrl Pts',(0.9289234780445,-3.839709447483,-5.787216421519));
#51943=CARTESIAN_POINT('Ctrl Pts',(-0.5839176592511,-3.907084288362,-5.833258088185));
#51944=CARTESIAN_POINT('Ctrl Pts',(-2.01095633678,-3.400341465311,-5.879299754852));
#51945=CARTESIAN_POINT('Ctrl Pts',(-3.142499583669,-2.393943156341,-5.925341421519));
#51946=CARTESIAN_POINT('Ctrl Pts',(-3.812275336764,-1.035772284748,-5.971383088185));
#51947=CARTESIAN_POINT('Ctrl Pts',(-3.921864912888,0.474597802576,-6.017424754852));
#51948=CARTESIAN_POINT('Ctrl Pts',(-3.455164919641,1.915229189219,-6.063466421519));
#51949=CARTESIAN_POINT('Ctrl Pts',(-2.480753531974,3.07443155441,-6.109508088185));
#51950=CARTESIAN_POINT('Ctrl Pts',(-1.14181342738,3.781868528414,-6.155549754852));
#51951=CARTESIAN_POINT('Ctrl Pts',(0.3649078688106,3.933587385127,-6.201591421519));
#51952=CARTESIAN_POINT('Ctrl Pts',(1.818008603547,3.5072941403,-6.247633088185));
#51953=CARTESIAN_POINT('Ctrl Pts',(3.003966175905,2.565629490626,-6.293674754852));
#51954=CARTESIAN_POINT('Ctrl Pts',(3.748512732746,1.246964218249,-6.339716421519));
#51955=CARTESIAN_POINT('Ctrl Pts',(3.942242564249,-0.2549333908658,-6.385758088185));
#51956=CARTESIAN_POINT('Ctrl Pts',(3.55668847849,-1.719370389453,-6.431799754852));
#51957=CARTESIAN_POINT('Ctrl Pts',(2.648504848577,-2.931158394938,-6.477841421519));
#51958=CARTESIAN_POINT('Ctrl Pts',(1.351142663929,-3.712233959607,-6.523883088185));
#51959=CARTESIAN_POINT('Ctrl Pts',(-0.1447601235313,-3.947823701204,-6.569924754852));
#51960=CARTESIAN_POINT('Ctrl Pts',(-1.61939146205,-3.603309417992,-6.615966421519));
#51961=CARTESIAN_POINT('Ctrl Pts',(-2.856064984826,-2.729314982116,-6.662008088185));
#51962=CARTESIAN_POINT('Ctrl Pts',(-3.673060498094,-1.454267529204,-6.708049754852));
#51963=CARTESIAN_POINT('Ctrl Pts',(-3.95032644399,0.03447397660705,-6.754091421519));
#51964=CARTESIAN_POINT('Ctrl Pts',(-3.647120605201,1.518149781897,-6.800133088185));
#51965=CARTESIAN_POINT('Ctrl Pts',(-2.807996877932,2.778744501151,-6.846174754852));
#51966=CARTESIAN_POINT('Ctrl Pts',(-1.556258400404,3.631022894492,-6.892216421519));
#51967=CARTESIAN_POINT('Ctrl Pts',(-0.07583905208719,3.949748841044,-6.938258088185));
#51968=CARTESIAN_POINT('Ctrl Pts',(1.41572429421,3.688087877469,-6.984299754852));
#51969=CARTESIAN_POINT('Ctrl Pts',(2.699257236101,2.884489182249,-7.030341421519));
#51970=CARTESIAN_POINT('Ctrl Pts',(3.58615392846,1.657035748118,-7.076383088185));
#51971=CARTESIAN_POINT('Ctrl Pts',(3.946091342763,0.1860929437699,-7.122424754852));
#51972=CARTESIAN_POINT('Ctrl Pts',(3.726179289751,-1.312194867306,-7.168466421519));
#51973=CARTESIAN_POINT('Ctrl Pts',(2.958732248669,-2.617665171453,-7.214508088185));
#51974=CARTESIAN_POINT('Ctrl Pts',(1.7565209892,-3.53848858747,-7.260549754852));
#51975=CARTESIAN_POINT('Ctrl Pts',(0.2962017257726,-3.939356801154,-7.306591421519));
#51976=CARTESIAN_POINT('Ctrl Pts',(-1.207642230314,-3.761365139508,-7.352633088185));
#51977=CARTESIAN_POINT('Ctrl Pts',(-2.53403193025,-3.030668184684,-7.398674754852));
#51978=CARTESIAN_POINT('Ctrl Pts',(-3.488064039506,-1.854636548043,-7.444716421519));
#51979=CARTESIAN_POINT('Ctrl Pts',(-3.929550467657,-0.4060795386097,-7.490758088185));
#51980=CARTESIAN_POINT('Ctrl Pts',(-3.793617989703,1.102147910351,-7.536799754852));
#51981=CARTESIAN_POINT('Ctrl Pts',(-3.100240897452,2.448422726752,-7.582841421519));
#51982=CARTESIAN_POINT('Ctrl Pts',(-1.951305914712,3.434919605699,-7.628883088185));
#51983=CARTESIAN_POINT('Ctrl Pts',(-0.5156407117324,3.916679983045,-7.674924754852));
#51984=CARTESIAN_POINT('Ctrl Pts',(0.9957942017955,3.822912712584,-7.720966421519));
#51985=CARTESIAN_POINT('Ctrl Pts',(2.360904192978,3.167396053969,-7.767008088185));
#51986=CARTESIAN_POINT('Ctrl Pts',(3.37909718725,2.046454016473,-7.813049754852));
#51987=CARTESIAN_POINT('Ctrl Pts',(3.900753663718,0.6247986664056,-7.859091421519));
#51988=CARTESIAN_POINT('Ctrl Pts',(3.849232882712,-0.8886597582905,-7.905133088185));
#51989=CARTESIAN_POINT('Ctrl Pts',(3.232057337464,-2.271560538139,-7.951174754852));
#51990=CARTESIAN_POINT('Ctrl Pts',(2.504083143683,-2.97090733339,-7.981869199296));
#51991=CARTESIAN_POINT('Ctrl Pts',(2.087596035333,-3.239314958832,-7.997216421519));
#51992=CARTESIAN_POINT('Ctrl Pts',(0.5039879501212,-3.989475419894,-5.147230388383));
#51993=CARTESIAN_POINT('Ctrl Pts',(-0.0089492302955,-4.054274455078,-5.162577610605));
#51994=CARTESIAN_POINT('Ctrl Pts',(-1.059906716638,-3.983530501776,-5.19327205505));
#51995=CARTESIAN_POINT('Ctrl Pts',(-2.480771754885,-3.292085724309,-5.239313721716));
#51996=CARTESIAN_POINT('Ctrl Pts',(-3.537058667077,-2.116886952389,-5.285355388383));
#51997=CARTESIAN_POINT('Ctrl Pts',(-4.073613014997,-0.6306285969564,-5.33139705505));
#51998=CARTESIAN_POINT('Ctrl Pts',(-4.011576156733,0.9482964751911,-5.377438721716));
#51999=CARTESIAN_POINT('Ctrl Pts',(-3.360068212288,2.387876153023,-5.423480388383));
#52000=CARTESIAN_POINT('Ctrl Pts',(-2.214822403112,3.476574800745,-5.46952205505));
#52001=CARTESIAN_POINT('Ctrl Pts',(-0.7441245898171,4.054416019338,-5.515563721716));
#52002=CARTESIAN_POINT('Ctrl Pts',(0.8359169456045,4.036490248204,-5.561605388383));
#52003=CARTESIAN_POINT('Ctrl Pts',(2.29312655145,3.425431546469,-5.60764705505));
#52004=CARTESIAN_POINT('Ctrl Pts',(3.413377863899,2.311030553742,-5.653688721716));
#52005=CARTESIAN_POINT('Ctrl Pts',(4.03205808599,0.8570404032131,-5.699730388383));
#52006=CARTESIAN_POINT('Ctrl Pts',(4.058256652206,-0.7228856109492,-5.74577205505));
#52007=CARTESIAN_POINT('Ctrl Pts',(3.488123873377,-2.196588833996,-5.791813721716));
#52008=CARTESIAN_POINT('Ctrl Pts',(2.405436621222,-3.347519278951,-5.837855388383));
#52009=CARTESIAN_POINT('Ctrl Pts',(0.9692879252418,-4.006556074691,-5.88389705505));
#52010=CARTESIAN_POINT('Ctrl Pts',(-0.6092905926321,-4.076858549839,-5.929938721716));
#52011=CARTESIAN_POINT('Ctrl Pts',(-2.098338282431,-3.548096266189,-5.975980388383));
#52012=CARTESIAN_POINT('Ctrl Pts',(-3.279050399221,-2.497967001589,-6.02202205505));
#52013=CARTESIAN_POINT('Ctrl Pts',(-3.97792987147,-1.080779625702,-6.068063721716));
#52014=CARTESIAN_POINT('Ctrl Pts',(-4.092281435813,0.4952204678384,-6.114105388383));
#52015=CARTESIAN_POINT('Ctrl Pts',(-3.605301960262,1.998451509793,-6.16014705505));
#52016=CARTESIAN_POINT('Ctrl Pts',(-2.588549542429,3.208024614627,-6.206188721716));
#52017=CARTESIAN_POINT('Ctrl Pts',(-1.19142856672,3.946201798194,-6.252230388383));
#52018=CARTESIAN_POINT('Ctrl Pts',(0.3807641850203,4.104513283822,-6.29827205505));
#52019=CARTESIAN_POINT('Ctrl Pts',(1.897006404783,3.659696348315,-6.344313721716));
#52020=CARTESIAN_POINT('Ctrl Pts',(3.134497308938,2.677113610201,-6.390355388383));
#52021=CARTESIAN_POINT('Ctrl Pts',(3.91139659546,1.30114846758,-6.43639705505));
#52022=CARTESIAN_POINT('Ctrl Pts',(4.113544555839,-0.2660109937444,-6.482438721716));
#52023=CARTESIAN_POINT('Ctrl Pts',(3.711237015243,-1.794082071242,-6.528480388383));
#52024=CARTESIAN_POINT('Ctrl Pts',(2.763590145309,-3.058525816535,-6.57452205505));
#52025=CARTESIAN_POINT('Ctrl Pts',(1.409853772006,-3.873541403319,-6.620563721716));
#52026=CARTESIAN_POINT('Ctrl Pts',(-0.1510503750974,-4.119368209549,-6.666605388383));
#52027=CARTESIAN_POINT('Ctrl Pts',(-1.689758766469,-3.759883771183,-6.71264705505));
#52028=CARTESIAN_POINT('Ctrl Pts',(-2.980169377703,-2.847911715953,-6.758688721716));
#52029=CARTESIAN_POINT('Ctrl Pts',(-3.83266574011,-1.517459714869,-6.804730388383));
#52030=CARTESIAN_POINT('Ctrl Pts',(-4.121979703844,0.03597197191164,-6.85077205505));
#52031=CARTESIAN_POINT('Ctrl Pts',(-3.805598682858,1.584117838639,-6.896813721716));
#52032=CARTESIAN_POINT('Ctrl Pts',(-2.930012570708,2.899489092436,-6.942855388383));
#52033=CARTESIAN_POINT('Ctrl Pts',(-1.623882388293,3.788801479446,-6.98889705505));
#52034=CARTESIAN_POINT('Ctrl Pts',(-0.07913448113579,4.121377002357,-7.034938721716));
#52035=CARTESIAN_POINT('Ctrl Pts',(1.47724166337,3.848346103155,-7.080980388383));
#52036=CARTESIAN_POINT('Ctrl Pts',(2.816547872794,3.009828689797,-7.12702205505));
#52037=CARTESIAN_POINT('Ctrl Pts',(3.741982825359,1.729038807078,-7.173063721716));
#52038=CARTESIAN_POINT('Ctrl Pts',(4.117560575058,0.1941792274952,-7.219105388383));
#52039=CARTESIAN_POINT('Ctrl Pts',(3.888092698922,-1.369213579488,-7.26514705505));
#52040=CARTESIAN_POINT('Ctrl Pts',(3.087297835011,-2.731410393844,-7.311188721716));
#52041=CARTESIAN_POINT('Ctrl Pts',(1.832846973412,-3.692246285626,-7.357230388383));
#52042=CARTESIAN_POINT('Ctrl Pts',(0.3090725587339,-4.110533397882,-7.40327205505));
#52043=CARTESIAN_POINT('Ctrl Pts',(-1.260117824043,-3.924807476958,-7.449313721716));
#52044=CARTESIAN_POINT('Ctrl Pts',(-2.644143043235,-3.162359598245,-7.495355388383));
#52045=CARTESIAN_POINT('Ctrl Pts',(-3.639630643292,-1.935225940801,-7.54139705505));
#52046=CARTESIAN_POINT('Ctrl Pts',(-4.100300950458,-0.4237248845199,-7.587438721716));
#52047=CARTESIAN_POINT('Ctrl Pts',(-3.958461808006,1.150039466741,-7.633480388383));
#52048=CARTESIAN_POINT('Ctrl Pts',(-3.234955449255,2.554813868979,-7.67952205505));
#52049=CARTESIAN_POINT('Ctrl Pts',(-2.036095874727,3.584176928104,-7.725563721716));
#52050=CARTESIAN_POINT('Ctrl Pts',(-0.5380468116679,4.086871205575,-7.771605388383));
#52051=CARTESIAN_POINT('Ctrl Pts',(1.039064377895,3.98902947244,-7.81764705505));
#52052=CARTESIAN_POINT('Ctrl Pts',(2.463492398452,3.305028694111,-7.863688721716));
#52053=CARTESIAN_POINT('Ctrl Pts',(3.525928861993,2.135378440328,-7.909730388383));
#52054=CARTESIAN_POINT('Ctrl Pts',(4.070252841003,0.6519479993433,-7.95577205505));
#52055=CARTESIAN_POINT('Ctrl Pts',(4.016493331088,-0.9272746288775,-8.001813721716));
#52056=CARTESIAN_POINT('Ctrl Pts',(3.372499699855,-2.370266500001,-8.047855388383));
#52057=CARTESIAN_POINT('Ctrl Pts',(2.612892894131,-3.100001962842,-8.078549832827));
#52058=CARTESIAN_POINT('Ctrl Pts',(2.178308200468,-3.380072686139,-8.09389705505));
#52059=CARTESIAN_POINT('Origin',(0.,5.773502691896,-10.5));
#52060=CARTESIAN_POINT('',(4.5,3.175426480543,-11.73961639634));
#52061=CARTESIAN_POINT('Origin',(4.,2.309401076759,-28.10392));
#52062=CARTESIAN_POINT('',(5.,2.309401076759,-11.73961639634));
#52063=CARTESIAN_POINT('Origin',(5.,2.886751345948,-10.5));
#52064=CARTESIAN_POINT('',(5.,-2.309401076759,-11.73961639634));
#52065=CARTESIAN_POINT('Origin',(4.,-2.309401076759,-28.10392));
#52066=CARTESIAN_POINT('',(4.5,-3.175426480543,-11.73961639634));
#52067=CARTESIAN_POINT('Origin',(5.,-2.886751345948,-10.5));
#52068=CARTESIAN_POINT('',(0.5,-5.484827557301,-11.73961639634));
#52069=CARTESIAN_POINT('Origin',(0.,-4.618802153517,-28.10392));
#52070=CARTESIAN_POINT('',(-0.5,-5.484827557301,-11.73961639634));
#52071=CARTESIAN_POINT('Origin',(-5.,2.886751345948,-10.5));
#52072=CARTESIAN_POINT('',(-4.5,3.175426480543,-11.73961639634));
#52073=CARTESIAN_POINT('Origin',(-4.,2.309401076759,-28.10392));
#52074=CARTESIAN_POINT('',(-5.,2.309401076758,-11.73961639634));
#52075=CARTESIAN_POINT('Origin',(-5.,-2.886751345948,-10.5));
#52076=CARTESIAN_POINT('',(-5.,-2.309401076759,-11.73961639634));
#52077=CARTESIAN_POINT('Origin',(-4.,-2.309401076759,-28.10392));
#52078=CARTESIAN_POINT('',(-4.5,-3.175426480543,-11.73961639634));
#52079=CARTESIAN_POINT('Origin',(0.,-5.773502691896,-10.5));
#52080=CARTESIAN_POINT('',(0.,0.,0.));
#52081=CARTESIAN_POINT('Origin',(0.,0.,-0.75));
#52082=CARTESIAN_POINT('',(-2.6,3.18408167778312E-16,-0.75));
#52083=CARTESIAN_POINT('Origin',(-3.35,4.10256677714363E-16,-0.75));
#52084=CARTESIAN_POINT('Origin',(0.,0.,-0.75));
#52085=CARTESIAN_POINT('',(0.,0.,0.));
#52086=CARTESIAN_POINT('Origin',(0.,0.,0.));
#52087=CARTESIAN_POINT('',(-3.8,0.,4.65365783675994E-16));
#52088=CARTESIAN_POINT('Origin',(0.,0.,0.));
#52089=CARTESIAN_POINT('',(-2.5,0.,3.06161699786838E-16));
#52090=CARTESIAN_POINT('Origin',(0.,0.,0.));
#52091=CARTESIAN_POINT('Origin',(0.,0.,0.));
#52092=CARTESIAN_POINT('',(-2.5,2.,3.06161699786838E-16));
#52093=CARTESIAN_POINT('',(-2.5,0.,3.06161699786838E-16));
#52094=CARTESIAN_POINT('Origin',(0.,2.,0.));
#52095=CARTESIAN_POINT('Origin',(0.,2.,0.));
#52096=CARTESIAN_POINT('',(-3.8,2.,4.65365783675994E-16));
#52097=CARTESIAN_POINT('Origin',(0.,2.,0.));
#52098=CARTESIAN_POINT('Origin',(0.,0.,0.));
#52099=CARTESIAN_POINT('',(-3.8,0.,4.65365783675994E-16));
#52100=CARTESIAN_POINT('',(0.,0.,0.));
#52101=CARTESIAN_POINT('Origin',(0.,0.,0.));
#52102=CARTESIAN_POINT('',(8.1439012143299E-16,-6.65,0.));
#52103=CARTESIAN_POINT('Origin',(0.,0.,0.));
#52104=CARTESIAN_POINT('',(0.,5.65,0.));
#52105=CARTESIAN_POINT('Origin',(0.,0.,0.));
#52106=CARTESIAN_POINT('Origin',(0.,0.,-1.51640802568));
#52107=CARTESIAN_POINT('',(8.1439012143299E-16,-6.65,-1.));
#52108=CARTESIAN_POINT('',(8.1439012143299E-16,-6.65,-1.51640802568));
#52109=CARTESIAN_POINT('Origin',(0.,0.,-1.));
#52110=CARTESIAN_POINT('Origin',(0.,0.,48.5558018803));
#52111=CARTESIAN_POINT('',(3.74939945665464E-31,-3.06161699786838E-15,-1.4441981197));
#52112=CARTESIAN_POINT('Origin',(0.,0.,48.5558018803));
#52113=CARTESIAN_POINT('Origin',(0.,0.,0.));
#52114=CARTESIAN_POINT('',(0.,5.65,-0.6206914879705));
#52115=CARTESIAN_POINT('',(6.91925441518255E-16,-5.65,-0.620691487970504));
#52116=CARTESIAN_POINT('Origin',(0.,0.,-0.6206914879705));
#52117=CARTESIAN_POINT('',(-6.91925441518255E-16,5.65,0.));
#52118=CARTESIAN_POINT('Origin',(0.,0.,-0.6206914879705));
#52119=CARTESIAN_POINT('Origin',(0.,0.,48.5558018803));
#52120=CARTESIAN_POINT('',(3.7119054620881E-31,-3.0310008278897E-15,-0.944198119699999));
#52121=CARTESIAN_POINT('Origin',(0.,0.,48.5558018803));
#52122=CARTESIAN_POINT('',(0.,8.91,5.88));
#52123=CARTESIAN_POINT('',(-2.9,1.41,0.));
#52124=CARTESIAN_POINT('',(-30.7,1.41,0.));
#52125=CARTESIAN_POINT('',(1.5,1.41,0.));
#52126=CARTESIAN_POINT('',(-5.6,1.41,0.));
#52127=CARTESIAN_POINT('',(-3.8,8.91,-20.6));
#52128=CARTESIAN_POINT('',(0.,8.91,-21.9));
#52129=CARTESIAN_POINT('',(0.,0.,0.));
#52130=CARTESIAN_POINT('',(-14.6,1.41,0.));
#52131=CARTESIAN_POINT('',(-5.7,1.41,0.));
#52132=CARTESIAN_POINT('',(0.,8.91,-16.1));
#52133=CARTESIAN_POINT('',(0.,8.91,-19.6));
#52134=CARTESIAN_POINT('',(4.25,1.41,0.));
#52135=UNCERTAINTY_MEASURE_WITH_UNIT(LENGTH_MEASURE(0.01),#52165,
'DISTANCE_ACCURACY_VALUE',
'Maximum model space distance between geometric entities at asserted c
onnectivities');
#52136=UNCERTAINTY_MEASURE_WITH_UNIT(LENGTH_MEASURE(0.01),#52165,
'DISTANCE_ACCURACY_VALUE',
'Maximum model space distance between geometric entities at asserted c
onnectivities');
#52137=UNCERTAINTY_MEASURE_WITH_UNIT(LENGTH_MEASURE(0.01),#52165,
'DISTANCE_ACCURACY_VALUE',
'Maximum model space distance between geometric entities at asserted c
onnectivities');
#52138=UNCERTAINTY_MEASURE_WITH_UNIT(LENGTH_MEASURE(0.01),#52165,
'DISTANCE_ACCURACY_VALUE',
'Maximum model space distance between geometric entities at asserted c
onnectivities');
#52139=UNCERTAINTY_MEASURE_WITH_UNIT(LENGTH_MEASURE(0.01),#52165,
'DISTANCE_ACCURACY_VALUE',
'Maximum model space distance between geometric entities at asserted c
onnectivities');
#52140=UNCERTAINTY_MEASURE_WITH_UNIT(LENGTH_MEASURE(0.01),#52165,
'DISTANCE_ACCURACY_VALUE',
'Maximum model space distance between geometric entities at asserted c
onnectivities');
#52141=UNCERTAINTY_MEASURE_WITH_UNIT(LENGTH_MEASURE(0.01),#52165,
'DISTANCE_ACCURACY_VALUE',
'Maximum model space distance between geometric entities at asserted c
onnectivities');
#52142=UNCERTAINTY_MEASURE_WITH_UNIT(LENGTH_MEASURE(0.01),#52165,
'DISTANCE_ACCURACY_VALUE',
'Maximum model space distance between geometric entities at asserted c
onnectivities');
#52143=UNCERTAINTY_MEASURE_WITH_UNIT(LENGTH_MEASURE(0.01),#52165,
'DISTANCE_ACCURACY_VALUE',
'Maximum model space distance between geometric entities at asserted c
onnectivities');
#52144=UNCERTAINTY_MEASURE_WITH_UNIT(LENGTH_MEASURE(0.01),#52165,
'DISTANCE_ACCURACY_VALUE',
'Maximum model space distance between geometric entities at asserted c
onnectivities');
#52145=UNCERTAINTY_MEASURE_WITH_UNIT(LENGTH_MEASURE(0.01),#52165,
'DISTANCE_ACCURACY_VALUE',
'Maximum model space distance between geometric entities at asserted c
onnectivities');
#52146=UNCERTAINTY_MEASURE_WITH_UNIT(LENGTH_MEASURE(0.01),#52165,
'DISTANCE_ACCURACY_VALUE',
'Maximum model space distance between geometric entities at asserted c
onnectivities');
#52147=UNCERTAINTY_MEASURE_WITH_UNIT(LENGTH_MEASURE(0.01),#52165,
'DISTANCE_ACCURACY_VALUE',
'Maximum model space distance between geometric entities at asserted c
onnectivities');
#52148=UNCERTAINTY_MEASURE_WITH_UNIT(LENGTH_MEASURE(0.01),#52165,
'DISTANCE_ACCURACY_VALUE',
'Maximum model space distance between geometric entities at asserted c
onnectivities');
#52149=UNCERTAINTY_MEASURE_WITH_UNIT(LENGTH_MEASURE(0.01),#52165,
'DISTANCE_ACCURACY_VALUE',
'Maximum model space distance between geometric entities at asserted c
onnectivities');
#52150=(
GEOMETRIC_REPRESENTATION_CONTEXT(3)
GLOBAL_UNCERTAINTY_ASSIGNED_CONTEXT((#52135))
GLOBAL_UNIT_ASSIGNED_CONTEXT((#52165,#52167,#52168))
REPRESENTATION_CONTEXT('','3D')
);
#52151=(
GEOMETRIC_REPRESENTATION_CONTEXT(3)
GLOBAL_UNCERTAINTY_ASSIGNED_CONTEXT((#52136))
GLOBAL_UNIT_ASSIGNED_CONTEXT((#52165,#52167,#52168))
REPRESENTATION_CONTEXT('','3D')
);
#52152=(
GEOMETRIC_REPRESENTATION_CONTEXT(3)
GLOBAL_UNCERTAINTY_ASSIGNED_CONTEXT((#52137))
GLOBAL_UNIT_ASSIGNED_CONTEXT((#52165,#52167,#52168))
REPRESENTATION_CONTEXT('','3D')
);
#52153=(
GEOMETRIC_REPRESENTATION_CONTEXT(3)
GLOBAL_UNCERTAINTY_ASSIGNED_CONTEXT((#52138))
GLOBAL_UNIT_ASSIGNED_CONTEXT((#52165,#52167,#52168))
REPRESENTATION_CONTEXT('','3D')
);
#52154=(
GEOMETRIC_REPRESENTATION_CONTEXT(3)
GLOBAL_UNCERTAINTY_ASSIGNED_CONTEXT((#52139))
GLOBAL_UNIT_ASSIGNED_CONTEXT((#52165,#52167,#52168))
REPRESENTATION_CONTEXT('','3D')
);
#52155=(
GEOMETRIC_REPRESENTATION_CONTEXT(3)
GLOBAL_UNCERTAINTY_ASSIGNED_CONTEXT((#52140))
GLOBAL_UNIT_ASSIGNED_CONTEXT((#52165,#52167,#52168))
REPRESENTATION_CONTEXT('','3D')
);
#52156=(
GEOMETRIC_REPRESENTATION_CONTEXT(3)
GLOBAL_UNCERTAINTY_ASSIGNED_CONTEXT((#52141))
GLOBAL_UNIT_ASSIGNED_CONTEXT((#52165,#52167,#52168))
REPRESENTATION_CONTEXT('','3D')
);
#52157=(
GEOMETRIC_REPRESENTATION_CONTEXT(3)
GLOBAL_UNCERTAINTY_ASSIGNED_CONTEXT((#52142))
GLOBAL_UNIT_ASSIGNED_CONTEXT((#52165,#52167,#52168))
REPRESENTATION_CONTEXT('','3D')
);
#52158=(
GEOMETRIC_REPRESENTATION_CONTEXT(3)
GLOBAL_UNCERTAINTY_ASSIGNED_CONTEXT((#52143))
GLOBAL_UNIT_ASSIGNED_CONTEXT((#52165,#52167,#52168))
REPRESENTATION_CONTEXT('','3D')
);
#52159=(
GEOMETRIC_REPRESENTATION_CONTEXT(3)
GLOBAL_UNCERTAINTY_ASSIGNED_CONTEXT((#52144))
GLOBAL_UNIT_ASSIGNED_CONTEXT((#52165,#52167,#52168))
REPRESENTATION_CONTEXT('','3D')
);
#52160=(
GEOMETRIC_REPRESENTATION_CONTEXT(3)
GLOBAL_UNCERTAINTY_ASSIGNED_CONTEXT((#52145))
GLOBAL_UNIT_ASSIGNED_CONTEXT((#52165,#52167,#52168))
REPRESENTATION_CONTEXT('','3D')
);
#52161=(
GEOMETRIC_REPRESENTATION_CONTEXT(3)
GLOBAL_UNCERTAINTY_ASSIGNED_CONTEXT((#52146))
GLOBAL_UNIT_ASSIGNED_CONTEXT((#52165,#52167,#52168))
REPRESENTATION_CONTEXT('','3D')
);
#52162=(
GEOMETRIC_REPRESENTATION_CONTEXT(3)
GLOBAL_UNCERTAINTY_ASSIGNED_CONTEXT((#52147))
GLOBAL_UNIT_ASSIGNED_CONTEXT((#52165,#52167,#52168))
REPRESENTATION_CONTEXT('','3D')
);
#52163=(
GEOMETRIC_REPRESENTATION_CONTEXT(3)
GLOBAL_UNCERTAINTY_ASSIGNED_CONTEXT((#52148))
GLOBAL_UNIT_ASSIGNED_CONTEXT((#52165,#52167,#52168))
REPRESENTATION_CONTEXT('','3D')
);
#52164=(
GEOMETRIC_REPRESENTATION_CONTEXT(3)
GLOBAL_UNCERTAINTY_ASSIGNED_CONTEXT((#52149))
GLOBAL_UNIT_ASSIGNED_CONTEXT((#52165,#52167,#52168))
REPRESENTATION_CONTEXT('','3D')
);
#52165=(
LENGTH_UNIT()
NAMED_UNIT(*)
SI_UNIT(.MILLI.,.METRE.)
);
#52166=(
LENGTH_UNIT()
NAMED_UNIT(*)
SI_UNIT($,.METRE.)
);
#52167=(
NAMED_UNIT(*)
PLANE_ANGLE_UNIT()
SI_UNIT($,.RADIAN.)
);
#52168=(
NAMED_UNIT(*)
SI_UNIT($,.STERADIAN.)
SOLID_ANGLE_UNIT()
);
#52169=SHAPE_DEFINITION_REPRESENTATION(#52183,#52210);
#52170=SHAPE_DEFINITION_REPRESENTATION(#52184,#52211);
#52171=SHAPE_DEFINITION_REPRESENTATION(#52185,#52212);
#52172=SHAPE_DEFINITION_REPRESENTATION(#52186,#52213);
#52173=SHAPE_DEFINITION_REPRESENTATION(#52187,#52214);
#52174=SHAPE_DEFINITION_REPRESENTATION(#52188,#52215);
#52175=SHAPE_DEFINITION_REPRESENTATION(#52189,#52216);
#52176=SHAPE_DEFINITION_REPRESENTATION(#52190,#52217);
#52177=SHAPE_DEFINITION_REPRESENTATION(#52191,#52218);
#52178=SHAPE_DEFINITION_REPRESENTATION(#52192,#52219);
#52179=SHAPE_DEFINITION_REPRESENTATION(#52193,#52220);
#52180=SHAPE_DEFINITION_REPRESENTATION(#52194,#52221);
#52181=SHAPE_DEFINITION_REPRESENTATION(#52195,#52222);
#52182=SHAPE_DEFINITION_REPRESENTATION(#52196,#52223);
#52183=PRODUCT_DEFINITION_SHAPE('',$,#52225);
#52184=PRODUCT_DEFINITION_SHAPE('',$,#52226);
#52185=PRODUCT_DEFINITION_SHAPE('',$,#52227);
#52186=PRODUCT_DEFINITION_SHAPE('',$,#52228);
#52187=PRODUCT_DEFINITION_SHAPE('',$,#52229);
#52188=PRODUCT_DEFINITION_SHAPE('',$,#52230);
#52189=PRODUCT_DEFINITION_SHAPE('',$,#52231);
#52190=PRODUCT_DEFINITION_SHAPE('',$,#52232);
#52191=PRODUCT_DEFINITION_SHAPE('',$,#52233);
#52192=PRODUCT_DEFINITION_SHAPE('',$,#52234);
#52193=PRODUCT_DEFINITION_SHAPE('',$,#52235);
#52194=PRODUCT_DEFINITION_SHAPE('',$,#52236);
#52195=PRODUCT_DEFINITION_SHAPE('',$,#52237);
#52196=PRODUCT_DEFINITION_SHAPE('',$,#52238);
#52197=PRODUCT_DEFINITION_SHAPE($,$,#50);
#52198=PRODUCT_DEFINITION_SHAPE($,$,#51);
#52199=PRODUCT_DEFINITION_SHAPE($,$,#52);
#52200=PRODUCT_DEFINITION_SHAPE($,$,#53);
#52201=PRODUCT_DEFINITION_SHAPE($,$,#54);
#52202=PRODUCT_DEFINITION_SHAPE($,$,#55);
#52203=PRODUCT_DEFINITION_SHAPE($,$,#56);
#52204=PRODUCT_DEFINITION_SHAPE($,$,#57);
#52205=PRODUCT_DEFINITION_SHAPE($,$,#58);
#52206=PRODUCT_DEFINITION_SHAPE($,$,#59);
#52207=PRODUCT_DEFINITION_SHAPE($,$,#60);
#52208=PRODUCT_DEFINITION_SHAPE($,$,#61);
#52209=PRODUCT_DEFINITION_SHAPE($,$,#62);
#52210=SHAPE_REPRESENTATION('',(#9275,#10197,#10198,#10199,#10200,#10201,
#10202,#10203,#10204,#10205,#10206,#10207,#10208,#10209),#52150);
#52211=SHAPE_REPRESENTATION('',(#9276),#52151);
#52212=SHAPE_REPRESENTATION('',(#9302),#52152);
#52213=SHAPE_REPRESENTATION('',(#9667),#52153);
#52214=SHAPE_REPRESENTATION('',(#9694),#52154);
#52215=SHAPE_REPRESENTATION('',(#9704),#52155);
#52216=SHAPE_REPRESENTATION('',(#9776),#52156);
#52217=SHAPE_REPRESENTATION('',(#9921),#52157);
#52218=SHAPE_REPRESENTATION('',(#9987),#52158);
#52219=SHAPE_REPRESENTATION('',(#10132),#52159);
#52220=SHAPE_REPRESENTATION('',(#10142),#52160);
#52221=SHAPE_REPRESENTATION('',(#10171),#52161);
#52222=SHAPE_REPRESENTATION('',(#10175),#52162);
#52223=SHAPE_REPRESENTATION('',(#10184),#52163);
#52224=PRODUCT_DEFINITION_CONTEXT('part definition',#52268,'design');
#52225=PRODUCT_DEFINITION('MONTAGEM_ASM','MAT-061',#52239,
#52224);
#52226=PRODUCT_DEFINITION('Worm Shaft / Tuning Worm',
'Worm Shaft / Tuning Worm',#52240,#52224);
#52227=PRODUCT_DEFINITION('Worm Gear / Tuning Gear',
'Worm Gear / Tuning Gear',#52241,#52224);
#52228=PRODUCT_DEFINITION('String Post / Peg Shaft',
'String Post / Peg Shaft',#52242,#52224);
#52229=PRODUCT_DEFINITION('Flat Washer M3','Flat Washer M3',#52243,#52224);
#52230=PRODUCT_DEFINITION('Screw M3','Screw M3',#52244,#52224);
#52231=PRODUCT_DEFINITION('Tuning Key / Button','Tuning Key / Button',#52245,
#52224);
#52232=PRODUCT_DEFINITION('Countersunk Screw 2.5x12',
'Countersunk Screw 2.5x12',#52246,#52224);
#52233=PRODUCT_DEFINITION('Housing / Gear Box Body',
'Housing / Gear Box Body',#52247,#52224);
#52234=PRODUCT_DEFINITION('Flat Washer M8','Flat Washer M8',#52248,#52224);
#52235=PRODUCT_DEFINITION('Bushing / Bearing Sleeve',
'Bushing / Bearing Sleeve',#52249,#52224);
#52236=PRODUCT_DEFINITION('O-Ring / Sealing Ring',
'O-Ring / Sealing Ring',#52250,#52224);
#52237=PRODUCT_DEFINITION('Retaining Ring / Washer',
'Retaining Ring / Washer',#52251,#52224);
#52238=PRODUCT_DEFINITION('Cover Plate / Back Cover',
'Cover Plate / Back Cover',#52252,#52224);
#52239=PRODUCT_DEFINITION_FORMATION('',$,#52270);
#52240=PRODUCT_DEFINITION_FORMATION('',$,#52271);
#52241=PRODUCT_DEFINITION_FORMATION('',$,#52272);
#52242=PRODUCT_DEFINITION_FORMATION('',$,#52273);
#52243=PRODUCT_DEFINITION_FORMATION('',$,#52274);
#52244=PRODUCT_DEFINITION_FORMATION('',$,#52275);
#52245=PRODUCT_DEFINITION_FORMATION('',$,#52276);
#52246=PRODUCT_DEFINITION_FORMATION('',$,#52277);
#52247=PRODUCT_DEFINITION_FORMATION('',$,#52278);
#52248=PRODUCT_DEFINITION_FORMATION('',$,#52279);
#52249=PRODUCT_DEFINITION_FORMATION('',$,#52280);
#52250=PRODUCT_DEFINITION_FORMATION('',$,#52281);
#52251=PRODUCT_DEFINITION_FORMATION('',$,#52282);
#52252=PRODUCT_DEFINITION_FORMATION('',$,#52283);
#52253=PRODUCT_RELATED_PRODUCT_CATEGORY('MAT-061',
'MAT-061',(#52270));
#52254=PRODUCT_RELATED_PRODUCT_CATEGORY('Worm Shaft / Tuning Worm',
'Worm Shaft / Tuning Worm',(#52271));
#52255=PRODUCT_RELATED_PRODUCT_CATEGORY('Worm Gear / Tuning Gear',
'Worm Gear / Tuning Gear',(#52272));
#52256=PRODUCT_RELATED_PRODUCT_CATEGORY('String Post / Peg Shaft',
'String Post / Peg Shaft',(#52273));
#52257=PRODUCT_RELATED_PRODUCT_CATEGORY('Flat Washer M3',
'Flat Washer M3',(#52274));
#52258=PRODUCT_RELATED_PRODUCT_CATEGORY('Screw M3','Screw M3',(#52275));
#52259=PRODUCT_RELATED_PRODUCT_CATEGORY('Tuning Key / Button',
'Tuning Key / Button',(#52276));
#52260=PRODUCT_RELATED_PRODUCT_CATEGORY('Countersunk Screw 2.5x12',
'Countersunk Screw 2.5x12',(#52277));
#52261=PRODUCT_RELATED_PRODUCT_CATEGORY('Housing / Gear Box Body',
'Housing / Gear Box Body',(#52278));
#52262=PRODUCT_RELATED_PRODUCT_CATEGORY('Flat Washer M8',
'Flat Washer M8',(#52279));
#52263=PRODUCT_RELATED_PRODUCT_CATEGORY('Bushing / Bearing Sleeve',
'Bushing / Bearing Sleeve',(#52280));
#52264=PRODUCT_RELATED_PRODUCT_CATEGORY('O-Ring / Sealing Ring',
'O-Ring / Sealing Ring',(#52281));
#52265=PRODUCT_RELATED_PRODUCT_CATEGORY('Retaining Ring / Washer',
'Retaining Ring / Washer',(#52282));
#52266=PRODUCT_RELATED_PRODUCT_CATEGORY('Cover Plate / Back Cover',
'Cover Plate / Back Cover',(#52283));
#52267=APPLICATION_PROTOCOL_DEFINITION('international standard',
'ap242_managed_model_based_3d_engineering',2011,#52268);
#52268=APPLICATION_CONTEXT('Managed model based 3d engineering');
#52269=PRODUCT_CONTEXT('part definition',#52268,'mechanical');
#52270=PRODUCT('MONTAGEM_ASM','MAT-061',$,(#52269));
#52271=PRODUCT('Worm Shaft / Tuning Worm','Worm Shaft / Tuning Worm',
'NOT SPECIFIED',(#52269));
#52272=PRODUCT('Worm Gear / Tuning Gear','Worm Gear / Tuning Gear',
'NOT SPECIFIED',(#52269));
#52273=PRODUCT('String Post / Peg Shaft','String Post / Peg Shaft',
'NOT SPECIFIED',(#52269));
#52274=PRODUCT('Flat Washer M3','Flat Washer M3','NOT SPECIFIED',(#52269));
#52275=PRODUCT('Screw M3','Screw M3','NOT SPECIFIED',(#52269));
#52276=PRODUCT('Tuning Key / Button','Tuning Key / Button',
'NOT SPECIFIED',(#52269));
#52277=PRODUCT('Countersunk Screw 2.5x12','Countersunk Screw 2.5x12',
'NOT SPECIFIED',(#52269));
#52278=PRODUCT('Housing / Gear Box Body','Housing / Gear Box Body',
'NOT SPECIFIED',(#52269));
#52279=PRODUCT('Flat Washer M8','Flat Washer M8','NOT SPECIFIED',(#52269));
#52280=PRODUCT('Bushing / Bearing Sleeve','Bushing / Bearing Sleeve',
'NOT SPECIFIED',(#52269));
#52281=PRODUCT('O-Ring / Sealing Ring','O-Ring / Sealing Ring',
'NOT SPECIFIED',(#52269));
#52282=PRODUCT('Retaining Ring / Washer','Retaining Ring / Washer',
'NOT SPECIFIED',(#52269));
#52283=PRODUCT('Cover Plate / Back Cover','Cover Plate / Back Cover',
'NOT SPECIFIED',(#52269));
#52284=PRESENTATION_STYLE_ASSIGNMENT((#52285));
#52285=SURFACE_STYLE_USAGE(.BOTH.,#52286);
#52286=SURFACE_SIDE_STYLE('',(#52287));
#52287=SURFACE_STYLE_FILL_AREA(#52288);
#52288=FILL_AREA_STYLE('Steel - Satin',(#52289));
#52289=FILL_AREA_STYLE_COLOUR('Steel - Satin',#52290);
#52290=COLOUR_RGB('Steel - Satin',0.627450980392157,0.627450980392157,0.627450980392157);
#52291=COLOUR_RGB('Dark Blue',0.08,0.2,0.34);
#52292=FILL_AREA_STYLE_COLOUR('',#52291);
#52293=FILL_AREA_STYLE('',(#52292));
#52294=SURFACE_STYLE_FILL_AREA(#52293);
#52295=SURFACE_SIDE_STYLE('',(#52294));
#52296=SURFACE_STYLE_USAGE(.BOTH.,#52295);
#52297=PRESENTATION_STYLE_ASSIGNMENT((#52296));
#52298=COLOUR_RGB('Light Blue',0.38,0.62,0.78);
#52299=FILL_AREA_STYLE_COLOUR('',#52298);
#52300=FILL_AREA_STYLE('',(#52299));
#52301=SURFACE_STYLE_FILL_AREA(#52300);
#52302=SURFACE_SIDE_STYLE('',(#52301));
#52303=SURFACE_STYLE_USAGE(.BOTH.,#52302);
#52304=PRESENTATION_STYLE_ASSIGNMENT((#52303));
#52305=COLOUR_RGB('Sky Blue',0.24,0.69,0.87);
#52306=FILL_AREA_STYLE_COLOUR('',#52305);
#52307=FILL_AREA_STYLE('',(#52306));
#52308=SURFACE_STYLE_FILL_AREA(#52307);
#52309=SURFACE_SIDE_STYLE('',(#52308));
#52310=SURFACE_STYLE_USAGE(.BOTH.,#52309);
#52311=PRESENTATION_STYLE_ASSIGNMENT((#52310));
#52312=COLOUR_RGB('Grey',0.48,0.52,0.57);
#52313=FILL_AREA_STYLE_COLOUR('',#52312);
#52314=FILL_AREA_STYLE('',(#52313));
#52315=SURFACE_STYLE_FILL_AREA(#52314);
#52316=SURFACE_SIDE_STYLE('',(#52315));
#52317=SURFACE_STYLE_USAGE(.BOTH.,#52316);
#52318=PRESENTATION_STYLE_ASSIGNMENT((#52317));
#52319=COLOUR_RGB('Black',0.12,0.14,0.17);
#52320=FILL_AREA_STYLE_COLOUR('',#52319);
#52321=FILL_AREA_STYLE('',(#52320));
#52322=SURFACE_STYLE_FILL_AREA(#52321);
#52323=SURFACE_SIDE_STYLE('',(#52322));
#52324=SURFACE_STYLE_USAGE(.BOTH.,#52323);
#52325=PRESENTATION_STYLE_ASSIGNMENT((#52324));
#52326=COLOUR_RGB('Off White',0.89,0.88,0.83);
#52327=FILL_AREA_STYLE_COLOUR('',#52326);
#52328=FILL_AREA_STYLE('',(#52327));
#52329=SURFACE_STYLE_FILL_AREA(#52328);
#52330=SURFACE_SIDE_STYLE('',(#52329));
#52331=SURFACE_STYLE_USAGE(.BOTH.,#52330);
#52332=PRESENTATION_STYLE_ASSIGNMENT((#52331));
ENDSEC;
END-ISO-10303-21;
